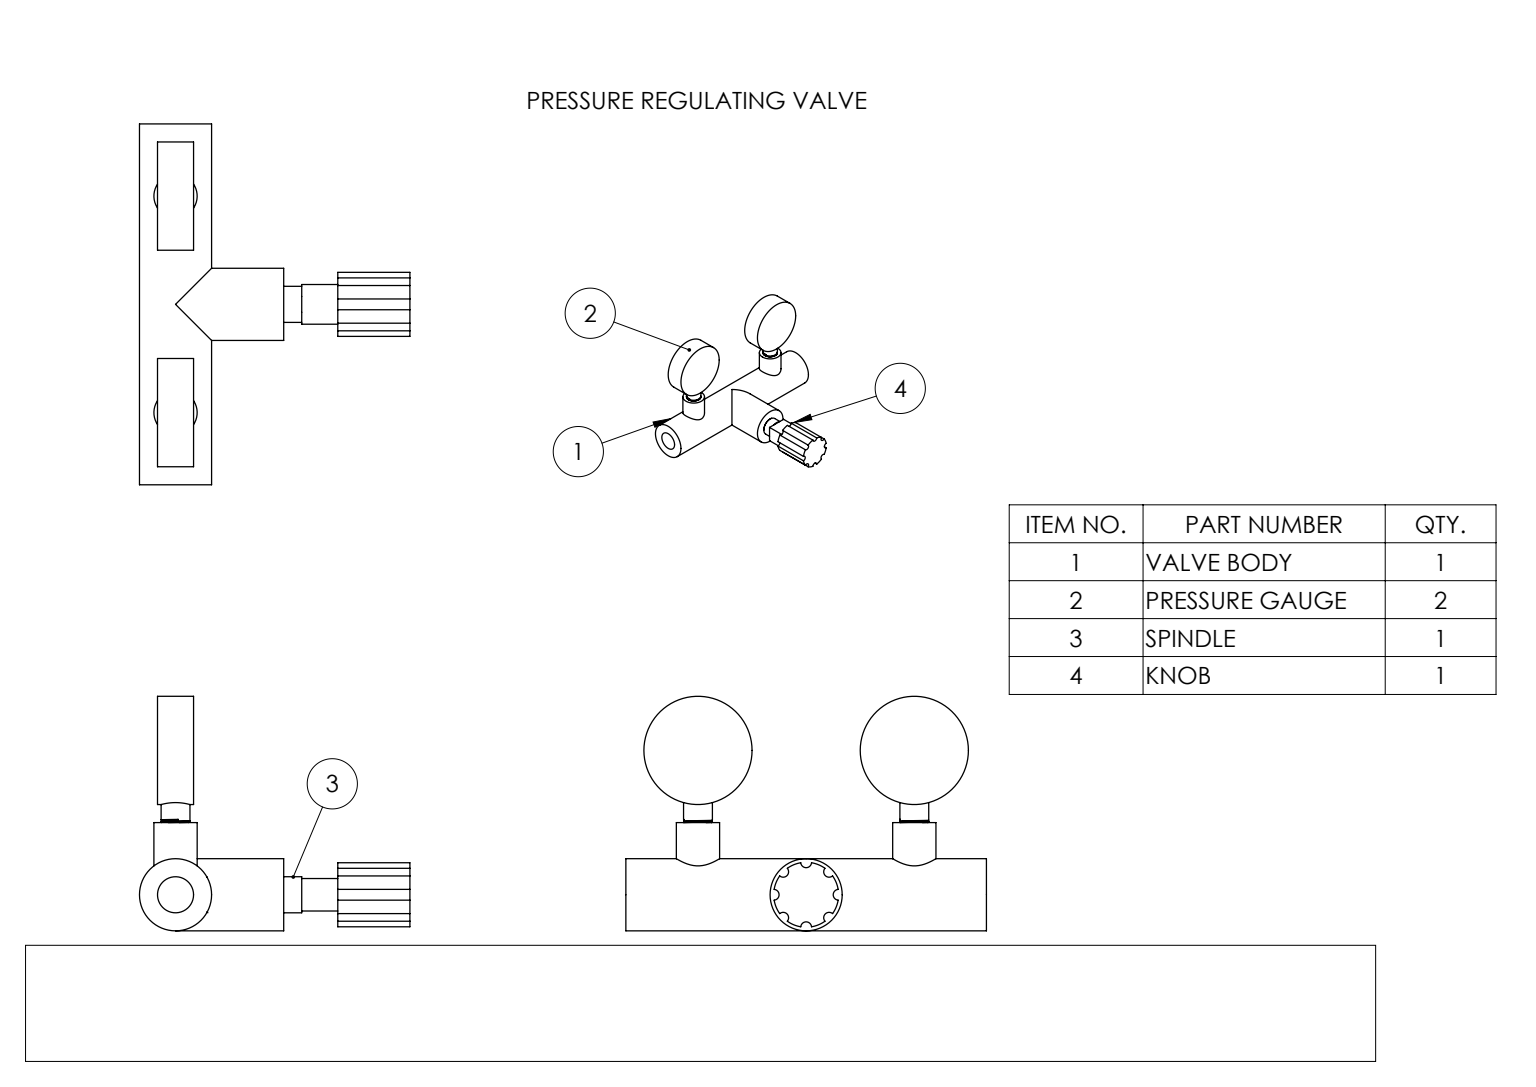
ISO-10303-21;
HEADER;
FILE_DESCRIPTION (('STEP AP214'),
    '1' );
FILE_NAME ('MAS-181',
    '2026-10-26T05:42:23',
    ( '' ),
    ( '' ),
    'SwSTEP 2.0',
    'SolidWorks 2026',
    '' );
FILE_SCHEMA (( 'AUTOMOTIVE_DESIGN' ));
ENDSEC;

DATA;
#1 = CARTESIAN_POINT ( 'NONE',  ( 9.721875000614517148, -6.054752690667223547, -1.112240025338166033E-15 ) ) ;
#2 = CARTESIAN_POINT ( 'NONE',  ( 3.999999999999998668, 14.07500000122903749, -32.30940107675850470 ) ) ;
#3 = CARTESIAN_POINT ( 'NONE',  ( 20.46562500061451928, -6.054752690667223547, -1.112240025338166033E-15 ) ) ;
#4 = CARTESIAN_POINT ( 'NONE',  ( -5.810221930991193690E-16, 14.48749999999999893, 26.00000000000000355 ) ) ;
#5 = CARTESIAN_POINT ( 'NONE',  ( 2.121784821875001281, 17.25312500061459176, 33.67503911421598417 ) ) ;
#6 = CARTESIAN_POINT ( 'NONE',  ( 21.83437500061451786, -4.541064518000419881, 2.621784821874995952 ) ) ;
#7 = CARTESIAN_POINT ( 'NONE',  ( 45.00000000000000000, 0.000000000000000000, 0.000000000000000000 ) ) ;
#8 = CARTESIAN_POINT ( 'NONE',  ( 27.97500000122903074, -5.773502691896255534, -1.060575238724906372E-15 ) ) ;
#9 = CARTESIAN_POINT ( 'NONE',  ( 19.58437500061451786, -2.746126346562642428, -4.756430356249999214 ) ) ;
#10 = CARTESIAN_POINT ( 'NONE',  ( 24.47812500061451502, -4.541064518000419881, 2.621784821874995952 ) ) ;
#11 = CARTESIAN_POINT ( 'NONE',  ( 15.06562500061451537, -6.054752690667223547, -1.112240025338166033E-15 ) ) ;
#12 = CARTESIAN_POINT ( 'NONE',  ( 15.13125000122903252, 4.330127018922191873, 2.499999999999999556 ) ) ;
#13 = CARTESIAN_POINT ( 'NONE',  ( 10.77187500061451786, 3.027376345333613106, -5.243569643749998122 ) ) ;
#14 = CARTESIAN_POINT ( 'NONE',  ( 27.89999999999999858, -4.330127018922190985, -2.500000000000001332 ) ) ;
#15 = CARTESIAN_POINT ( 'NONE',  ( 25.95000000122903216, 5.773502691896255534, 3.535250795749688894E-16 ) ) ;
#16 = CARTESIAN_POINT ( 'NONE',  ( 3.646875000614520079, 6.054752690667223547, 3.707466751127219781E-16 ) ) ;
#17 = CARTESIAN_POINT ( 'NONE',  ( 13.58437500061451786, 4.541064518000418104, 2.621784821874999949 ) ) ;
#18 = CARTESIAN_POINT ( 'NONE',  ( 28.92187500061451644, 3.027376345333611329, 5.243569643749999010 ) ) ;
#19 = CARTESIAN_POINT ( 'NONE',  ( -5.810221930991193690E-16, 12.23750000000000071, -34.00000000000000000 ) ) ;
#20 = ADVANCED_FACE ( 'NONE', ( #69844 ), #24040, .F. ) ;
#21 = CARTESIAN_POINT ( 'NONE',  ( 18.48750000000000071, -2.886751345948126435, -5.000000000000000000 ) ) ;
#22 = CARTESIAN_POINT ( 'NONE',  ( 23.74687500061451573, -3.027376345333610441, -5.243569643749999898 ) ) ;
#23 = CARTESIAN_POINT ( 'NONE',  ( 13.99687500061451928, 6.054752690667223547, 3.707466751127219781E-16 ) ) ;
#24 = CARTESIAN_POINT ( 'NONE',  ( -7.967954043666661671E-16, 16.24062499938548143, 34.33755215474603517 ) ) ;
#25 = CARTESIAN_POINT ( 'NONE',  ( 28.64999999999999858, 0.000000000000000000, 4.999999999999998224 ) ) ;
#26 = CARTESIAN_POINT ( 'NONE',  ( 3.000000001229032875, 5.773502691896255534, 3.535250795749688894E-16 ) ) ;
#27 = CARTESIAN_POINT ( 'NONE',  ( 7.396875000614516082, -4.119189519843965641, -2.378215178125001383 ) ) ;
#28 = CARTESIAN_POINT ( 'NONE',  ( 18.25312500061451715, -4.541064518000417216, -2.621784821875001281 ) ) ;
#29 = CARTESIAN_POINT ( 'NONE',  ( 5.962500000000002132, 2.886751345948129099, -4.999999999999998224 ) ) ;
#30 = CARTESIAN_POINT ( 'NONE',  ( 13.68750000122903288, 6.123233995736764310E-16, -4.999999999999998224 ) ) ;
#31 = CARTESIAN_POINT ( 'NONE',  ( 16.08749999999999503, -2.886751345948129988, 4.999999999999997335 ) ) ;
#32 = CARTESIAN_POINT ( 'NONE',  ( -4.243569643749999898, 13.05312500061451786, 30.00000000000000000 ) ) ;
#33 = CARTESIAN_POINT ( 'NONE',  ( -5.810221930991193690E-16, 11.78749999999999964, 26.00000000000000355 ) ) ;
#34 = CARTESIAN_POINT ( 'NONE',  ( 21.63750000122903572, -4.330127018922194537, 2.499999999999995559 ) ) ;
#35 = FACE_OUTER_BOUND ( 'NONE', #55826, .T. ) ;
#36 = CARTESIAN_POINT ( 'NONE',  ( 26.59687500061451360, 6.054752690667223547, 3.707466751127219781E-16 ) ) ;
#37 = ORIENTED_EDGE ( 'NONE', *, *, #44217, .T. ) ;
#38 = CARTESIAN_POINT ( 'NONE',  ( 14.69062500061451537, -3.027376345333610441, -5.243569643749999898 ) ) ;
#39 = CARTESIAN_POINT ( 'NONE',  ( 22.75312500061451360, -4.541064518000417216, -2.621784821875001281 ) ) ;
#40 = CARTESIAN_POINT ( 'NONE',  ( 22.99687500061451573, 6.054752690667223547, 3.707466751127219781E-16 ) ) ;
#41 = CARTESIAN_POINT ( 'NONE',  ( 6.337499999999998579, -2.886751345948125991, -5.000000000000000000 ) ) ;
#42 = CARTESIAN_POINT ( 'NONE',  ( 8.990625000614516082, 6.054752690667223547, 3.707466751127219781E-16 ) ) ;
#43 = CARTESIAN_POINT ( 'NONE',  ( 24.85312500061451502, 0.000000000000000000, 5.243569643749999010 ) ) ;
#44 = CARTESIAN_POINT ( 'NONE',  ( 14.03437500061451715, 4.541064518000418104, 2.621784821874999949 ) ) ;
#45 = CARTESIAN_POINT ( 'NONE',  ( 18.12187500061451573, 3.027376345333611329, 5.243569643749999010 ) ) ;
#46 = PLANE ( 'NONE',  #66233 ) ;
#47 = CARTESIAN_POINT ( 'NONE',  ( -4.243569643749997233, 17.59062500061451928, 32.45002607614398471 ) ) ;
#48 = CARTESIAN_POINT ( 'NONE',  ( 21.78750000122903074, 6.123233995736764310E-16, -4.999999999999998224 ) ) ;
#49 = CARTESIAN_POINT ( 'NONE',  ( 13.88437500061451679, 5.824947211148865298E-16, -4.756430356249998326 ) ) ;
#50 = CARTESIAN_POINT ( 'NONE',  ( 11.39062500061451644, -3.027376345333614438, 5.243569643749998122 ) ) ;
#51 = CARTESIAN_POINT ( 'NONE',  ( 6.684375000614518392, 6.421520780324663323E-16, -5.243569643749999010 ) ) ;
#52 = CARTESIAN_POINT ( 'NONE',  ( 4.284375000614518925, -4.541064518000419881, 2.621784821874995952 ) ) ;
#53 = ORIENTED_EDGE ( 'NONE', *, *, #36827, .F. ) ;
#54 = CARTESIAN_POINT ( 'NONE',  ( 26.82187500061451857, -6.054752690667223547, -1.112240025338166033E-15 ) ) ;
#55 = CARTESIAN_POINT ( 'NONE',  ( 16.45312500061451289, -4.541064518000417216, -2.621784821875001281 ) ) ;
#56 = CARTESIAN_POINT ( 'NONE',  ( 27.82500000122903572, 2.886751345948126879, 4.999999999999999112 ) ) ;
#57 = CARTESIAN_POINT ( 'NONE',  ( 28.45312500061451289, 0.000000000000000000, 5.243569643749999010 ) ) ;
#58 = CARTESIAN_POINT ( 'NONE',  ( 25.02187500061451431, -6.054752690667223547, -1.112240025338166033E-15 ) ) ;
#59 = CARTESIAN_POINT ( 'NONE',  ( 18.14062500061451644, -3.027376345333614438, 5.243569643749998122 ) ) ;
#60 = CARTESIAN_POINT ( 'NONE',  ( 4.243569643749999010, 19.22187500061452070, 27.54997392385601174 ) ) ;
#61 = CARTESIAN_POINT ( 'NONE',  ( 24.92812500061451431, -4.541064518000419881, 2.621784821874995952 ) ) ;
#62 = CARTESIAN_POINT ( 'NONE',  ( 4.087500001229035007, -4.330127018922194537, 2.499999999999995559 ) ) ;
#63 = ORIENTED_EDGE ( 'NONE', *, *, #30962, .F. ) ;
#64 = CARTESIAN_POINT ( 'NONE',  ( 27.89999999999999858, -4.330127018922190985, -2.500000000000001332 ) ) ;
#65 = CARTESIAN_POINT ( 'NONE',  ( -2.828200636599751609E-16, 15.83750000000000036, -34.61880215351700230 ) ) ;
#66 = CARTESIAN_POINT ( 'NONE',  ( -3.756430356250000102, 17.92812499938548498, 30.00000000000000000 ) ) ;
#67 = CARTESIAN_POINT ( 'NONE',  ( 5.784375000614517148, 6.421520780324663323E-16, -5.243569643749999010 ) ) ;
#68 = CARTESIAN_POINT ( 'NONE',  ( 10.07812500061451644, -4.541064518000419881, 2.621784821874995952 ) ) ;
#69 = CARTESIAN_POINT ( 'NONE',  ( 5.859375000614519102, 4.541064518000418104, -2.621784821874998173 ) ) ;
#70 = CARTESIAN_POINT ( 'NONE',  ( 24.22500000122903430, 2.886751345948126879, 4.999999999999999112 ) ) ;
#71 = CARTESIAN_POINT ( 'NONE',  ( 14.70937500061451786, -4.541064518000417216, -2.621784821875001281 ) ) ;
#72 = CARTESIAN_POINT ( 'NONE',  ( 28.86562500061451786, 3.027376345333611329, 5.243569643749999010 ) ) ;
#73 = CARTESIAN_POINT ( 'NONE',  ( 27.67499999999999716, 4.330127018922191873, 2.499999999999999556 ) ) ;
#74 = EDGE_CURVE ( 'NONE', #45106, #54880, #1431, .T. ) ;
#75 = CARTESIAN_POINT ( 'NONE',  ( 3.065625000614517592, 3.027376345333613106, -5.243569643749998122 ) ) ;
#76 = CARTESIAN_POINT ( 'NONE',  ( 12.92812500061451786, 6.421520780324663323E-16, -5.243569643749999010 ) ) ;
#77 = ORIENTED_EDGE ( 'NONE', *, *, #11122, .T. ) ;
#78 = CARTESIAN_POINT ( 'NONE',  ( 8.953125000614518214, 4.541064518000418104, -2.621784821874998173 ) ) ;
#79 = CARTESIAN_POINT ( 'NONE',  ( 5.203125000614518214, -4.541064518000417216, -2.621784821875001281 ) ) ;
#80 = CARTESIAN_POINT ( 'NONE',  ( 19.88437500061451857, 4.119189519843966529, 2.378215178124999607 ) ) ;
#81 = CARTESIAN_POINT ( 'NONE',  ( 14.10000000122903430, -2.886751345948126435, -5.000000000000000000 ) ) ;
#82 = CARTESIAN_POINT ( 'NONE',  ( 14.66249999999999964, 2.886751345948126879, 4.999999999999999112 ) ) ;
#83 = CARTESIAN_POINT ( 'NONE',  ( 15.90937500061451892, 0.000000000000000000, 5.243569643749999010 ) ) ;
#84 = CARTESIAN_POINT ( 'NONE',  ( 11.36250000122903536, -4.330127018922190985, -2.500000000000001332 ) ) ;
#85 = CARTESIAN_POINT ( 'NONE',  ( 19.46249999999999858, 2.886751345948129099, -4.999999999999998224 ) ) ;
#86 = CARTESIAN_POINT ( 'NONE',  ( 21.72187500061451715, 3.027376345333611329, 5.243569643749999010 ) ) ;
#87 = CARTESIAN_POINT ( 'NONE',  ( -3.000416591977282496E-16, 12.94062500061451537, -34.90005215228797653 ) ) ;
#88 = CARTESIAN_POINT ( 'NONE',  ( -3.999999999999999112, 19.88749999999999929, 27.69059892324149530 ) ) ;
#89 = CARTESIAN_POINT ( 'NONE',  ( 24.45937500061451786, -5.492252693125287522, -1.008910452111647106E-15 ) ) ;
#90 = CARTESIAN_POINT ( 'NONE',  ( 27.62812500061451360, -4.541064518000419881, 2.621784821874995952 ) ) ;
#91 = CARTESIAN_POINT ( 'NONE',  ( 25.05000000000000071, 0.000000000000000000, 4.999999999999998224 ) ) ;
#92 = CARTESIAN_POINT ( 'NONE',  ( 29.82187500061451502, 3.027376345333611329, 5.243569643749999010 ) ) ;
#93 = CARTESIAN_POINT ( 'NONE',  ( 25.38749999999999929, 5.773502691896255534, 3.535250795749688894E-16 ) ) ;
#94 = CARTESIAN_POINT ( 'NONE',  ( 8.465625000614515727, 3.027376345333613106, -5.243569643749998122 ) ) ;
#95 = CARTESIAN_POINT ( 'NONE',  ( 27.64687500061451431, -4.119189519843965641, -2.378215178125001383 ) ) ;
#96 = CARTESIAN_POINT ( 'NONE',  ( 19.09687500061451360, -3.027376345333614438, 5.243569643749998122 ) ) ;
#97 = CARTESIAN_POINT ( 'NONE',  ( 11.07187500061451679, 5.824947211148865298E-16, -4.756430356249998326 ) ) ;
#98 = CARTESIAN_POINT ( 'NONE',  ( 4.603125000614518569, 0.000000000000000000, 5.243569643749999010 ) ) ;
#99 = CARTESIAN_POINT ( 'NONE',  ( 10.69687500061451679, -3.027376345333610441, -5.243569643749999898 ) ) ;
#100 = VERTEX_POINT ( 'NONE', #12957 ) ;
#101 = CARTESIAN_POINT ( 'NONE',  ( 22.28437500061451715, -4.541064518000419881, 2.621784821874995952 ) ) ;
#102 = CARTESIAN_POINT ( 'NONE',  ( -1.071796769724496334, 15.72634618820330310, 26.00000000000000355 ) ) ;
#103 = CARTESIAN_POINT ( 'NONE',  ( 28.42499999999999716, 6.123233995736764310E-16, -4.999999999999998224 ) ) ;
#104 =( BOUNDED_CURVE ( )  B_SPLINE_CURVE ( 2, ( #27084, #21157, #20050, #59212, #14521, #42242, #3825 ),
 .UNSPECIFIED., .F., .F. ) 
 B_SPLINE_CURVE_WITH_KNOTS ( ( 3, 2, 2, 3 ),
 ( 0.5700000000000000622, 0.5733333333333334725, 0.5766666666666667718, 0.5800000000000000711 ),
 .UNSPECIFIED. ) 
 CURVE ( )  GEOMETRIC_REPRESENTATION_ITEM ( )  RATIONAL_B_SPLINE_CURVE ( ( 0.9999999999999955591, 0.8660254037844431485, 1.000000000000000000, 0.8660254037844387076, 1.000000000000000000, 0.8660254037844342667, 1.000000000000004441 ) ) 
 REPRESENTATION_ITEM ( '' )  );
#105 = CARTESIAN_POINT ( 'NONE',  ( 5.887500000000000178, -2.886751345948125991, -5.000000000000000000 ) ) ;
#106 = CARTESIAN_POINT ( 'NONE',  ( 14.36250000122903359, 0.000000000000000000, 4.999999999999998224 ) ) ;
#107 = CARTESIAN_POINT ( 'NONE',  ( 1.999999999999998668, 12.31250000122903465, 26.53589838486224650 ) ) ;
#108 = CARTESIAN_POINT ( 'NONE',  ( 18.67500000000000071, 4.330127018922191873, 2.499999999999999556 ) ) ;
#109 = ORIENTED_EDGE ( 'NONE', *, *, #38380, .F. ) ;
#110 = CARTESIAN_POINT ( 'NONE',  ( 12.15000000000000036, -4.330127018922190985, -2.500000000000001332 ) ) ;
#111 = CARTESIAN_POINT ( 'NONE',  ( 26.84062500061451573, -3.027376345333610441, -5.243569643749999898 ) ) ;
#112 = CARTESIAN_POINT ( 'NONE',  ( 16.19999999999999929, -4.330127018922190985, -2.500000000000001332 ) ) ;
#113 = ADVANCED_FACE ( 'NONE', ( #65026 ), #30323, .F. ) ;
#114 = CARTESIAN_POINT ( 'NONE',  ( 10.20000000122903572, 5.773502691896255534, 3.535250795749688894E-16 ) ) ;
#115 = CARTESIAN_POINT ( 'NONE',  ( 8.128125000614515372, 4.541064518000418104, 2.621784821874999949 ) ) ;
#116 = CARTESIAN_POINT ( 'NONE',  ( 9.225000000000001421, 4.330127018922191873, 2.499999999999999556 ) ) ;
#117 = FACE_OUTER_BOUND ( 'NONE', #13285, .T. ) ;
#118 = CARTESIAN_POINT ( 'NONE',  ( 4.243569643749999010, 15.17187500061451644, -32.45002607614398471 ) ) ;
#119 = CARTESIAN_POINT ( 'NONE',  ( 27.00000000122903288, -2.886751345948129988, 4.999999999999997335 ) ) ;
#120 = CARTESIAN_POINT ( 'NONE',  ( 3.756430356250000546, 13.57812499938548711, 27.83122392262697886 ) ) ;
#121 = CARTESIAN_POINT ( 'NONE',  ( 7.162500000000001421, -5.773502691896255534, -1.060575238724906372E-15 ) ) ;
#122 = DIRECTION ( 'NONE',  ( 0.000000000000000000, 0.000000000000000000, -1.000000000000000000 ) ) ;
#123 = ORIENTED_EDGE ( 'NONE', *, *, #29254, .F. ) ;
#124 = CARTESIAN_POINT ( 'NONE',  ( 25.04062500061451502, -3.027376345333610441, -5.243569643749999898 ) ) ;
#125 = CARTESIAN_POINT ( 'NONE',  ( 14.88750000122903394, -4.330127018922194537, 2.499999999999995559 ) ) ;
#126 = CARTESIAN_POINT ( 'NONE',  ( 29.57812500061451644, 6.421520780324663323E-16, -5.243569643749999010 ) ) ;
#127 = CARTESIAN_POINT ( 'NONE',  ( 28.62187500061451573, -6.054752690667223547, -1.112240025338166033E-15 ) ) ;
#128 = CARTESIAN_POINT ( 'NONE',  ( 18.87187500061451573, 3.027376345333613106, -5.243569643749998122 ) ) ;
#129 = CARTESIAN_POINT ( 'NONE',  ( 16.49062500061451786, -3.027376345333610441, -5.243569643749999898 ) ) ;
#130 = CARTESIAN_POINT ( 'NONE',  ( -4.243569643749998122, 10.39062500061459460, -27.54997392385601174 ) ) ;
#131 = CARTESIAN_POINT ( 'NONE',  ( 5.990625000614517859, -3.027376345333614438, 5.243569643749998122 ) ) ;
#132 = CARTESIAN_POINT ( 'NONE',  ( 29.28750000122903074, -4.330127018922194537, 2.499999999999995559 ) ) ;
#133 = CARTESIAN_POINT ( 'NONE',  ( 22.35937500061451644, -4.119189519843965641, -2.378215178125001383 ) ) ;
#134 = CARTESIAN_POINT ( 'NONE',  ( 19.19062500061452070, -3.027376345333610441, -5.243569643749999898 ) ) ;
#135 = CARTESIAN_POINT ( 'NONE',  ( 1.878215178125000495, 19.01562499938548356, 26.74683588394047007 ) ) ;
#136 = CARTESIAN_POINT ( 'NONE',  ( 13.39687500061451608, -3.027376345333610441, -5.243569643749999898 ) ) ;
#137 = CARTESIAN_POINT ( 'NONE',  ( 11.14687500061451608, -3.027376345333610441, -5.243569643749999898 ) ) ;
#138 = CARTESIAN_POINT ( 'NONE',  ( 23.59687500061451715, -3.027376345333614438, 5.243569643749998122 ) ) ;
#139 = ORIENTED_EDGE ( 'NONE', *, *, #5292, .F. ) ;
#140 = CARTESIAN_POINT ( 'NONE',  ( 3.290625000614516793, -3.027376345333614438, 5.243569643749998122 ) ) ;
#141 = CARTESIAN_POINT ( 'NONE',  ( 27.40312500061451573, 4.541064518000418104, -2.621784821874998173 ) ) ;
#142 =( BOUNDED_CURVE ( )  B_SPLINE_CURVE ( 2, ( #31020, #38022, #48390, #19556, #9951, #32488, #65735 ),
 .UNSPECIFIED., .F., .F. ) 
 B_SPLINE_CURVE_WITH_KNOTS ( ( 3, 2, 2, 3 ),
 ( 0.6416666666666668295, 0.6444444444444445974, 0.6472222222222223653, 0.6500000000000001332 ),
 .UNSPECIFIED. ) 
 CURVE ( )  GEOMETRIC_REPRESENTATION_ITEM ( )  RATIONAL_B_SPLINE_CURVE ( ( 0.9999999999999946709, 0.8660254037844440367, 1.000000000000000000, 0.8660254037844387076, 1.000000000000000000, 0.8660254037844333785, 1.000000000000005329 ) ) 
 REPRESENTATION_ITEM ( '' )  );
#143 = CARTESIAN_POINT ( 'NONE',  ( 27.55312500061451786, 0.000000000000000000, 5.243569643749999010 ) ) ;
#144 = CARTESIAN_POINT ( 'NONE',  ( 4.000000000000000000, 12.08750000000000036, -27.69059892324149885 ) ) ;
#145 = CARTESIAN_POINT ( 'NONE',  ( -2.828200636599751609E-16, 16.73750000000000071, 25.38119784648299770 ) ) ;
#146 = CARTESIAN_POINT ( 'NONE',  ( 4.021875000614516082, 3.027376345333613106, -5.243569643749998122 ) ) ;
#147 = CARTESIAN_POINT ( 'NONE',  ( 11.58750000122903501, 4.330127018922191873, 2.499999999999999556 ) ) ;
#148 = CARTESIAN_POINT ( 'NONE',  ( 7.987500001229032698, 4.330127018922191873, 2.499999999999999556 ) ) ;
#149 = CARTESIAN_POINT ( 'NONE',  ( 28.50000000122903288, -2.886751345948125991, -5.000000000000000000 ) ) ;
#150 = CARTESIAN_POINT ( 'NONE',  ( 2.828200636599751609E-16, 18.40624999877096712, 25.38119784648299415 ) ) ;
#151 = CARTESIAN_POINT ( 'NONE',  ( 17.30625000122903145, 4.330127018922192761, -2.499999999999997780 ) ) ;
#152 = CARTESIAN_POINT ( 'NONE',  ( 11.78437500061451892, 4.541064518000418104, 2.621784821874999949 ) ) ;
#153 = CARTESIAN_POINT ( 'NONE',  ( -3.999999999999999112, 17.58124999877096428, 27.69059892324149530 ) ) ;
#154 = CARTESIAN_POINT ( 'NONE',  ( 20.31562500061451715, 3.027376345333611329, 5.243569643749999010 ) ) ;
#155 = CARTESIAN_POINT ( 'NONE',  ( 13.95937500061451786, 4.541064518000418104, -2.621784821874998173 ) ) ;
#156 = CARTESIAN_POINT ( 'NONE',  ( 3.778125000614519280, -4.541064518000419881, 2.621784821874995952 ) ) ;
#157 = CARTESIAN_POINT ( 'NONE',  ( 23.33437500061451786, 6.421520780324663323E-16, -5.243569643749999010 ) ) ;
#158 = CARTESIAN_POINT ( 'NONE',  ( 8.746875000614515727, -3.027376345333614438, 5.243569643749998122 ) ) ;
#159 = CARTESIAN_POINT ( 'NONE',  ( 4.565625000614516260, 3.027376345333611329, 5.243569643749999010 ) ) ;
#160 = CARTESIAN_POINT ( 'NONE',  ( 5.812500000000001776, -5.773502691896255534, -1.060575238724906372E-15 ) ) ;
#161 = CARTESIAN_POINT ( 'NONE',  ( 5.850000001229035185, -2.886751345948129988, 4.999999999999997335 ) ) ;
#162 = CARTESIAN_POINT ( 'NONE',  ( 19.82812500061451644, 4.541064518000418104, 2.621784821874999949 ) ) ;
#163 = EDGE_CURVE ( 'NONE', #39643, #7983, #64627, .T. ) ;
#164 = CARTESIAN_POINT ( 'NONE',  ( 9.000000001229034652, -2.886751345948129988, 4.999999999999997335 ) ) ;
#165 =( BOUNDED_CURVE ( )  B_SPLINE_CURVE ( 2, ( #55772, #22147, #62756, #34675, #57203, #6619, #72393 ),
 .UNSPECIFIED., .F., .F. ) 
 B_SPLINE_CURVE_WITH_KNOTS ( ( 3, 2, 2, 3 ),
 ( 0.06666666666666665186, 0.06944444444444443365, 0.07222222222222218768, 0.07499999999999996947 ),
 .UNSPECIFIED. ) 
 CURVE ( )  GEOMETRIC_REPRESENTATION_ITEM ( )  RATIONAL_B_SPLINE_CURVE ( ( 1.000000000000000666, 0.8660254037844379305, 1.000000000000000000, 0.8660254037844387076, 1.000000000000000000, 0.8660254037844400399, 0.9999999999999986677 ) ) 
 REPRESENTATION_ITEM ( '' )  );
#166 = CARTESIAN_POINT ( 'NONE',  ( 18.47812500061451857, 4.541064518000418104, 2.621784821874999949 ) ) ;
#167 = CARTESIAN_POINT ( 'NONE',  ( 14.35312500061451679, 4.541064518000418104, -2.621784821874998173 ) ) ;
#168 = CARTESIAN_POINT ( 'NONE',  ( 26.67187500061451644, 2.746126346562643317, 4.756430356249998326 ) ) ;
#169 = CARTESIAN_POINT ( 'NONE',  ( 12.71250000000000036, 2.886751345948129099, -4.999999999999998224 ) ) ;
#170 = CARTESIAN_POINT ( 'NONE',  ( 10.16250000122903252, 4.330127018922192761, -2.499999999999997780 ) ) ;
#171 = CARTESIAN_POINT ( 'NONE',  ( 4.603125000614518569, 0.000000000000000000, 5.243569643749999010 ) ) ;
#172 = CARTESIAN_POINT ( 'NONE',  ( 21.45000000122903216, 5.773502691896255534, 3.535250795749688894E-16 ) ) ;
#173 = CARTESIAN_POINT ( 'NONE',  ( 26.25000000000000000, 4.330127018922192761, -2.499999999999997780 ) ) ;
#174 = CARTESIAN_POINT ( 'NONE',  ( 4.243569643749999898, 11.08437500061451786, -30.00000000000000000 ) ) ;
#175 = CARTESIAN_POINT ( 'NONE',  ( 5.587500001229033231, 6.123233995736764310E-16, -4.999999999999998224 ) ) ;
#176 = CARTESIAN_POINT ( 'NONE',  ( 24.07499999999999929, 4.330127018922191873, 2.499999999999999556 ) ) ;
#177 = CARTESIAN_POINT ( 'NONE',  ( 6.487499999999999822, 5.773502691896255534, 3.535250795749688401E-16 ) ) ;
#178 = CARTESIAN_POINT ( 'NONE',  ( 21.38437500061451502, -4.541064518000419881, 2.621784821874995952 ) ) ;
#179 = CARTESIAN_POINT ( 'NONE',  ( 1.999999999999998668, 18.61250000122903359, 26.53589838486224650 ) ) ;
#180 = CARTESIAN_POINT ( 'NONE',  ( 16.34062500061451573, -3.027376345333614438, 5.243569643749998122 ) ) ;
#181 = CARTESIAN_POINT ( 'NONE',  ( 11.11875000122903323, 2.886751345948126879, 4.999999999999999112 ) ) ;
#182 = CARTESIAN_POINT ( 'NONE',  ( 13.19999999999999929, 4.330127018922192761, -2.499999999999997780 ) ) ;
#183 = CARTESIAN_POINT ( 'NONE',  ( -1.071796769724492115, 14.61740381056766402, 34.00000000000000000 ) ) ;
#184 = CARTESIAN_POINT ( 'NONE',  ( 27.12187500061451573, 3.027376345333611329, 5.243569643749999010 ) ) ;
#185 = CARTESIAN_POINT ( 'NONE',  ( 21.27187500061451431, -4.119189519843968306, 2.378215178124996054 ) ) ;
#186 = CARTESIAN_POINT ( 'NONE',  ( 11.54062500061451857, -3.027376345333610441, -5.243569643749999898 ) ) ;
#187 = CARTESIAN_POINT ( 'NONE',  ( 11.67187500061451821, 3.027376345333613106, -5.243569643749998122 ) ) ;
#188 = ORIENTED_EDGE ( 'NONE', *, *, #4935, .T. ) ;
#189 = CARTESIAN_POINT ( 'NONE',  ( -1.999999999999997113, 14.22500000000000142, -26.53589838486224295 ) ) ;
#190 = CARTESIAN_POINT ( 'NONE',  ( 23.54062500061451146, -3.027376345333614438, 5.243569643749998122 ) ) ;
#191 = CARTESIAN_POINT ( 'NONE',  ( 1.071796769724489895, 13.22990381179669939, -34.00000000000000000 ) ) ;
#192 = CARTESIAN_POINT ( 'NONE',  ( 10.74375000122903323, -2.886751345948130876, 4.999999999999996447 ) ) ;
#193 = CARTESIAN_POINT ( 'NONE',  ( 12.00000000000000000, 0.000000000000000000, 4.999999999999998224 ) ) ;
#194 = CARTESIAN_POINT ( 'NONE',  ( 22.72500000122903430, 2.886751345948129099, -4.999999999999998224 ) ) ;
#195 = CARTESIAN_POINT ( 'NONE',  ( 15.70312500061451644, 4.541064518000418104, -2.621784821874998173 ) ) ;
#196 = CARTESIAN_POINT ( 'NONE',  ( 13.05937500061451573, 2.746126346562643317, 4.756430356249998326 ) ) ;
#197 = ORIENTED_EDGE ( 'NONE', *, *, #67048, .T. ) ;
#198 = CARTESIAN_POINT ( 'NONE',  ( 19.98749999999999716, 5.773502691896255534, 3.535250795749688894E-16 ) ) ;
#199 = CARTESIAN_POINT ( 'NONE',  ( 24.78750000000000497, -2.886751345948125991, -5.000000000000000000 ) ) ;
#200 = CARTESIAN_POINT ( 'NONE',  ( 21.42187500061451644, -6.054752690667223547, -1.112240025338166033E-15 ) ) ;
#201 = CARTESIAN_POINT ( 'NONE',  ( 26.20312500061451644, 0.000000000000000000, 5.243569643749999010 ) ) ;
#202 = ORIENTED_EDGE ( 'NONE', *, *, #63479, .F. ) ;
#203 = LINE ( 'NONE', #67793, #8872 ) ;
#204 = CARTESIAN_POINT ( 'NONE',  ( 8.728125000614518569, -4.541064518000419881, 2.621784821874995952 ) ) ;
#205 = CARTESIAN_POINT ( 'NONE',  ( 17.40000000122903145, 5.773502691896255534, 3.535250795749688401E-16 ) ) ;
#206 = CARTESIAN_POINT ( 'NONE',  ( 14.40000000000000036, -4.330127018922190985, -2.500000000000001332 ) ) ;
#207 = CARTESIAN_POINT ( 'NONE',  ( 2.121784821874999061, 17.85312500061451502, 26.32496088578401583 ) ) ;
#208 = CARTESIAN_POINT ( 'NONE',  ( 4.171875000614517326, 3.027376345333611329, 5.243569643749999010 ) ) ;
#209 = CARTESIAN_POINT ( 'NONE',  ( 27.30937500061451573, -4.541064518000417216, -2.621784821875001281 ) ) ;
#210 = ORIENTED_EDGE ( 'NONE', *, *, #33045, .F. ) ;
#211 = CARTESIAN_POINT ( 'NONE',  ( 24.70312500061451644, 4.541064518000418104, -2.621784821874998173 ) ) ;
#212 = CARTESIAN_POINT ( 'NONE',  ( 25.05937500061451573, -4.541064518000417216, -2.621784821875001281 ) ) ;
#213 = CARTESIAN_POINT ( 'NONE',  ( 4.243569643749999898, 19.57812500061459460, -30.00000000000000000 ) ) ;
#214 = CARTESIAN_POINT ( 'NONE',  ( 10.49999999999999822, 4.330127018922192761, -2.499999999999997780 ) ) ;
#215 = CARTESIAN_POINT ( 'NONE',  ( 9.478125000614515017, 4.541064518000418104, 2.621784821874999949 ) ) ;
#216 = CYLINDRICAL_SURFACE ( 'NONE', #71725, 4.000000000000000000 ) ;
#217 = CARTESIAN_POINT ( 'NONE',  ( 13.57500000000000107, 6.123233995736764310E-16, -4.999999999999998224 ) ) ;
#218 = CARTESIAN_POINT ( 'NONE',  ( 27.44062500061451715, 6.054752690667223547, 3.707466751127219781E-16 ) ) ;
#219 = CARTESIAN_POINT ( 'NONE',  ( 29.29687500061451644, 0.000000000000000000, 4.756430356249998326 ) ) ;
#220 = CARTESIAN_POINT ( 'NONE',  ( 12.38437500061451857, -4.119189519843968306, 2.378215178124996054 ) ) ;
#221 = CARTESIAN_POINT ( 'NONE',  ( 3.665625000614517681, 3.027376345333611329, 5.243569643749999010 ) ) ;
#222 = CARTESIAN_POINT ( 'NONE',  ( 19.39687500061451786, 6.054752690667223547, 3.707466751127219781E-16 ) ) ;
#223 = CARTESIAN_POINT ( 'NONE',  ( 9.001249775931846008E-16, 14.57187500061451679, 34.90005215228797653 ) ) ;
#224 = CARTESIAN_POINT ( 'NONE',  ( 19.65937500061451360, -4.541064518000417216, -2.621784821875001281 ) ) ;
#225 = CARTESIAN_POINT ( 'NONE',  ( 29.55937500061451573, -4.541064518000417216, -2.621784821875001281 ) ) ;
#226 = CARTESIAN_POINT ( 'NONE',  ( -4.243569643749999898, 18.47187500061451715, 27.54997392385601529 ) ) ;
#227 = CARTESIAN_POINT ( 'NONE',  ( 10.19062500061451892, -3.027376345333610441, -5.243569643749999898 ) ) ;
#228 = CARTESIAN_POINT ( 'NONE',  ( 3.112500001229034918, 0.000000000000000000, 4.999999999999998224 ) ) ;
#229 = CARTESIAN_POINT ( 'NONE',  ( 7.846875000614518036, -3.027376345333614438, 5.243569643749998122 ) ) ;
#230 = CARTESIAN_POINT ( 'NONE',  ( 16.16250000122903430, 0.000000000000000000, 4.999999999999998224 ) ) ;
#231 = CARTESIAN_POINT ( 'NONE',  ( 8.165625000614516793, 3.027376345333611329, 5.243569643749999010 ) ) ;
#232 = CARTESIAN_POINT ( 'NONE',  ( 11.22187500061451892, 3.027376345333613106, -5.243569643749998122 ) ) ;
#233 = CARTESIAN_POINT ( 'NONE',  ( 18.90000000122902790, -2.886751345948129988, 4.999999999999997335 ) ) ;
#234 = CARTESIAN_POINT ( 'NONE',  ( 8.446875000614518569, -3.027376345333610441, -5.243569643749999898 ) ) ;
#235 = CARTESIAN_POINT ( 'NONE',  ( 9.815625000614518925, 3.027376345333613106, -5.243569643749998122 ) ) ;
#236 = CARTESIAN_POINT ( 'NONE',  ( 5.803125000614517859, 4.541064518000418104, -2.621784821874998173 ) ) ;
#237 = CARTESIAN_POINT ( 'NONE',  ( 23.26875000122903003, 2.886751345948126879, 4.999999999999999112 ) ) ;
#238 = CARTESIAN_POINT ( 'NONE',  ( 20.25937500061451857, 4.541064518000418104, -2.621784821874998173 ) ) ;
#239 = CARTESIAN_POINT ( 'NONE',  ( -5.810221930991193690E-16, 13.25000000122903465, 26.00000000000000355 ) ) ;
#240 = CARTESIAN_POINT ( 'NONE',  ( 26.39062500061451644, -3.027376345333610441, -5.243569643749999898 ) ) ;
#241 = CARTESIAN_POINT ( 'NONE',  ( 12.02812500061451573, 6.421520780324663323E-16, -5.243569643749999010 ) ) ;
#242 = CARTESIAN_POINT ( 'NONE',  ( 28.99687500061451573, -3.027376345333614438, 5.243569643749998122 ) ) ;
#243 = CARTESIAN_POINT ( 'NONE',  ( 2.121784821874999061, 10.25937500061451857, -33.67503911421598417 ) ) ;
#244 = CARTESIAN_POINT ( 'NONE',  ( 12.78750000122903430, 6.123233995736764310E-16, -4.999999999999998224 ) ) ;
#245 = CARTESIAN_POINT ( 'NONE',  ( 28.19062500061451715, -3.027376345333610441, -5.243569643749999898 ) ) ;
#246 = ADVANCED_FACE ( 'NONE', ( #36587 ), #41411, .F. ) ;
#247 = CARTESIAN_POINT ( 'NONE',  ( -2.121784821874999949, 15.22812500061451679, -33.67503911421598417 ) ) ;
#248 = CARTESIAN_POINT ( 'NONE',  ( 15.22500000122903252, 2.886751345948126879, 4.999999999999999112 ) ) ;
#249 = CARTESIAN_POINT ( 'NONE',  ( 13.68750000000000178, 5.773502691896255534, 3.535250795749688894E-16 ) ) ;
#250 = CARTESIAN_POINT ( 'NONE',  ( 21.62812500061451360, 4.541064518000418104, 2.621784821874999949 ) ) ;
#251 = CARTESIAN_POINT ( 'NONE',  ( 8.184375000614515727, 4.541064518000418104, 2.621784821874999949 ) ) ;
#252 = CARTESIAN_POINT ( 'NONE',  ( 7.912500001229033408, 4.330127018922192761, -2.499999999999997780 ) ) ;
#253 = CARTESIAN_POINT ( 'NONE',  ( 17.25000000122903288, -2.886751345948125991, -5.000000000000000000 ) ) ;
#254 = CARTESIAN_POINT ( 'NONE',  ( 13.04062500061451502, 6.054752690667223547, 3.707466751127219781E-16 ) ) ;
#255 = CARTESIAN_POINT ( 'NONE',  ( 16.04062500061451857, -3.027376345333610441, -5.243569643749999898 ) ) ;
#256 = CARTESIAN_POINT ( 'NONE',  ( 27.56250000122902932, -4.330127018922190985, -2.500000000000001332 ) ) ;
#257 = CARTESIAN_POINT ( 'NONE',  ( 21.93750000000000000, -2.886751345948129988, 4.999999999999997335 ) ) ;
#258 = CARTESIAN_POINT ( 'NONE',  ( 24.15937500061451715, -4.541064518000417216, -2.621784821875001281 ) ) ;
#259 = DIRECTION ( 'NONE',  ( -0.000000000000000000, -1.000000000000000000, -0.000000000000000000 ) ) ;
#260 = CARTESIAN_POINT ( 'NONE',  ( 10.42500000122903536, -5.773502691896255534, -1.060575238724906372E-15 ) ) ;
#261 = CARTESIAN_POINT ( 'NONE',  ( 28.28437500061451715, 6.421520780324663323E-16, -5.243569643749999010 ) ) ;
#262 = CARTESIAN_POINT ( 'NONE',  ( 5.146875000614517859, -3.027376345333614438, 5.243569643749998122 ) ) ;
#263 = CARTESIAN_POINT ( 'NONE',  ( 24.59062500061451573, -3.027376345333610441, -5.243569643749999898 ) ) ;
#264 = CARTESIAN_POINT ( 'NONE',  ( -7.967954043666661671E-16, 14.44062499938548250, 34.33755215474603517 ) ) ;
#265 = CARTESIAN_POINT ( 'NONE',  ( -1.999999999999999112, 13.94374999877096677, 26.53589838486224650 ) ) ;
#266 = CARTESIAN_POINT ( 'NONE',  ( 10.69687500061451679, -3.027376345333610441, -5.243569643749999898 ) ) ;
#267 = CARTESIAN_POINT ( 'NONE',  ( 3.999999999999998668, 12.61250000000000249, 27.69059892324149530 ) ) ;
#268 = CARTESIAN_POINT ( 'NONE',  ( 29.09062500061451573, -3.027376345333610441, -5.243569643749999898 ) ) ;
#269 = CARTESIAN_POINT ( 'NONE',  ( 7.321875000614516793, 3.027376345333611329, 5.243569643749999010 ) ) ;
#270 = CARTESIAN_POINT ( 'NONE',  ( 6.825000000000001066, 6.123233995736764310E-16, -4.999999999999998224 ) ) ;
#271 = CARTESIAN_POINT ( 'NONE',  ( 25.24687500061451573, 6.054752690667223547, 3.707466751127219781E-16 ) ) ;
#272 = CARTESIAN_POINT ( 'NONE',  ( 2.121784821874999061, 10.65312500061459566, 26.32496088578401583 ) ) ;
#273 = CARTESIAN_POINT ( 'NONE',  ( 18.56250000000000000, 2.886751345948129099, -4.999999999999998224 ) ) ;
#274 = EDGE_LOOP ( 'NONE', ( #54307, #37100, #57406 ) ) ;
#275 = CARTESIAN_POINT ( 'NONE',  ( 26.84999999999999787, 0.000000000000000000, 4.999999999999998224 ) ) ;
#276 =( BOUNDED_CURVE ( )  B_SPLINE_CURVE ( 2, ( #33865, #44247, #5440, #72677, #27980, #66778, #16868, #50510, #73036 ),
 .UNSPECIFIED., .F., .F. ) 
 B_SPLINE_CURVE_WITH_KNOTS ( ( 3, 2, 2, 2, 3 ),
 ( 0.2916666666666666852, 0.2962962962962962798, 0.3055555555555555802, 0.3148148148148148251, 0.3194444444444444753 ),
 .UNSPECIFIED. ) 
 CURVE ( )  GEOMETRIC_REPRESENTATION_ITEM ( )  RATIONAL_B_SPLINE_CURVE ( ( 0.9330127018922194093, 0.9330127018922197424, 1.000000000000000000, 0.8660254037844387076, 1.000000000000000000, 0.8660254037844387076, 1.000000000000000000, 0.9330127018922189652, 0.9330127018922194093 ) ) 
 REPRESENTATION_ITEM ( '' )  );
#277 = CARTESIAN_POINT ( 'NONE',  ( 28.99687500061451573, -3.027376345333614438, 5.243569643749998122 ) ) ;
#278 = ADVANCED_FACE ( 'NONE', ( #72396 ), #26980, .F. ) ;
#279 = EDGE_LOOP ( 'NONE', ( #33564, #50876, #16388, #71740 ) ) ;
#280 = CARTESIAN_POINT ( 'NONE',  ( 16.45312500061451289, -4.541064518000417216, -2.621784821875001281 ) ) ;
#281 = CARTESIAN_POINT ( 'NONE',  ( 7.565625000614518036, 3.027376345333613106, -5.243569643749998122 ) ) ;
#282 = CARTESIAN_POINT ( 'NONE',  ( 17.89687500061451431, 4.119189519843966529, -2.378215178124998275 ) ) ;
#283 = CARTESIAN_POINT ( 'NONE',  ( 5.821875000614519458, 3.027376345333613106, -5.243569643749998122 ) ) ;
#284 = CARTESIAN_POINT ( 'NONE',  ( 18.93750000122903288, -4.330127018922194537, 2.499999999999995559 ) ) ;
#285 = CARTESIAN_POINT ( 'NONE',  ( 22.64999999999999858, 4.330127018922192761, -2.499999999999997780 ) ) ;
#286 = CARTESIAN_POINT ( 'NONE',  ( 3.275492200589926739, -3.777717676570560901, -3.275492200590059078 ) ) ;
#287 = CARTESIAN_POINT ( 'NONE',  ( 7.734375000614517326, 4.541064518000418104, 2.621784821874999949 ) ) ;
#288 = CARTESIAN_POINT ( 'NONE',  ( 12.60937500061451821, 4.541064518000418104, -2.621784821874998173 ) ) ;
#289 = CARTESIAN_POINT ( 'NONE',  ( 21.60937500061451644, 4.541064518000418104, -2.621784821874998173 ) ) ;
#290 = CARTESIAN_POINT ( 'NONE',  ( -5.810221930991193690E-16, 14.48749999999999893, -34.00000000000000000 ) ) ;
#291 = ORIENTED_EDGE ( 'NONE', *, *, #26409, .F. ) ;
#292 = CARTESIAN_POINT ( 'NONE',  ( 3.909375000614518481, -4.541064518000417216, -2.621784821875001281 ) ) ;
#293 = CARTESIAN_POINT ( 'NONE',  ( 7.696875000614516793, 6.054752690667223547, 3.707466751127219781E-16 ) ) ;
#294 = CARTESIAN_POINT ( 'NONE',  ( 19.46249999999999858, 2.886751345948129099, -4.999999999999998224 ) ) ;
#295 = CARTESIAN_POINT ( 'NONE',  ( 15.06562500061451537, -6.054752690667223547, -1.112240025338166033E-15 ) ) ;
#296 = CARTESIAN_POINT ( 'NONE',  ( -1.999999999999999112, 17.60000000000000142, 26.53589838486224650 ) ) ;
#297 = CARTESIAN_POINT ( 'NONE',  ( 18.22499999999999787, 4.330127018922191873, 2.499999999999999556 ) ) ;
#298 = CARTESIAN_POINT ( 'NONE',  ( 19.05937500061451928, 0.000000000000000000, 4.756430356249998326 ) ) ;
#299 = CARTESIAN_POINT ( 'NONE',  ( 10.90312500061451928, 0.000000000000000000, 5.243569643749999010 ) ) ;
#300 = CARTESIAN_POINT ( 'NONE',  ( 26.89687500061451431, -3.027376345333610441, -5.243569643749999898 ) ) ;
#301 = CARTESIAN_POINT ( 'NONE',  ( 27.90937500061451715, 4.541064518000418104, -2.621784821874998173 ) ) ;
#302 = CARTESIAN_POINT ( 'NONE',  ( 9.750000000000001776, 0.000000000000000000, 4.999999999999998224 ) ) ;
#303 = CARTESIAN_POINT ( 'NONE',  ( -3.999999999999999112, 16.06250000122903288, 30.00000000000000000 ) ) ;
#304 = CARTESIAN_POINT ( 'NONE',  ( 8.475000001229034297, 2.886751345948126879, 4.999999999999999112 ) ) ;
#305 = CARTESIAN_POINT ( 'NONE',  ( 20.63437500061451857, 6.421520780324663323E-16, -5.243569643749999010 ) ) ;
#306 = CARTESIAN_POINT ( 'NONE',  ( 14.70937500061451786, -4.541064518000417216, -2.621784821875001281 ) ) ;
#307 = CARTESIAN_POINT ( 'NONE',  ( 9.999999999999992895, 5.857864376269048989, 9.999999999999992895 ) ) ;
#308 = EDGE_LOOP ( 'NONE', ( #45837, #56679, #50706, #57678 ) ) ;
#309 = CARTESIAN_POINT ( 'NONE',  ( 13.97812500061451679, 4.541064518000418104, 2.621784821874999949 ) ) ;
#310 = CARTESIAN_POINT ( 'NONE',  ( 27.00000000122903288, -2.886751345948129988, 4.999999999999997335 ) ) ;
#311 = CARTESIAN_POINT ( 'NONE',  ( 15.38437500061451679, 4.541064518000418104, 2.621784821874999949 ) ) ;
#312 = CARTESIAN_POINT ( 'NONE',  ( 3.440625000614518036, -3.027376345333610441, -5.243569643749999898 ) ) ;
#313 = CARTESIAN_POINT ( 'NONE',  ( 17.42812500061451786, 6.421520780324663323E-16, -5.243569643749999010 ) ) ;
#314 = ADVANCED_FACE ( 'NONE', ( #9615 ), #38044, .F. ) ;
#315 = FACE_OUTER_BOUND ( 'NONE', #42185, .T. ) ;
#316 = CARTESIAN_POINT ( 'NONE',  ( 25.92187500061451999, -6.054752690667223547, -1.112240025338166033E-15 ) ) ;
#317 = CARTESIAN_POINT ( 'NONE',  ( 2.121784821874999061, 11.10312500061451679, 26.32496088578401583 ) ) ;
#318 = CARTESIAN_POINT ( 'NONE',  ( 16.28437500061452070, 4.541064518000418104, 2.621784821874999949 ) ) ;
#319 = CARTESIAN_POINT ( 'NONE',  ( 13.01250000122903394, 0.000000000000000000, 4.999999999999998224 ) ) ;
#320 = CARTESIAN_POINT ( 'NONE',  ( 30.00000000000000000, 0.000000000000000000, 0.000000000000000000 ) ) ;
#321 = CARTESIAN_POINT ( 'NONE',  ( -2.121784821874999949, 19.78437500061451715, -33.67503911421598417 ) ) ;
#322 = CARTESIAN_POINT ( 'NONE',  ( 18.87187500061451573, 3.027376345333613106, -5.243569643749998122 ) ) ;
#323 = CARTESIAN_POINT ( 'NONE',  ( 19.87500000122903288, -5.773502691896255534, -1.060575238724906372E-15 ) ) ;
#324 = CARTESIAN_POINT ( 'NONE',  ( 14.89687500061451786, 6.054752690667223547, 3.707466751127219781E-16 ) ) ;
#325 = CARTESIAN_POINT ( 'NONE',  ( -2.121784821874996840, 11.38437500061451679, 33.67503911421598417 ) ) ;
#326 = CARTESIAN_POINT ( 'NONE',  ( 21.26250000122903572, -4.330127018922190985, -2.500000000000001332 ) ) ;
#327 = CARTESIAN_POINT ( 'NONE',  ( 14.65312500061451573, -4.541064518000417216, -2.621784821875001281 ) ) ;
#328 = CYLINDRICAL_SURFACE ( 'NONE', #3060, 3.999999999999996447 ) ;
#329 = VERTEX_POINT ( 'NONE', #38418 ) ;
#330 = ORIENTED_EDGE ( 'NONE', *, *, #52495, .F. ) ;
#331 = CARTESIAN_POINT ( 'NONE',  ( 20.54999999999999716, 0.000000000000000000, 4.999999999999998224 ) ) ;
#332 = CARTESIAN_POINT ( 'NONE',  ( 3.482548389542082568, 3.599757532507414481, 32.03236939885417911 ) ) ;
#333 = CARTESIAN_POINT ( 'NONE',  ( 14.85000000122903252, -2.886751345948129988, 4.999999999999997335 ) ) ;
#334 = CARTESIAN_POINT ( 'NONE',  ( 19.52812500061451573, -4.541064518000419881, 2.621784821874995952 ) ) ;
#335 = CARTESIAN_POINT ( 'NONE',  ( 23.24062500061451786, -3.027376345333610441, -5.243569643749999898 ) ) ;
#336 = EDGE_CURVE ( 'NONE', #58790, #48104, #15871, .T. ) ;
#337 = CARTESIAN_POINT ( 'NONE',  ( 5.128125000614516260, -4.541064518000419881, 2.621784821874995952 ) ) ;
#338 =( BOUNDED_CURVE ( )  B_SPLINE_CURVE ( 2, ( #15519, #49887, #72412, #9995, #32529, #66507, #49526 ),
 .UNSPECIFIED., .F., .F. ) 
 B_SPLINE_CURVE_WITH_KNOTS ( ( 3, 2, 2, 3 ),
 ( 0.5083333333333334147, 0.5111111111111110716, 0.5138888888888888395, 0.5166666666666666075 ),
 .UNSPECIFIED. ) 
 CURVE ( )  GEOMETRIC_REPRESENTATION_ITEM ( )  RATIONAL_B_SPLINE_CURVE ( ( 0.9999999999999946709, 0.8660254037844440367, 1.000000000000000000, 0.8660254037844387076, 1.000000000000000000, 0.8660254037844440367, 0.9999999999999946709 ) ) 
 REPRESENTATION_ITEM ( '' )  );
#339 = AXIS2_PLACEMENT_3D ( 'NONE', #22340, #45247, #39713 ) ;
#340 = CARTESIAN_POINT ( 'NONE',  ( 29.06250000000000000, 2.886751345948126879, 4.999999999999999112 ) ) ;
#341 = CARTESIAN_POINT ( 'NONE',  ( -1.626862140677534273E-15, 15.03124999877096535, 34.00000000000000000 ) ) ;
#342 = CARTESIAN_POINT ( 'NONE',  ( 9.946875000614516793, 5.492252693125287522, 3.363034840372157021E-16 ) ) ;
#343 = CYLINDRICAL_SURFACE ( 'NONE', #34692, 4.000000000000000000 ) ;
#344 = CARTESIAN_POINT ( 'NONE',  ( 4.000000000000000000, 10.85000000122903430, -27.69059892324149530 ) ) ;
#345 = CARTESIAN_POINT ( 'NONE',  ( 4.243569643749999010, 17.87187500061451573, -32.45002607614398471 ) ) ;
#346 = CARTESIAN_POINT ( 'NONE',  ( 6.562500001229032875, 4.330127018922192761, -2.499999999999997780 ) ) ;
#347 = CARTESIAN_POINT ( 'NONE',  ( 8.737500000000002487, 5.773502691896255534, 3.535250795749688894E-16 ) ) ;
#348 = CARTESIAN_POINT ( 'NONE',  ( 3.787500001229033408, 6.123233995736764310E-16, -4.999999999999998224 ) ) ;
#349 = CARTESIAN_POINT ( 'NONE',  ( 11.74687500061451573, 6.054752690667223547, 3.707466751127219781E-16 ) ) ;
#350 = CARTESIAN_POINT ( 'NONE',  ( 4.057522967627288146, -2.921730200955767298, 4.057522967627288146 ) ) ;
#351 = CARTESIAN_POINT ( 'NONE',  ( 4.396875000614516971, -3.027376345333610441, -5.243569643749999898 ) ) ;
#352 = CARTESIAN_POINT ( 'NONE',  ( 12.90000000122903323, 5.773502691896255534, 3.535250795749688401E-16 ) ) ;
#353 = CARTESIAN_POINT ( 'NONE',  ( 4.000000000000000000, 19.40000000122903856, 32.30940107675849760 ) ) ;
#354 = CARTESIAN_POINT ( 'NONE',  ( 10.84687500061451892, 6.054752690667223547, 3.707466751127219781E-16 ) ) ;
#355 = CARTESIAN_POINT ( 'NONE',  ( 14.48437500061451821, 4.541064518000418104, 2.621784821874999949 ) ) ;
#356 = CARTESIAN_POINT ( 'NONE',  ( 3.609349942001692124, -3.970247583483341280, -3.123329466779292130 ) ) ;
#357 = CARTESIAN_POINT ( 'NONE',  ( 2.121784821874999061, 16.50312500061459176, 26.32496088578401583 ) ) ;
#358 = CARTESIAN_POINT ( 'NONE',  ( 21.15937500061451715, 4.541064518000418104, -2.621784821874998173 ) ) ;
#359 = CARTESIAN_POINT ( 'NONE',  ( 26.92500000122903359, 2.886751345948126879, 4.999999999999999112 ) ) ;
#360 = CARTESIAN_POINT ( 'NONE',  ( 18.38437500061451502, 5.492252693125287522, 3.363034840372157021E-16 ) ) ;
#361 = CARTESIAN_POINT ( 'NONE',  ( 22.52812500061451573, 4.541064518000418104, 2.621784821874999949 ) ) ;
#362 = CARTESIAN_POINT ( 'NONE',  ( 15.85312500061451857, 0.000000000000000000, 5.243569643749999010 ) ) ;
#363 = CARTESIAN_POINT ( 'NONE',  ( 26.67187500061451289, -4.119189519843968306, 2.378215178124996054 ) ) ;
#364 = CARTESIAN_POINT ( 'NONE',  ( 11.55937500061451928, -4.541064518000417216, -2.621784821875001281 ) ) ;
#365 = CARTESIAN_POINT ( 'NONE',  ( 29.73750000000000071, -2.886751345948125991, -5.000000000000000000 ) ) ;
#366 = CARTESIAN_POINT ( 'NONE',  ( 24.75000000122902932, -2.886751345948129988, 4.999999999999997335 ) ) ;
#367 = CARTESIAN_POINT ( 'NONE',  ( 4.659375000614518925, 0.000000000000000000, 5.243569643749999010 ) ) ;
#368 = CARTESIAN_POINT ( 'NONE',  ( 14.93437500061451750, 4.541064518000418104, 2.621784821874999949 ) ) ;
#369 = CARTESIAN_POINT ( 'NONE',  ( 29.70937500061451431, 4.541064518000418104, -2.621784821874998173 ) ) ;
#370 = CARTESIAN_POINT ( 'NONE',  ( 3.070561448845197550, -4.159287105319667610, 2.795903410320249360 ) ) ;
#371 = FACE_OUTER_BOUND ( 'NONE', #14066, .T. ) ;
#372 = CARTESIAN_POINT ( 'NONE',  ( 22.84687500061451715, -3.027376345333610441, -5.243569643749999898 ) ) ;
#373 = CARTESIAN_POINT ( 'NONE',  ( 14.82187500061451679, 3.027376345333613106, -5.243569643749998122 ) ) ;
#374 = CARTESIAN_POINT ( 'NONE',  ( -1.878215178125001827, 14.85312499938548214, 33.25316411605952283 ) ) ;
#375 = CARTESIAN_POINT ( 'NONE',  ( 25.76249999999999929, 2.886751345948129099, -4.999999999999998224 ) ) ;
#376 = CARTESIAN_POINT ( 'NONE',  ( 4.350000001229033408, 5.773502691896255534, 3.535250795749688894E-16 ) ) ;
#377 = CARTESIAN_POINT ( 'NONE',  ( 7.696875000614517681, 0.000000000000000000, 4.756430356249998326 ) ) ;
#378 = CARTESIAN_POINT ( 'NONE',  ( 16.26562500061451289, 3.027376345333611329, 5.243569643749999010 ) ) ;
#379 = CARTESIAN_POINT ( 'NONE',  ( 7.687500000000000000, -2.886751345948125991, -5.000000000000000000 ) ) ;
#380 = EDGE_CURVE ( 'NONE', #38892, #55608, #31618, .T. ) ;
#381 = CARTESIAN_POINT ( 'NONE',  ( 13.65000000122903323, -2.886751345948193048, -4.999999999999883649 ) ) ;
#382 = CARTESIAN_POINT ( 'NONE',  ( 16.80000000000000071, 4.330127018922192761, -2.499999999999997780 ) ) ;
#383 = CARTESIAN_POINT ( 'NONE',  ( -4.243569643749999898, 13.95312500061451821, 30.00000000000000000 ) ) ;
#384 = CARTESIAN_POINT ( 'NONE',  ( 24.84375000122903288, -2.886751345948153968, -4.999999999999952038 ) ) ;
#385 = CARTESIAN_POINT ( 'NONE',  ( 20.88750000122903572, 6.123233995736764310E-16, -4.999999999999998224 ) ) ;
#386 = CARTESIAN_POINT ( 'NONE',  ( 11.38125000122903252, 6.123233995736764310E-16, -4.999999999999998224 ) ) ;
#387 = CARTESIAN_POINT ( 'NONE',  ( 26.18437500061451573, 4.541064518000418104, 2.621784821874999949 ) ) ;
#388 = ORIENTED_EDGE ( 'NONE', *, *, #31467, .F. ) ;
#389 = CARTESIAN_POINT ( 'NONE',  ( 21.36562500061451431, -6.054752690667223547, -1.112240025338166033E-15 ) ) ;
#390 = CARTESIAN_POINT ( 'NONE',  ( 21.72187500061451715, 3.027376345333611329, 5.243569643749999010 ) ) ;
#391 = CARTESIAN_POINT ( 'NONE',  ( 6.787500000000001421, -2.886751345948125991, -5.000000000000000000 ) ) ;
#392 = CARTESIAN_POINT ( 'NONE',  ( 8.915625000614515017, 3.027376345333613106, -5.243569643749998122 ) ) ;
#393 = CARTESIAN_POINT ( 'NONE',  ( 23.46562500061451573, 3.027376345333611329, 5.243569643749999010 ) ) ;
#394 = CARTESIAN_POINT ( 'NONE',  ( 12.72187500061451537, 3.027376345333611329, 5.243569643749999010 ) ) ;
#395 = CARTESIAN_POINT ( 'NONE',  ( 16.80937500061451573, 0.000000000000000000, 5.243569643749999010 ) ) ;
#396 = CARTESIAN_POINT ( 'NONE',  ( 19.20000000000000284, 0.000000000000000000, 4.999999999999998224 ) ) ;
#397 = CARTESIAN_POINT ( 'NONE',  ( 4.243569643749999898, 17.74062500061451786, 32.45002607614398471 ) ) ;
#398 = CARTESIAN_POINT ( 'NONE',  ( 21.60000000122903430, -2.886751345948129988, 4.999999999999997335 ) ) ;
#399 = CARTESIAN_POINT ( 'NONE',  ( 15.08437500061451786, -4.119189519843968306, 2.378215178124996054 ) ) ;
#400 = CARTESIAN_POINT ( 'NONE',  ( 11.16562500061451679, 3.027376345333612662, -5.243569643749998122 ) ) ;
#401 = CARTESIAN_POINT ( 'NONE',  ( 4.959375000614516971, 4.541064518000418104, -2.621784821874998173 ) ) ;
#402 = CARTESIAN_POINT ( 'NONE',  ( 4.059375000614519280, 4.541064518000418104, -2.621784821874998173 ) ) ;
#403 = VERTEX_POINT ( 'NONE', #43241 ) ;
#404 = CARTESIAN_POINT ( 'NONE',  ( 24.68437500061451573, 6.421520780324663323E-16, -5.243569643749999010 ) ) ;
#405 = CARTESIAN_POINT ( 'NONE',  ( 16.15312500061451573, 4.541064518000418104, -2.621784821874998173 ) ) ;
#406 = CARTESIAN_POINT ( 'NONE',  ( 27.26250000122903216, 4.330127018922192761, -2.499999999999997780 ) ) ;
#407 = CARTESIAN_POINT ( 'NONE',  ( 28.60312500061451502, -4.541064518000417216, -2.621784821875001281 ) ) ;
#408 = CARTESIAN_POINT ( 'NONE',  ( 21.98437500061451644, 6.421520780324663323E-16, -5.243569643749999010 ) ) ;
#409 = CARTESIAN_POINT ( 'NONE',  ( 16.22812500061451857, 4.541064518000418104, 2.621784821874999949 ) ) ;
#410 = CARTESIAN_POINT ( 'NONE',  ( 4.243569643749999898, 19.63437500061451857, 30.00000000000000000 ) ) ;
#411 = CARTESIAN_POINT ( 'NONE',  ( 22.94062500061451715, 6.054752690667223547, 3.707466751127219781E-16 ) ) ;
#412 = CARTESIAN_POINT ( 'NONE',  ( 3.825000001229032609, 2.886751345948129099, -4.999999999999998224 ) ) ;
#413 = ORIENTED_EDGE ( 'NONE', *, *, #34178, .T. ) ;
#414 = CARTESIAN_POINT ( 'NONE',  ( 28.57499999999999929, 4.330127018922191873, 2.499999999999999556 ) ) ;
#415 = CARTESIAN_POINT ( 'NONE',  ( -2.000000000000000000, 13.17500000000000071, -33.46410161513775705 ) ) ;
#416 = CARTESIAN_POINT ( 'NONE',  ( 2.655984681222220721E-16, 16.46562499938548285, 25.66244784525396483 ) ) ;
#417 = CARTESIAN_POINT ( 'NONE',  ( 29.09062500061451573, -3.027376345333610441, -5.243569643749999898 ) ) ;
#418 = CARTESIAN_POINT ( 'NONE',  ( 9.253125000614517148, -4.541064518000417216, -2.621784821875001281 ) ) ;
#419 = CARTESIAN_POINT ( 'NONE',  ( 21.22500000122903074, -5.773502691896255534, -1.060575238724906372E-15 ) ) ;
#420 = EDGE_CURVE ( 'NONE', #14890, #16300, #13688, .T. ) ;
#421 = CARTESIAN_POINT ( 'NONE',  ( 12.68437500061451573, 4.541064518000418104, 2.621784821874999949 ) ) ;
#422 = CARTESIAN_POINT ( 'NONE',  ( 28.07812500061451289, -4.541064518000419881, 2.621784821874995952 ) ) ;
#423 = CARTESIAN_POINT ( 'NONE',  ( 27.29999999999999716, 0.000000000000000000, 4.999999999999998224 ) ) ;
#424 = CARTESIAN_POINT ( 'NONE',  ( 4.000000000000000000, 17.60000000122903785, -27.69059892324149530 ) ) ;
#425 = CARTESIAN_POINT ( 'NONE',  ( -1.487416814333745711E-14, 15.72500000122903430, -26.00000000000000000 ) ) ;
#426 = CARTESIAN_POINT ( 'NONE',  ( 12.10312500061451857, 4.541064518000418104, -2.621784821874998173 ) ) ;
#427 = VERTEX_POINT ( 'NONE', #4808 ) ;
#428 = CARTESIAN_POINT ( 'NONE',  ( 11.16562500061451679, 3.027376345333613106, -5.243569643749998122 ) ) ;
#429 = CARTESIAN_POINT ( 'NONE',  ( 6.253125000614517148, 4.541064518000418104, -2.621784821874998173 ) ) ;
#430 = CARTESIAN_POINT ( 'NONE',  ( 17.37187500061451573, -5.492252693125287522, -1.008910452111647106E-15 ) ) ;
#431 = EDGE_CURVE ( 'NONE', #55385, #17600, #60203, .T. ) ;
#432 = CARTESIAN_POINT ( 'NONE',  ( 14.53125000122903288, 6.123233995736764310E-16, -4.999999999999998224 ) ) ;
#433 = CARTESIAN_POINT ( 'NONE',  ( 15.90000000000000036, 4.330127018922192761, -2.499999999999997780 ) ) ;
#434 = CARTESIAN_POINT ( 'NONE',  ( 16.54687500061451644, -3.027376345333610441, -5.243569643749999898 ) ) ;
#435 = CARTESIAN_POINT ( 'NONE',  ( 10.98750000122903536, 6.123233995736764310E-16, -4.999999999999998224 ) ) ;
#436 = CARTESIAN_POINT ( 'NONE',  ( 18.79687500061451644, -3.027376345333610441, -5.243569643749999898 ) ) ;
#437 = CARTESIAN_POINT ( 'NONE',  ( 18.67500000000000071, 4.330127018922191873, 2.499999999999999556 ) ) ;
#438 = CARTESIAN_POINT ( 'NONE',  ( 19.73437500061451644, 6.421520780324663323E-16, -5.243569643749999010 ) ) ;
#439 = CARTESIAN_POINT ( 'NONE',  ( -2.121784821874996840, 14.92812500061451608, -26.32496088578401583 ) ) ;
#440 = CARTESIAN_POINT ( 'NONE',  ( 1.071796769724497445, 16.71740381056766367, 26.00000000000000355 ) ) ;
#441 = CARTESIAN_POINT ( 'NONE',  ( 26.14687500061451431, 0.000000000000000000, 4.756430356249998326 ) ) ;
#442 = CARTESIAN_POINT ( 'NONE',  ( 18.39375000122902648, -2.886751345948074920, 5.000000000000092371 ) ) ;
#443 = CARTESIAN_POINT ( 'NONE',  ( 27.66562500061451146, -6.054752690667223547, -1.112240025338166033E-15 ) ) ;
#444 = SURFACE_STYLE_FILL_AREA ( #52132 ) ;
#445 = CARTESIAN_POINT ( 'NONE',  ( 29.14687500061451075, -3.027376345333610441, -5.243569643749999898 ) ) ;
#446 = EDGE_CURVE ( 'NONE', #17600, #24863, #53958, .T. ) ;
#447 = CARTESIAN_POINT ( 'NONE',  ( 25.01249999999999929, 2.886751345948126879, 4.999999999999999112 ) ) ;
#448 = CARTESIAN_POINT ( 'NONE',  ( 9.478125000614515017, 4.541064518000418104, 2.621784821874999949 ) ) ;
#449 = CARTESIAN_POINT ( 'NONE',  ( 25.02187500061451431, 5.824947211148865298E-16, -4.756430356249998326 ) ) ;
#450 = CARTESIAN_POINT ( 'NONE',  ( 19.50937500061451857, 0.000000000000000000, 5.243569643749999010 ) ) ;
#451 = CARTESIAN_POINT ( 'NONE',  ( 11.10937500061451644, 2.746126346562645981, -4.756430356249997438 ) ) ;
#452 = CARTESIAN_POINT ( 'NONE',  ( 6.440625000614517148, -3.027376345333614438, 5.243569643749998122 ) ) ;
#453 = CARTESIAN_POINT ( 'NONE',  ( 11.07187500061451679, -6.054752690667223547, -1.112240025338166033E-15 ) ) ;
#454 = ORIENTED_EDGE ( 'NONE', *, *, #66600, .F. ) ;
#455 = CARTESIAN_POINT ( 'NONE',  ( 22.54687500061451999, 6.054752690667223547, 3.707466751127219781E-16 ) ) ;
#456 = CARTESIAN_POINT ( 'NONE',  ( 45.00000000000000000, 6.123233995736764310E-16, -4.999999999999998224 ) ) ;
#457 = CARTESIAN_POINT ( 'NONE',  ( 17.00625000122903074, 0.000000000000000000, 4.999999999999998224 ) ) ;
#458 = EDGE_CURVE ( 'NONE', #51815, #43576, #43970, .T. ) ;
#459 = CARTESIAN_POINT ( 'NONE',  ( 3.862500000000001155, 2.886751345948126879, 4.999999999999999112 ) ) ;
#460 = CARTESIAN_POINT ( 'NONE',  ( 14.73750000122903359, 4.330127018922191873, 2.499999999999999556 ) ) ;
#461 = CYLINDRICAL_SURFACE ( 'NONE', #51393, 4.999999999999998224 ) ;
#462 = LINE ( 'NONE', #60676, #9126 ) ;
#463 = ORIENTED_EDGE ( 'NONE', *, *, #9642, .F. ) ;
#464 = CARTESIAN_POINT ( 'NONE',  ( 13.23750000000000071, 5.773502691896255534, 3.535250795749688894E-16 ) ) ;
#465 = CARTESIAN_POINT ( 'NONE',  ( 13.69687500061451679, -4.119189519843965641, -2.378215178125001383 ) ) ;
#466 = CARTESIAN_POINT ( 'NONE',  ( 25.15312500061451217, 4.541064518000418104, -2.621784821874998173 ) ) ;
#467 = CARTESIAN_POINT ( 'NONE',  ( 14.62500000000000000, 4.330127018922191873, 2.499999999999999556 ) ) ;
#468 = CARTESIAN_POINT ( 'NONE',  ( 11.25000000122903288, -2.886751345948129988, 4.999999999999997335 ) ) ;
#469 = CARTESIAN_POINT ( 'NONE',  ( 10.00312500061451715, 0.000000000000000000, 5.243569643749999010 ) ) ;
#470 = CARTESIAN_POINT ( 'NONE',  ( 9.825000000000001066, -4.330127018922194537, 2.499999999999995559 ) ) ;
#471 = CARTESIAN_POINT ( 'NONE',  ( 4.898734551532200499, 1.001199177798645534, 4.898734551532191617 ) ) ;
#472 = CARTESIAN_POINT ( 'NONE',  ( 26.81250000122903288, 4.330127018922192761, -2.499999999999997780 ) ) ;
#473 = CARTESIAN_POINT ( 'NONE',  ( 1.878215178125000495, 18.11562499938548498, 26.74683588394047007 ) ) ;
#474 = CARTESIAN_POINT ( 'NONE',  ( 8.362500000000002487, 2.886751345948126879, 4.999999999999999112 ) ) ;
#475 = CARTESIAN_POINT ( 'NONE',  ( 18.86249999999999716, -5.773502691896255534, -1.060575238724906372E-15 ) ) ;
#476 = ORIENTED_EDGE ( 'NONE', *, *, #37237, .F. ) ;
#477 = CARTESIAN_POINT ( 'NONE',  ( 22.90312500061451573, 4.541064518000418104, -2.621784821874998173 ) ) ;
#478 = CARTESIAN_POINT ( 'NONE',  ( 28.37812500061451715, 4.541064518000418104, 2.621784821874999949 ) ) ;
#479 = CARTESIAN_POINT ( 'NONE',  ( 4.898587196589411843E-16, 20.00000000000000000, -26.00000000000000000 ) ) ;
#480 = CARTESIAN_POINT ( 'NONE',  ( 19.05937500061451928, 0.000000000000000000, 5.243569643749999010 ) ) ;
#481 = CARTESIAN_POINT ( 'NONE',  ( 17.65312500061451573, 0.000000000000000000, 5.243569643749999010 ) ) ;
#482 = CARTESIAN_POINT ( 'NONE',  ( 4.243569643749999898, 11.47812500061459318, -30.00000000000000000 ) ) ;
#483 = CARTESIAN_POINT ( 'NONE',  ( 6.328125000614515550, 4.541064518000418104, 2.621784821874999949 ) ) ;
#484 = CARTESIAN_POINT ( 'NONE',  ( 29.21250000122903145, 0.000000000000000000, 4.999999999999998224 ) ) ;
#485 = CARTESIAN_POINT ( 'NONE',  ( 21.53437500061451715, 5.824947211148865298E-16, -4.756430356249998326 ) ) ;
#486 = CARTESIAN_POINT ( 'NONE',  ( 18.17812500061451786, -4.541064518000419881, 2.621784821874995952 ) ) ;
#487 = CARTESIAN_POINT ( 'NONE',  ( 1.999999999999998668, 11.41250000122903430, -33.46410161513775705 ) ) ;
#488 = CARTESIAN_POINT ( 'NONE',  ( 3.375000001229033320, 2.886751345948129099, -4.999999999999998224 ) ) ;
#489 =( BOUNDED_CURVE ( )  B_SPLINE_CURVE ( 2, ( #20921, #14646, #9118, #48647, #21286, #33107, #71172 ),
 .UNSPECIFIED., .F., .F. ) 
 B_SPLINE_CURVE_WITH_KNOTS ( ( 3, 2, 2, 3 ),
 ( 0.3500000000000000888, 0.3533333333333333881, 0.3566666666666667429, 0.3599999999999999867 ),
 .UNSPECIFIED. ) 
 CURVE ( )  GEOMETRIC_REPRESENTATION_ITEM ( )  RATIONAL_B_SPLINE_CURVE ( ( 0.9999999999999955591, 0.8660254037844431485, 1.000000000000000000, 0.8660254037844387076, 1.000000000000000000, 0.8660254037844387076, 1.000000000000000000 ) ) 
 REPRESENTATION_ITEM ( '' )  );
#490 = CARTESIAN_POINT ( 'NONE',  ( 13.13437500061451857, 4.541064518000418104, 2.621784821874999949 ) ) ;
#491 = CARTESIAN_POINT ( 'NONE',  ( 12.68437500061451573, 4.541064518000418104, 2.621784821874999949 ) ) ;
#492 = CARTESIAN_POINT ( 'NONE',  ( 20.67187500061451289, 3.027376345333613106, -5.243569643749998122 ) ) ;
#493 = VERTEX_POINT ( 'NONE', #59846 ) ;
#494 = CARTESIAN_POINT ( 'NONE',  ( -0.8062380997993553455, 9.975217491784283297, 24.04105076033751942 ) ) ;
#495 = CARTESIAN_POINT ( 'NONE',  ( 23.91562500061451502, 3.027376345333611329, 5.243569643749999010 ) ) ;
#496 = CARTESIAN_POINT ( 'NONE',  ( 18.00937500061451502, 4.541064518000418104, -2.621784821874998173 ) ) ;
#497 = CARTESIAN_POINT ( 'NONE',  ( 25.30312500061451431, 0.000000000000000000, 5.243569643749999010 ) ) ;
#498 = CARTESIAN_POINT ( 'NONE',  ( -4.000000000000000000, 17.16874999877096641, 30.00000000000000000 ) ) ;
#499 = CARTESIAN_POINT ( 'NONE',  ( -3.999999999999999112, 15.94999999999999929, 30.00000000000000000 ) ) ;
#500 = CARTESIAN_POINT ( 'NONE',  ( 3.871875000614519280, -6.054752690667223547, -1.112240025338166033E-15 ) ) ;
#501 = ITEM_DEFINED_TRANSFORMATION ( 'NONE', 'NONE', #6134,  #23765 ) ;
#502 = CARTESIAN_POINT ( 'NONE',  ( 10.95000000122903394, -2.886751345948125991, -5.000000000000000000 ) ) ;
#503 = CARTESIAN_POINT ( 'NONE',  ( 7.612500001229035362, 0.000000000000000000, 4.999999999999998224 ) ) ;
#504 = CARTESIAN_POINT ( 'NONE',  ( 10.20000000000000107, 0.000000000000000000, 4.999999999999998224 ) ) ;
#505 = CARTESIAN_POINT ( 'NONE',  ( 27.56250000122902932, -4.330127018922190985, -2.500000000000001332 ) ) ;
#506 = CARTESIAN_POINT ( 'NONE',  ( 4.000000000000000000, 17.88124999877096855, 27.69059892324149530 ) ) ;
#507 = CARTESIAN_POINT ( 'NONE',  ( 16.66875000122903216, -5.773502691896255534, -1.060575238724906372E-15 ) ) ;
#508 = CARTESIAN_POINT ( 'NONE',  ( 9.009375000614518569, 4.541064518000418104, -2.621784821874998173 ) ) ;
#509 = CARTESIAN_POINT ( 'NONE',  ( 29.67656250092177217, 0.000000000000000000, 4.878215178124998275 ) ) ;
#510 = CARTESIAN_POINT ( 'NONE',  ( 16.37812500061451715, -4.541064518000419881, 2.621784821874995952 ) ) ;
#511 = CARTESIAN_POINT ( 'NONE',  ( 12.57187500061451857, 3.027376345333613106, -5.243569643749998122 ) ) ;
#512 = CARTESIAN_POINT ( 'NONE',  ( 5.765625000614519102, 3.027376345333613106, -5.243569643749998122 ) ) ;
#513 = CARTESIAN_POINT ( 'NONE',  ( 20.25937500061451857, 4.541064518000418104, -2.621784821874998173 ) ) ;
#514 = CARTESIAN_POINT ( 'NONE',  ( 10.65937500061451715, -4.541064518000417216, -2.621784821875001281 ) ) ;
#515 = CARTESIAN_POINT ( 'NONE',  ( 2.990625000614519191, -3.027376345333610441, -5.243569643749999898 ) ) ;
#516 = CARTESIAN_POINT ( 'NONE',  ( 7.320879633048903241E-15, 17.63749999999999218, 26.00000000000000355 ) ) ;
#517 = CARTESIAN_POINT ( 'NONE',  ( 6.300000001229033586, -2.886751345948129988, 4.999999999999997335 ) ) ;
#518 = CARTESIAN_POINT ( 'NONE',  ( 21.14062500061451289, 6.054752690667223547, 3.707466751127219781E-16 ) ) ;
#519 = EDGE_LOOP ( 'NONE', ( #17956, #34557, #55612, #8707 ) ) ;
#520 = CARTESIAN_POINT ( 'NONE',  ( 5.475000001229035185, -5.773502691896255534, -1.060575238724906372E-15 ) ) ;
#521 = CARTESIAN_POINT ( 'NONE',  ( 18.32812500061451644, 6.421520780324663323E-16, -5.243569643749999010 ) ) ;
#522 = CARTESIAN_POINT ( 'NONE',  ( 13.64062500061451644, -3.027376345333614438, 5.243569643749998122 ) ) ;
#523 = CARTESIAN_POINT ( 'NONE',  ( 25.32187500061451857, 2.746126346562643317, 4.756430356249998326 ) ) ;
#524 = CARTESIAN_POINT ( 'NONE',  ( 13.01249999999999929, -5.773502691896255534, -1.060575238724906372E-15 ) ) ;
#525 = CARTESIAN_POINT ( 'NONE',  ( 9.750000001229032875, 5.773502691896255534, 3.535250795749688894E-16 ) ) ;
#526 = CARTESIAN_POINT ( 'NONE',  ( 6.478125000614516793, -4.541064518000419881, 2.621784821874995952 ) ) ;
#527 = CARTESIAN_POINT ( 'NONE',  ( 19.61250000122903359, 4.330127018922192761, -2.499999999999997780 ) ) ;
#528 = CARTESIAN_POINT ( 'NONE',  ( 26.17500000000000071, 6.123233995736764310E-16, -4.999999999999998224 ) ) ;
#529 = CARTESIAN_POINT ( 'NONE',  ( -2.121784821874996840, 11.83437500061451786, -26.32496088578401583 ) ) ;
#530 = CARTESIAN_POINT ( 'NONE',  ( 4.955651476953736534, 0.6855146069033769551, 5.046959488524436210 ) ) ;
#531 = EDGE_CURVE ( 'NONE', #11388, #40707, #27615, .T. ) ;
#532 = DIRECTION ( 'NONE',  ( 0.000000000000000000, 0.000000000000000000, 1.000000000000000000 ) ) ;
#533 =( BOUNDED_CURVE ( )  B_SPLINE_CURVE ( 2, ( #30429, #71415, #70675, #37054, #15610, #8992, #71046, #4191, #26346 ),
 .UNSPECIFIED., .F., .F. ) 
 B_SPLINE_CURVE_WITH_KNOTS ( ( 3, 2, 2, 2, 3 ),
 ( 0.1630434782608695676, 0.1666666666666666574, 0.1739130434782608647, 0.1811594202898550721, 0.1847826086956521896 ),
 .UNSPECIFIED. ) 
 CURVE ( )  GEOMETRIC_REPRESENTATION_ITEM ( )  RATIONAL_B_SPLINE_CURVE ( ( 0.9330127018922194093, 0.9330127018922196314, 1.000000000000000000, 0.8660254037844387076, 1.000000000000000000, 0.8660254037844387076, 1.000000000000000000, 0.9330127018922190762, 0.9330127018922194093 ) ) 
 REPRESENTATION_ITEM ( '' )  );
#534 = CARTESIAN_POINT ( 'NONE',  ( 2.000000000000000444, 14.82500000000000107, 26.53589838486224650 ) ) ;
#535 = CARTESIAN_POINT ( 'NONE',  ( 21.19687500061451502, 6.054752690667223547, 3.707466751127219781E-16 ) ) ;
#536 = CARTESIAN_POINT ( 'NONE',  ( -1.487416814333745711E-14, 16.62500000122903288, 34.00000000000000000 ) ) ;
#537 = CARTESIAN_POINT ( 'NONE',  ( 15.70312500061451644, 4.541064518000418104, -2.621784821874998173 ) ) ;
#538 = CARTESIAN_POINT ( 'NONE',  ( 9.431250001229033231, -4.330127018922194537, 2.499999999999995559 ) ) ;
#539 = CARTESIAN_POINT ( 'NONE',  ( 23.02499999999999858, 6.123233995736764310E-16, -4.999999999999998224 ) ) ;
#540 = CARTESIAN_POINT ( 'NONE',  ( 28.50937500061451502, 0.000000000000000000, 5.243569643749999010 ) ) ;
#541 = CARTESIAN_POINT ( 'NONE',  ( 26.59687500061451360, 6.054752690667223547, 3.707466751127219781E-16 ) ) ;
#542 = CARTESIAN_POINT ( 'NONE',  ( 18.87187500061451573, 4.119189519843966529, 2.378215178124999607 ) ) ;
#543 = VECTOR ( 'NONE', #40593, 1000.000000000000000 ) ;
#544 = CARTESIAN_POINT ( 'NONE',  ( 11.50312500061451892, -4.541064518000417216, -2.621784821875001281 ) ) ;
#545 = CARTESIAN_POINT ( 'NONE',  ( 10.95937500061451964, 0.000000000000000000, 5.243569643749999010 ) ) ;
#546 = EDGE_LOOP ( 'NONE', ( #30188, #59828, #46939, #45480 ) ) ;
#547 = CARTESIAN_POINT ( 'NONE',  ( -1.071796769724488563, 14.24240381056766758, -26.00000000000000000 ) ) ;
#548 = CARTESIAN_POINT ( 'NONE',  ( 20.50312500061451715, -4.541064518000417216, -2.621784821875001281 ) ) ;
#549 = DIRECTION ( 'NONE',  ( 0.000000000000000000, 1.000000000000000000, -6.195440985631455317E-17 ) ) ;
#550 = CARTESIAN_POINT ( 'NONE',  ( 20.96250000000000213, 2.886751345948161074, 4.999999999999941380 ) ) ;
#551 = ADVANCED_FACE ( 'NONE', ( #32513 ), #31786, .F. ) ;
#552 = CARTESIAN_POINT ( 'NONE',  ( 9.074999999999999289, 6.123233995736764310E-16, -4.999999999999998224 ) ) ;
#553 = CARTESIAN_POINT ( 'NONE',  ( 22.20000000122903216, -2.886751345948125991, -5.000000000000000000 ) ) ;
#554 = CARTESIAN_POINT ( 'NONE',  ( 16.04062500061451857, -3.027376345333610441, -5.243569643749999898 ) ) ;
#555 = CARTESIAN_POINT ( 'NONE',  ( 13.13437500061451679, -2.746126346562646425, 4.756430356249996549 ) ) ;
#556 = ORIENTED_EDGE ( 'NONE', *, *, #3876, .T. ) ;
#557 = CARTESIAN_POINT ( 'NONE',  ( 19.57500000000000284, 4.330127018922191873, 2.499999999999999556 ) ) ;
#558 = CARTESIAN_POINT ( 'NONE',  ( 22.19999999999999574, 4.330127018922192761, -2.499999999999997780 ) ) ;
#559 = CARTESIAN_POINT ( 'NONE',  ( 21.53437500061451715, 6.421520780324663323E-16, -5.243569643749999010 ) ) ;
#560 = CARTESIAN_POINT ( 'NONE',  ( 26.16562500061451502, 3.027376345333611329, 5.243569643749999010 ) ) ;
#561 = EDGE_CURVE ( 'NONE', #45352, #72689, #39182, .T. ) ;
#562 =( BOUNDED_CURVE ( )  B_SPLINE_CURVE ( 2, ( #23170, #34989, #67892, #57518, #62340, #11736, #40181 ),
 .UNSPECIFIED., .F., .F. ) 
 B_SPLINE_CURVE_WITH_KNOTS ( ( 3, 2, 2, 3 ),
 ( 0.1750000000000000167, 0.1777777777777778123, 0.1805555555555555525, 0.1833333333333333204 ),
 .UNSPECIFIED. ) 
 CURVE ( )  GEOMETRIC_REPRESENTATION_ITEM ( )  RATIONAL_B_SPLINE_CURVE ( ( 0.9999999999999986677, 0.8660254037844400399, 1.000000000000000000, 0.8660254037844387076, 1.000000000000000000, 0.8660254037844387076, 1.000000000000000000 ) ) 
 REPRESENTATION_ITEM ( '' )  );
#564 = ORIENTED_EDGE ( 'NONE', *, *, #40344, .T. ) ;
#563 = VECTOR ( 'NONE', #40809, 1000.000000000000000 ) ;
#565 = CARTESIAN_POINT ( 'NONE',  ( 27.97500000122903074, -5.773502691896255534, -1.060575238724906372E-15 ) ) ;
#566 = CARTESIAN_POINT ( 'NONE',  ( 7.340625000614518392, -3.027376345333614438, 5.243569643749998122 ) ) ;
#567 = CARTESIAN_POINT ( 'NONE',  ( 1.071796769724489895, 12.21740381056766900, 26.00000000000000355 ) ) ;
#568 = CARTESIAN_POINT ( 'NONE',  ( 14.73749999999999893, -2.886751345948129988, 4.999999999999997335 ) ) ;
#569 = CARTESIAN_POINT ( 'NONE',  ( -2.121784821874999949, 18.37812500061451715, 26.32496088578401938 ) ) ;
#570 = CARTESIAN_POINT ( 'NONE',  ( 28.34062500061451928, 6.054752690667223547, 3.707466751127219781E-16 ) ) ;
#571 = VECTOR ( 'NONE', #21775, 1000.000000000000000 ) ;
#572 = CARTESIAN_POINT ( 'NONE',  ( 27.08437500061451786, 4.541064518000418104, 2.621784821874999949 ) ) ;
#573 = EDGE_LOOP ( 'NONE', ( #31473, #72505, #31464, #35325 ) ) ;
#574 = CARTESIAN_POINT ( 'NONE',  ( 24.77812500061451217, 4.541064518000418104, 2.621784821874999949 ) ) ;
#575 = CARTESIAN_POINT ( 'NONE',  ( 25.17187500061451644, 3.027376345333613106, -5.243569643749998122 ) ) ;
#576 = CARTESIAN_POINT ( 'NONE',  ( -4.243569643749999898, 19.31562500061459176, -32.45002607614398471 ) ) ;
#577 = CARTESIAN_POINT ( 'NONE',  ( 11.47499999999999964, 4.330127018922191873, 2.499999999999999556 ) ) ;
#578 = CARTESIAN_POINT ( 'NONE',  ( 9.740625000614516082, -3.027376345333610441, -5.243569643749999898 ) ) ;
#579 = CARTESIAN_POINT ( 'NONE',  ( 28.88437500061451502, 4.119189519843966529, 2.378215178124999607 ) ) ;
#580 = CARTESIAN_POINT ( 'NONE',  ( 29.01562500061451644, -6.054752690667223547, -1.112240025338166033E-15 ) ) ;
#581 = CARTESIAN_POINT ( 'NONE',  ( 26.95312500061451644, 4.541064518000418104, -2.621784821874998173 ) ) ;
#582 = CARTESIAN_POINT ( 'NONE',  ( 7.320879633048903241E-15, 18.08749999999999858, 26.00000000000000355 ) ) ;
#583 = CARTESIAN_POINT ( 'NONE',  ( 11.67187500061451821, 2.746126346562645981, -4.756430356249997438 ) ) ;
#584 = CARTESIAN_POINT ( 'NONE',  ( 18.42187500061451644, 3.027376345333613106, -5.243569643749998122 ) ) ;
#585 = CARTESIAN_POINT ( 'NONE',  ( -4.243569643749999898, 13.52187500061451786, 27.54997392385601529 ) ) ;
#586 = CARTESIAN_POINT ( 'NONE',  ( 20.18437500061451573, 6.421520780324663323E-16, -5.243569643749999010 ) ) ;
#587 = CARTESIAN_POINT ( 'NONE',  ( 27.98437500061451289, 4.541064518000418104, 2.621784821874999949 ) ) ;
#588 = CARTESIAN_POINT ( 'NONE',  ( 2.121784821874999061, 17.00937500061451857, 26.32496088578401583 ) ) ;
#589 = CARTESIAN_POINT ( 'NONE',  ( 10.97812500061451679, -4.541064518000419881, 2.621784821874995952 ) ) ;
#590 = FACE_OUTER_BOUND ( 'NONE', #71381, .T. ) ;
#591 = CARTESIAN_POINT ( 'NONE',  ( 4.096875000614518925, 6.054752690667223547, 3.707466751127219781E-16 ) ) ;
#592 = CARTESIAN_POINT ( 'NONE',  ( -1.999999999999997113, 16.13750000122903216, -26.53589838486224295 ) ) ;
#593 =( BOUNDED_CURVE ( )  B_SPLINE_CURVE ( 2, ( #12661, #29655, #35196, #35914, #62904, #56997, #24104 ),
 .UNSPECIFIED., .F., .F. ) 
 B_SPLINE_CURVE_WITH_KNOTS ( ( 3, 2, 2, 3 ),
 ( 0.8600000000000002087, 0.8633333333333333970, 0.8666666666666668073, 0.8699999999999999956 ),
 .UNSPECIFIED. ) 
 CURVE ( )  GEOMETRIC_REPRESENTATION_ITEM ( )  RATIONAL_B_SPLINE_CURVE ( ( 0.9999999999999911182, 0.8660254037844475894, 1.000000000000000000, 0.8660254037844387076, 1.000000000000000000, 0.8660254037844387076, 1.000000000000000000 ) ) 
 REPRESENTATION_ITEM ( '' )  );
#594 = CARTESIAN_POINT ( 'NONE',  ( 7.828125000614517326, -4.541064518000419881, 2.621784821874995952 ) ) ;
#595 = CARTESIAN_POINT ( 'NONE',  ( 11.67187500061451821, 3.027376345333613106, -5.243569643749998122 ) ) ;
#596 = CARTESIAN_POINT ( 'NONE',  ( 19.35000000122903430, -2.886751345948129988, 4.999999999999997335 ) ) ;
#597 = CARTESIAN_POINT ( 'NONE',  ( 4.809375000614516615, -4.541064518000417216, -2.621784821875001281 ) ) ;
#598 = CARTESIAN_POINT ( 'NONE',  ( 7.903125000614515727, -4.541064518000417216, -2.621784821875001281 ) ) ;
#599 = CARTESIAN_POINT ( 'NONE',  ( 5.765625000614519102, 3.027376345333612662, -5.243569643749998122 ) ) ;
#600 = CARTESIAN_POINT ( 'NONE',  ( 22.36875000122903145, 2.886751345948126879, 4.999999999999999112 ) ) ;
#601 = CARTESIAN_POINT ( 'NONE',  ( 17.93437500061451928, 6.421520780324663323E-16, -5.243569643749999010 ) ) ;
#602 = ORIENTED_EDGE ( 'NONE', *, *, #7167, .F. ) ;
#603 = CARTESIAN_POINT ( 'NONE',  ( 24.36562500061451786, 3.027376345333611329, 5.243569643749999010 ) ) ;
#604 = CARTESIAN_POINT ( 'NONE',  ( 12.92812500061451786, 6.421520780324663323E-16, -5.243569643749999010 ) ) ;
#605 = CARTESIAN_POINT ( 'NONE',  ( 26.84999999999999787, 0.000000000000000000, 4.999999999999998224 ) ) ;
#606 = CARTESIAN_POINT ( 'NONE',  ( 11.76562500061451644, 3.027376345333611329, 5.243569643749999010 ) ) ;
#607 = CARTESIAN_POINT ( 'NONE',  ( 25.55625000122903501, 0.000000000000000000, 4.999999999999998224 ) ) ;
#608 = CARTESIAN_POINT ( 'NONE',  ( 11.73750000122903181, -4.330127018922194537, 2.499999999999995559 ) ) ;
#609 = CARTESIAN_POINT ( 'NONE',  ( 26.80312500061451431, -4.541064518000417216, -2.621784821875001281 ) ) ;
#610 = CARTESIAN_POINT ( 'NONE',  ( -3.000416591977282496E-16, 12.94062500061451537, -34.90005215228797653 ) ) ;
#611 = CARTESIAN_POINT ( 'NONE',  ( 14.88750000122903394, -4.330127018922194537, 2.499999999999995559 ) ) ;
#612 = CARTESIAN_POINT ( 'NONE',  ( 11.47499999999999964, 4.330127018922191873, 2.499999999999999556 ) ) ;
#613 = CARTESIAN_POINT ( 'NONE',  ( 19.56562500061451715, -6.054752690667223547, -1.112240025338166033E-15 ) ) ;
#614 = CARTESIAN_POINT ( 'NONE',  ( 7.921875000614517326, -6.054752690667223547, -1.112240025338166033E-15 ) ) ;
#615 = CARTESIAN_POINT ( 'NONE',  ( 6.900000001229035007, -2.886751345948125991, -5.000000000000000000 ) ) ;
#616 = CARTESIAN_POINT ( 'NONE',  ( 16.01250000122903216, 4.330127018922192761, -2.499999999999997780 ) ) ;
#617 = CIRCLE ( 'NONE', #41869, 14.99999999999999822 ) ;
#618 = CARTESIAN_POINT ( 'NONE',  ( 13.22812500061451502, -4.541064518000419881, 2.621784821874995952 ) ) ;
#619 = CARTESIAN_POINT ( 'NONE',  ( 16.71562500061451573, 3.027376345333611329, 5.243569643749999010 ) ) ;
#620 = AXIS2_PLACEMENT_3D ( 'NONE', #43170, #25435, #32078 ) ;
#621 = CARTESIAN_POINT ( 'NONE',  ( 26.55000000122902648, -2.886751345948129988, 4.999999999999997335 ) ) ;
#622 = CARTESIAN_POINT ( 'NONE',  ( 20.96250000000000213, 2.886751345948126879, 4.999999999999999112 ) ) ;
#623 = AXIS2_PLACEMENT_3D ( 'NONE', #29778, #52314, #7249 ) ;
#624 = CARTESIAN_POINT ( 'NONE',  ( 22.39687500061451075, -3.027376345333610441, -5.243569643749999898 ) ) ;
#625 = CARTESIAN_POINT ( 'NONE',  ( 4.000000000000000000, 13.85000000000000142, 30.00000000000000000 ) ) ;
#626 = CARTESIAN_POINT ( 'NONE',  ( 10.80000000122903536, -2.886751345948129988, 4.999999999999997335 ) ) ;
#627 = CARTESIAN_POINT ( 'NONE',  ( 8.746875000614515727, -3.027376345333614438, 5.243569643749998122 ) ) ;
#628 = CARTESIAN_POINT ( 'NONE',  ( 27.38437500061451857, 6.421520780324663323E-16, -5.243569643749999010 ) ) ;
#629 = CARTESIAN_POINT ( 'NONE',  ( 1.626862140677534470E-15, 13.23124999877096819, 34.00000000000000000 ) ) ;
#630 = CARTESIAN_POINT ( 'NONE',  ( 23.54062500061451146, -3.027376345333614438, 5.243569643749998122 ) ) ;
#631 = CARTESIAN_POINT ( 'NONE',  ( 3.756430356250000546, 15.94062499938548427, 27.83122392262697886 ) ) ;
#632 = CARTESIAN_POINT ( 'NONE',  ( 4.000000000000000000, 19.73749999999999716, -27.69059892324149885 ) ) ;
#633 = CARTESIAN_POINT ( 'NONE',  ( 8.334375000614516082, -4.541064518000419881, 2.621784821874995952 ) ) ;
#634 = CARTESIAN_POINT ( 'NONE',  ( 1.626862140677534273E-15, 12.46250000000000213, 34.00000000000000000 ) ) ;
#635 = CARTESIAN_POINT ( 'NONE',  ( 27.62812500061451360, -4.541064518000419881, 2.621784821874995952 ) ) ;
#636 = CARTESIAN_POINT ( 'NONE',  ( 6.759375000614516793, 4.541064518000418104, -2.621784821874998173 ) ) ;
#637 = CARTESIAN_POINT ( 'NONE',  ( 6.787500000000001421, -2.886751345948126435, -5.000000000000000000 ) ) ;
#638 = CARTESIAN_POINT ( 'NONE',  ( 25.77187500061451075, 3.027376345333611329, 5.243569643749999010 ) ) ;
#639 = CARTESIAN_POINT ( 'NONE',  ( 18.89999999999999858, -4.330127018922190985, -2.500000000000001332 ) ) ;
#640 = EDGE_LOOP ( 'NONE', ( #68001, #59297, #35506, #56728 ) ) ;
#641 = CARTESIAN_POINT ( 'NONE',  ( 27.67499999999999716, 4.330127018922191873, 2.499999999999999556 ) ) ;
#642 = CARTESIAN_POINT ( 'NONE',  ( 28.54687500061451644, -3.027376345333614438, 5.243569643749998122 ) ) ;
#643 = EDGE_CURVE ( 'NONE', #26767, #59300, #38760, .T. ) ;
#644 = ORIENTED_EDGE ( 'NONE', *, *, #29319, .T. ) ;
#645 = CARTESIAN_POINT ( 'NONE',  ( 14.46562500061451750, 3.027376345333611329, 5.243569643749999010 ) ) ;
#646 = CARTESIAN_POINT ( 'NONE',  ( 8.278125000614515727, -4.541064518000419881, 2.621784821874995952 ) ) ;
#647 = CARTESIAN_POINT ( 'NONE',  ( 18.12187500061451928, -4.119189519843968306, 2.378215178124996054 ) ) ;
#648 = CARTESIAN_POINT ( 'NONE',  ( 4.246875000614519280, -3.027376345333614438, 5.243569643749998122 ) ) ;
#649 = CARTESIAN_POINT ( 'NONE',  ( 18.15000000122903501, -2.886751345948125991, -5.000000000000000000 ) ) ;
#650 = CARTESIAN_POINT ( 'NONE',  ( 21.75000000000000000, 4.330127018922192761, -2.499999999999997780 ) ) ;
#651 = CARTESIAN_POINT ( 'NONE',  ( 29.21249999999999858, -5.773502691896255534, -1.060575238724906372E-15 ) ) ;
#652 = CARTESIAN_POINT ( 'NONE',  ( 5.821875000614519458, 3.027376345333613106, -5.243569643749998122 ) ) ;
#653 = CARTESIAN_POINT ( 'NONE',  ( 11.93437500061451573, -4.541064518000419881, 2.621784821874995952 ) ) ;
#654 = CARTESIAN_POINT ( 'NONE',  ( 22.17187500061451644, 3.027376345333611329, 5.243569643749999010 ) ) ;
#655 = CARTESIAN_POINT ( 'NONE',  ( -2.000000000000000000, 17.22500000000000142, -33.46410161513775705 ) ) ;
#656 = ORIENTED_EDGE ( 'NONE', *, *, #40314, .T. ) ;
#657 = CARTESIAN_POINT ( 'NONE',  ( 4.996875000614516615, 6.054752690667223547, 3.707466751127219781E-16 ) ) ;
#658 = CARTESIAN_POINT ( 'NONE',  ( 7.021875000614518747, -6.054752690667223547, -1.112240025338166033E-15 ) ) ;
#659 = CARTESIAN_POINT ( 'NONE',  ( 18.67500000000000071, 4.330127018922191873, 2.499999999999999556 ) ) ;
#660 = CARTESIAN_POINT ( 'NONE',  ( 16.90312500061451573, -4.541064518000417216, -2.621784821875001281 ) ) ;
#661 = CARTESIAN_POINT ( 'NONE',  ( -2.000000000000001776, 19.54999999999999716, 33.46410161513775705 ) ) ;
#662 = CARTESIAN_POINT ( 'NONE',  ( 22.12500000000000000, 6.123233995736764310E-16, -4.999999999999998224 ) ) ;
#663 = CARTESIAN_POINT ( 'NONE',  ( 20.85937500061451644, 0.000000000000000000, 4.756430356249998326 ) ) ;
#664 = CARTESIAN_POINT ( 'NONE',  ( 9.815625000614518925, 3.027376345333613106, -5.243569643749998122 ) ) ;
#665 = CARTESIAN_POINT ( 'NONE',  ( 27.15937500061451360, 0.000000000000000000, 5.243569643749999010 ) ) ;
#666 = CARTESIAN_POINT ( 'NONE',  ( 6.262500001229034829, 0.000000000000000000, 4.999999999999998224 ) ) ;
#667 = CARTESIAN_POINT ( 'NONE',  ( 25.62187500061451573, 3.027376345333613106, -5.243569643749998122 ) ) ;
#668 = CARTESIAN_POINT ( 'NONE',  ( 9.674999999999998934, 4.330127018922191873, 2.499999999999999556 ) ) ;
#669 = CARTESIAN_POINT ( 'NONE',  ( 2.000000000000001332, 13.51250000122903394, 33.46410161513774995 ) ) ;
#670 = CARTESIAN_POINT ( 'NONE',  ( 9.412500001229034297, 0.000000000000000000, 4.999999999999998224 ) ) ;
#671 = AXIS2_PLACEMENT_3D ( 'NONE', #60394, #71870, #49704 ) ;
#672 = CARTESIAN_POINT ( 'NONE',  ( 20.59687500061451360, -3.027376345333610441, -5.243569643749999898 ) ) ;
#673 = CARTESIAN_POINT ( 'NONE',  ( 11.33437500061451608, 4.541064518000418104, 2.621784821874999949 ) ) ;
#674 = CARTESIAN_POINT ( 'NONE',  ( -1.090676731616017747, 4.887066358488519668, -33.85805426562694720 ) ) ;
#675 = VERTEX_POINT ( 'NONE', #2077 ) ;
#676 = CARTESIAN_POINT ( 'NONE',  ( 15.96562500061451573, -6.054752690667223547, -1.112240025338166033E-15 ) ) ;
#677 = AXIS2_PLACEMENT_3D ( 'NONE', #72142, #59579, #42605 ) ;
#678 = CARTESIAN_POINT ( 'NONE',  ( 25.80000000122903714, -2.886751345948125991, -5.000000000000000000 ) ) ;
#679 = CARTESIAN_POINT ( 'NONE',  ( 12.49687500061451573, -3.027376345333610441, -5.243569643749999898 ) ) ;
#680 = CARTESIAN_POINT ( 'NONE',  ( 17.16562500061451502, 3.027376345333611329, 5.243569643749999010 ) ) ;
#681 = CYLINDRICAL_SURFACE ( 'NONE', #16177, 4.999999999999998224 ) ;
#682 = CARTESIAN_POINT ( 'NONE',  ( 27.00937500061451857, 4.541064518000418104, -2.621784821874998173 ) ) ;
#683 = CARTESIAN_POINT ( 'NONE',  ( -2.121784821874996840, 11.32812500061451644, 33.67503911421598417 ) ) ;
#684 = CARTESIAN_POINT ( 'NONE',  ( 12.22500000122903430, -5.773502691896255534, -1.060575238724906372E-15 ) ) ;
#685 = LINE ( 'NONE', #56105, #8000 ) ;
#686 = CARTESIAN_POINT ( 'NONE',  ( -3.000416591977282496E-16, 17.49687500061451573, -34.90005215228797653 ) ) ;
#687 = CARTESIAN_POINT ( 'NONE',  ( 17.33437500061451431, -4.541064518000419881, 2.621784821874995952 ) ) ;
#688 = CARTESIAN_POINT ( 'NONE',  ( 20.88750000122903572, 6.123233995736764310E-16, -4.999999999999998224 ) ) ;
#689 = CARTESIAN_POINT ( 'NONE',  ( 14.59687500061452070, -3.027376345333614438, 5.243569643749998122 ) ) ;
#690 = CARTESIAN_POINT ( 'NONE',  ( -4.243569643749999898, 19.76562500061451644, -32.45002607614398471 ) ) ;
#691 = CARTESIAN_POINT ( 'NONE',  ( 23.55000000122903359, -2.886751345948125991, -5.000000000000000000 ) ) ;
#692 = CARTESIAN_POINT ( 'NONE',  ( 15.02812500061451750, -4.541064518000419881, 2.621784821874995952 ) ) ;
#693 = DIRECTION ( 'NONE',  ( -0.000000000000000000, -1.000000000000000000, -0.000000000000000000 ) ) ;
#694 = ORIENTED_EDGE ( 'NONE', *, *, #60253, .T. ) ;
#695 = ORIENTED_EDGE ( 'NONE', *, *, #13854, .T. ) ;
#696 = CARTESIAN_POINT ( 'NONE',  ( 20.62499999999999645, -4.330127018922194537, 2.499999999999995559 ) ) ;
#697 = CARTESIAN_POINT ( 'NONE',  ( 1.071796769724491227, 18.38615380933863008, 26.00000000000000000 ) ) ;
#698 = CARTESIAN_POINT ( 'NONE',  ( 2.915625000614516793, -6.054752690667223547, -1.112240025338166033E-15 ) ) ;
#699 = CARTESIAN_POINT ( 'NONE',  ( 15.11250000122903359, 4.330127018922192761, -2.499999999999997780 ) ) ;
#700 = CARTESIAN_POINT ( 'NONE',  ( 21.21562500061451573, 3.027376345333611329, 5.243569643749999010 ) ) ;
#701 = CARTESIAN_POINT ( 'NONE',  ( 23.91562500061451502, 3.027376345333611329, 5.243569643749999010 ) ) ;
#702 = CARTESIAN_POINT ( 'NONE',  ( 29.36250000122903003, -4.330127018922190985, -2.500000000000001332 ) ) ;
#703 = EDGE_CURVE ( 'NONE', #27416, #27910, #5889, .T. ) ;
#704 = CARTESIAN_POINT ( 'NONE',  ( 28.80000000000000071, -4.330127018922190985, -2.500000000000001332 ) ) ;
#705 = CARTESIAN_POINT ( 'NONE',  ( 4.621347029917726168, 1.908772861692954237, 4.883837314020292197 ) ) ;
#706 = AXIS2_PLACEMENT_3D ( 'NONE', #6791, #31874, #14139 ) ;
#707 = CARTESIAN_POINT ( 'NONE',  ( 9.834375000614517859, 5.824947211148865298E-16, -4.756430356249998326 ) ) ;
#708 = CARTESIAN_POINT ( 'NONE',  ( 29.59687500061451715, -3.027376345333610441, -5.243569643749999898 ) ) ;
#709 = B_SPLINE_CURVE_WITH_KNOTS ( 'NONE', 3,
 ( #61858, #17153, #39711, #5719, #62940, #22338, #17864, #44890, #62229, #23420 ),
 .UNSPECIFIED., .F., .F.,
 ( 4, 3, 3, 4 ),
 ( 1.810050118334583309E-16, 0.0001572268011904103229, 0.0003144534009725573147, 0.0005711762704777365160 ),
 .UNSPECIFIED. ) ;
#710 = CARTESIAN_POINT ( 'NONE',  ( -1.999999999999997113, 11.18750000122903288, -26.53589838486224295 ) ) ;
#711 = CARTESIAN_POINT ( 'NONE',  ( 2.121784821875001281, 19.55937500061451573, -26.32496088578401938 ) ) ;
#712 = CARTESIAN_POINT ( 'NONE',  ( 5.850000001229035185, -2.886751345948129988, 4.999999999999997335 ) ) ;
#713 = CARTESIAN_POINT ( 'NONE',  ( 7.537500000000002309, -2.886751345948129988, 4.999999999999997335 ) ) ;
#714 =( BOUNDED_CURVE ( )  B_SPLINE_CURVE ( 2, ( #55045, #54322, #32143, #43600, #3352, #48777, #59843, #48414, #25874 ),
 .UNSPECIFIED., .F., .F. ) 
 B_SPLINE_CURVE_WITH_KNOTS ( ( 3, 2, 2, 2, 3 ),
 ( 0.1413043478260869734, 0.1449275362318840632, 0.1521739130434782705, 0.1594202898550724501, 0.1630434782608695676 ),
 .UNSPECIFIED. ) 
 CURVE ( )  GEOMETRIC_REPRESENTATION_ITEM ( )  RATIONAL_B_SPLINE_CURVE ( ( 0.9330127018922194093, 0.9330127018922196314, 1.000000000000000000, 0.8660254037844387076, 1.000000000000000000, 0.8660254037844387076, 1.000000000000000000, 0.9330127018922190762, 0.9330127018922194093 ) ) 
 REPRESENTATION_ITEM ( '' )  );
#715 = CARTESIAN_POINT ( 'NONE',  ( 3.900000001229034563, 5.773502691896255534, 3.535250795749688894E-16 ) ) ;
#716 = CARTESIAN_POINT ( 'NONE',  ( 12.53437500061451537, 6.421520780324663323E-16, -5.243569643749999010 ) ) ;
#717 = CARTESIAN_POINT ( 'NONE',  ( 24.71250000122903145, 0.000000000000000000, 4.999999999999998224 ) ) ;
#718 = CARTESIAN_POINT ( 'NONE',  ( 3.871875000614519280, -6.054752690667223547, -1.112240025338166033E-15 ) ) ;
#719 = DIRECTION ( 'NONE',  ( -0.000000000000000000, -1.000000000000000000, -0.000000000000000000 ) ) ;
#720 = CARTESIAN_POINT ( 'NONE',  ( 29.47500000122903430, 2.886751345948139313, -4.999999999999980460 ) ) ;
#721 = EDGE_CURVE ( 'NONE', #60301, #16877, #21451, .T. ) ;
#722 = CARTESIAN_POINT ( 'NONE',  ( 11.14687500061451608, -3.027376345333610441, -5.243569643749999898 ) ) ;
#723 = CARTESIAN_POINT ( 'NONE',  ( 14.40937500061451715, 4.541064518000418104, -2.621784821874998173 ) ) ;
#724 = CARTESIAN_POINT ( 'NONE',  ( 3.756430356250000102, 12.64062499938548356, 30.00000000000000000 ) ) ;
#725 = CARTESIAN_POINT ( 'NONE',  ( 6.899999999999999467, 4.330127018922192761, -2.499999999999997780 ) ) ;
#726 = CARTESIAN_POINT ( 'NONE',  ( 4.243569643749999898, 17.29062500061459318, 32.45002607614398471 ) ) ;
#727 = CARTESIAN_POINT ( 'NONE',  ( 20.63437500061451857, 6.421520780324663323E-16, -5.243569643749999010 ) ) ;
#728 = CARTESIAN_POINT ( 'NONE',  ( 26.73750000122903003, 6.123233995736764310E-16, -4.999999999999998224 ) ) ;
#729 = CARTESIAN_POINT ( 'NONE',  ( 18.23437500061451644, -2.746126346562642428, -4.756430356249999214 ) ) ;
#730 = CARTESIAN_POINT ( 'NONE',  ( 22.97812500061451857, 4.541064518000418104, 2.621784821874999949 ) ) ;
#731 = CARTESIAN_POINT ( 'NONE',  ( 14.87812500061451537, 4.541064518000418104, 2.621784821874999949 ) ) ;
#732 = CARTESIAN_POINT ( 'NONE',  ( 24.98437500061451289, -2.746126346562642428, -4.756430356249999214 ) ) ;
#733 = CARTESIAN_POINT ( 'NONE',  ( 12.60937500061451821, 4.541064518000418104, -2.621784821874998173 ) ) ;
#734 = CARTESIAN_POINT ( 'NONE',  ( 29.39999999999999858, 4.330127018922192761, -2.499999999999997780 ) ) ;
#735 = CARTESIAN_POINT ( 'NONE',  ( 25.42500000122903359, 2.886751345948129099, -4.999999999999998224 ) ) ;
#736 = CARTESIAN_POINT ( 'NONE',  ( 28.72500000000000142, -4.330127018922194537, 2.499999999999995559 ) ) ;
#737 = CARTESIAN_POINT ( 'NONE',  ( 10.84687500061451892, 6.054752690667223547, 3.707466751127219781E-16 ) ) ;
#738 = CARTESIAN_POINT ( 'NONE',  ( 29.67187500061451644, 3.027376345333613106, -5.243569643749998122 ) ) ;
#739 = CARTESIAN_POINT ( 'NONE',  ( 3.046875000614519990, -3.027376345333610441, -5.243569643749999898 ) ) ;
#740 = DIRECTION ( 'NONE',  ( -1.000000000000000000, -0.000000000000000000, -0.000000000000000000 ) ) ;
#741 = CARTESIAN_POINT ( 'NONE',  ( 21.68437500061451573, 4.541064518000418104, 2.621784821874999949 ) ) ;
#742 = CARTESIAN_POINT ( 'NONE',  ( 15.38437500061451679, 4.541064518000418104, 2.621784821874999949 ) ) ;
#743 = CARTESIAN_POINT ( 'NONE',  ( -7.967954043666661671E-16, 18.49062499938548143, 34.33755215474603517 ) ) ;
#744 = CARTESIAN_POINT ( 'NONE',  ( 25.87500000000000000, 4.330127018922191873, 2.499999999999999556 ) ) ;
#745 = CARTESIAN_POINT ( 'NONE',  ( 4.575000001229033941, -5.773502691896255534, -1.060575238724906372E-15 ) ) ;
#746 = CARTESIAN_POINT ( 'NONE',  ( 26.14687500061451431, 5.492252693125287522, 3.363034840372157021E-16 ) ) ;
#747 = CARTESIAN_POINT ( 'NONE',  ( 17.09062500061451573, 6.054752690667223547, 3.707466751127219781E-16 ) ) ;
#748 = CARTESIAN_POINT ( 'NONE',  ( 5.887500000000000178, -2.886751345948125991, -5.000000000000000000 ) ) ;
#749 = CARTESIAN_POINT ( 'NONE',  ( 1.999999999999998668, 13.66250000122903607, 26.53589838486224650 ) ) ;
#750 = CARTESIAN_POINT ( 'NONE',  ( 16.16250000000000142, -5.773502691896255534, -1.060575238724906372E-15 ) ) ;
#751 = CARTESIAN_POINT ( 'NONE',  ( 2.121784821875001281, 12.30312500061451608, 33.67503911421598417 ) ) ;
#752 = CARTESIAN_POINT ( 'NONE',  ( -2.000000000000001776, 16.40000000000000213, 33.46410161513775705 ) ) ;
#753 = CARTESIAN_POINT ( 'NONE',  ( 26.10937500061451644, 4.541064518000418104, -2.621784821874998173 ) ) ;
#754 = AXIS2_PLACEMENT_3D ( 'NONE', #48020, #47643, #36558 ) ;
#755 = VERTEX_POINT ( 'NONE', #11435 ) ;
#756 = CARTESIAN_POINT ( 'NONE',  ( 23.09062500061451573, -3.027376345333614438, 5.243569643749998122 ) ) ;
#757 = CARTESIAN_POINT ( 'NONE',  ( 21.94687500061451857, -3.027376345333610441, -5.243569643749999898 ) ) ;
#758 = CARTESIAN_POINT ( 'NONE',  ( 3.525000000000000355, -4.330127018922194537, 2.499999999999995559 ) ) ;
#759 = CARTESIAN_POINT ( 'NONE',  ( 6.703125000614516438, 4.541064518000418104, -2.621784821874998173 ) ) ;
#760 = CARTESIAN_POINT ( 'NONE',  ( 24.77812500061451217, 4.541064518000418104, 2.621784821874999949 ) ) ;
#761 = CARTESIAN_POINT ( 'NONE',  ( 13.32187500061451502, -6.054752690667223547, -1.112240025338166033E-15 ) ) ;
#762 = CARTESIAN_POINT ( 'NONE',  ( 16.13437500061451502, 6.421520780324663323E-16, -5.243569643749999010 ) ) ;
#763 = CARTESIAN_POINT ( 'NONE',  ( 2.121784821874999061, 18.75312500061451715, 26.32496088578401583 ) ) ;
#764 = CARTESIAN_POINT ( 'NONE',  ( 18.60000000122903430, -2.886751345948125991, -5.000000000000000000 ) ) ;
#765 = CARTESIAN_POINT ( 'NONE',  ( 15.19687500061451679, -2.746126346562641984, -4.756430356249999214 ) ) ;
#766 = CARTESIAN_POINT ( 'NONE',  ( 9.440625000614517148, 6.054752690667223547, 3.707466751127219781E-16 ) ) ;
#767 = CARTESIAN_POINT ( 'NONE',  ( 6.046875000614519102, -3.027376345333614438, 5.243569643749998122 ) ) ;
#768 = CARTESIAN_POINT ( 'NONE',  ( 5.259375000614518569, -4.541064518000417216, -2.621784821875001281 ) ) ;
#769 = ORIENTED_EDGE ( 'NONE', *, *, #18393, .F. ) ;
#770 = CARTESIAN_POINT ( 'NONE',  ( 24.79687500061451999, 6.054752690667223547, 3.707466751127219781E-16 ) ) ;
#771 = CARTESIAN_POINT ( 'NONE',  ( 15.85312500061451857, 0.000000000000000000, 5.243569643749999010 ) ) ;
#772 = CARTESIAN_POINT ( 'NONE',  ( 26.47500000122903074, 2.886751345948126879, 4.999999999999999112 ) ) ;
#773 =( BOUNDED_CURVE ( )  B_SPLINE_CURVE ( 2, ( #17330, #46145, #39889, #18045, #63124, #12520, #27707 ),
 .UNSPECIFIED., .F., .F. ) 
 B_SPLINE_CURVE_WITH_KNOTS ( ( 3, 2, 2, 3 ),
 ( 0.7500000000000000000, 0.7527777777777777679, 0.7555555555555555358, 0.7583333333333333037 ),
 .UNSPECIFIED. ) 
 CURVE ( )  GEOMETRIC_REPRESENTATION_ITEM ( )  RATIONAL_B_SPLINE_CURVE ( ( 1.000000000000000000, 0.8660254037844387076, 1.000000000000000000, 0.8660254037844387076, 1.000000000000000000, 0.8660254037844387076, 1.000000000000000000 ) ) 
 REPRESENTATION_ITEM ( '' )  );
#774 = CARTESIAN_POINT ( 'NONE',  ( 27.66562500061451146, -6.054752690667223547, -1.112240025338166033E-15 ) ) ;
#775 = CARTESIAN_POINT ( 'NONE',  ( 20.67187500061451289, 3.027376345333613106, -5.243569643749998122 ) ) ;
#776 = CARTESIAN_POINT ( 'NONE',  ( 16.00312500061451715, -4.541064518000417216, -2.621784821875001281 ) ) ;
#777 = CARTESIAN_POINT ( 'NONE',  ( 1.999999999999998668, 10.40000000000000213, 26.53589838486224650 ) ) ;
#778 = CARTESIAN_POINT ( 'NONE',  ( 21.85312500061451502, -4.541064518000417216, -2.621784821875001281 ) ) ;
#779 = CARTESIAN_POINT ( 'NONE',  ( 3.262500001229035718, -4.330127018922190985, -2.500000000000001332 ) ) ;
#780 = ORIENTED_EDGE ( 'NONE', *, *, #27131, .T. ) ;
#781 = CARTESIAN_POINT ( 'NONE',  ( 26.92499999999999716, -4.330127018922194537, 2.499999999999995559 ) ) ;
#782 = CARTESIAN_POINT ( 'NONE',  ( -1.999999999999997113, 12.42500000000000249, -26.53589838486224295 ) ) ;
#783 = CARTESIAN_POINT ( 'NONE',  ( 1.878215178124997609, 18.52812499938548285, 33.25316411605952993 ) ) ;
#784 = CARTESIAN_POINT ( 'NONE',  ( 29.31562500061451715, 3.027376345333611329, 5.243569643749999010 ) ) ;
#785 = CARTESIAN_POINT ( 'NONE',  ( 10.56562500061451715, -6.054752690667223547, -1.112240025338166033E-15 ) ) ;
#786 = CARTESIAN_POINT ( 'NONE',  ( 21.63750000122903572, -4.330127018922194537, 2.499999999999995559 ) ) ;
#787 = CARTESIAN_POINT ( 'NONE',  ( 27.59062500061451573, -3.027376345333614438, 5.243569643749998122 ) ) ;
#788 = CARTESIAN_POINT ( 'NONE',  ( 28.38749999999999929, -2.886751345948125991, -5.000000000000000000 ) ) ;
#789 = CARTESIAN_POINT ( 'NONE',  ( 2.000000000000001332, 18.46250000122903501, -26.53589838486224650 ) ) ;
#790 = CARTESIAN_POINT ( 'NONE',  ( 25.27500000122903145, -5.773502691896255534, -1.060575238724906372E-15 ) ) ;
#791 = CARTESIAN_POINT ( 'NONE',  ( 13.19062500061451537, -3.027376345333614438, 5.243569643749998122 ) ) ;
#792 = ORIENTED_EDGE ( 'NONE', *, *, #47637, .T. ) ;
#793 = EDGE_CURVE ( 'NONE', #12747, #52141, #14130, .T. ) ;
#794 = CARTESIAN_POINT ( 'NONE',  ( 7.115625000614516082, 3.027376345333613106, -5.243569643749998122 ) ) ;
#795 = CARTESIAN_POINT ( 'NONE',  ( 5.090625000614516615, -3.027376345333614438, 5.243569643749998122 ) ) ;
#796 = AXIS2_PLACEMENT_3D ( 'NONE', #15994, #54797, #66618 ) ;
#797 = CARTESIAN_POINT ( 'NONE',  ( 17.29687500061451999, -2.746126346562646425, 4.756430356249996549 ) ) ;
#798 = EDGE_CURVE ( 'NONE', #16648, #45031, #59438, .T. ) ;
#799 = CARTESIAN_POINT ( 'NONE',  ( -4.243569643749999898, 19.85937500061451644, -30.00000000000000000 ) ) ;
#800 = CARTESIAN_POINT ( 'NONE',  ( 15.37500000000000000, 6.123233995736764310E-16, -4.999999999999998224 ) ) ;
#801 = ADVANCED_FACE ( 'NONE', ( #17678 ), #50957, .F. ) ;
#802 = CARTESIAN_POINT ( 'NONE',  ( 16.77187500061451786, 3.027376345333611329, 5.243569643749999010 ) ) ;
#803 = CARTESIAN_POINT ( 'NONE',  ( 11.25000000122903288, -2.886751345948129988, 4.999999999999997335 ) ) ;
#804 = CARTESIAN_POINT ( 'NONE',  ( 19.35937500061451644, 4.541064518000418104, -2.621784821874998173 ) ) ;
#805 = CARTESIAN_POINT ( 'NONE',  ( 16.35000000000000142, 4.330127018922192761, -2.499999999999997780 ) ) ;
#806 = CARTESIAN_POINT ( 'NONE',  ( 21.34687500061451715, -3.027376345333614438, 5.243569643749998122 ) ) ;
#807 = CARTESIAN_POINT ( 'NONE',  ( 2.121784821875001281, 15.00312500061451715, -26.32496088578401938 ) ) ;
#808 = DIRECTION ( 'NONE',  ( 0.000000000000000000, 1.000000000000000000, -8.673617379884036705E-17 ) ) ;
#809 = CARTESIAN_POINT ( 'NONE',  ( 26.52187500061451431, 4.119189519843966529, 2.378215178124999607 ) ) ;
#810 = CARTESIAN_POINT ( 'NONE',  ( 20.73750000000000071, -2.886751345948092684, -5.000000000000057732 ) ) ;
#811 = CARTESIAN_POINT ( 'NONE',  ( 27.36562500061451786, 3.027376345333613106, -5.243569643749998122 ) ) ;
#812 =( NAMED_UNIT ( * ) SI_UNIT ( $, .STERADIAN. ) SOLID_ANGLE_UNIT ( ) );
#813 = CARTESIAN_POINT ( 'NONE',  ( 28.58437500061451786, -4.541064518000419881, 2.621784821874995952 ) ) ;
#814 = CARTESIAN_POINT ( 'NONE',  ( 23.55000000000000071, 4.330127018922192761, -2.499999999999997780 ) ) ;
#815 = CARTESIAN_POINT ( 'NONE',  ( 7.040625000614517681, -3.027376345333610441, -5.243569643749999898 ) ) ;
#816 = CARTESIAN_POINT ( 'NONE',  ( 23.85937500061451644, 2.746126346562643317, 4.756430356249998326 ) ) ;
#817 = CARTESIAN_POINT ( 'NONE',  ( 19.32187500061451857, 3.027376345333613106, -5.243569643749998122 ) ) ;
#818 = CARTESIAN_POINT ( 'NONE',  ( 10.32187500061451679, 4.119189519843966529, 2.378215178124999607 ) ) ;
#819 = CARTESIAN_POINT ( 'NONE',  ( 4.865625000614517859, 3.027376345333613106, -5.243569643749998122 ) ) ;
#820 = CARTESIAN_POINT ( 'NONE',  ( 9.571875000614518569, 3.027376345333611329, 5.243569643749999010 ) ) ;
#821 = ORIENTED_EDGE ( 'NONE', *, *, #39594, .T. ) ;
#822 = CARTESIAN_POINT ( 'NONE',  ( 22.09687500061451715, 6.054752690667223547, 3.707466751127219781E-16 ) ) ;
#823 = CARTESIAN_POINT ( 'NONE',  ( 16.72500000000000142, 6.123233995736764310E-16, -4.999999999999998224 ) ) ;
#824 = CARTESIAN_POINT ( 'NONE',  ( 29.62500000000000000, -4.330127018922194537, 2.499999999999995559 ) ) ;
#826 = EDGE_CURVE ( 'NONE', #30532, #37056, #33986, .T. ) ;
#825 = CARTESIAN_POINT ( 'NONE',  ( 29.10937500061451644, -4.541064518000417216, -2.621784821875001281 ) ) ;
#827 = CARTESIAN_POINT ( 'NONE',  ( 29.55000000000000071, 0.000000000000000000, 4.999999999999998224 ) ) ;
#828 = CARTESIAN_POINT ( 'NONE',  ( 3.319923472288579536, -4.210009680006762345, 3.195188621371491511 ) ) ;
#829 = VERTEX_POINT ( 'NONE', #12152 ) ;
#830 = CARTESIAN_POINT ( 'NONE',  ( 9.299999999999998934, 0.000000000000000000, 4.999999999999998224 ) ) ;
#831 = CARTESIAN_POINT ( 'NONE',  ( 11.82187500061451502, -4.119189519843968306, 2.378215178124996054 ) ) ;
#832 = CARTESIAN_POINT ( 'NONE',  ( 23.95312500061451289, 0.000000000000000000, 5.243569643749999010 ) ) ;
#833 = CARTESIAN_POINT ( 'NONE',  ( 13.98750000000000249, -2.886751345948125991, -5.000000000000000000 ) ) ;
#834 = CARTESIAN_POINT ( 'NONE',  ( 10.83750000122903501, -4.330127018922194537, 2.499999999999995559 ) ) ;
#835 = CARTESIAN_POINT ( 'NONE',  ( 8.090625000614515727, 6.054752690667223547, 3.707466751127219781E-16 ) ) ;
#836 = CARTESIAN_POINT ( 'NONE',  ( 25.19999999999999929, -4.330127018922190985, -2.500000000000001332 ) ) ;
#837 = CARTESIAN_POINT ( 'NONE',  ( 20.84062500061451573, -3.027376345333614438, 5.243569643749998122 ) ) ;
#838 = CARTESIAN_POINT ( 'NONE',  ( 18.71250000122903145, 4.330127018922192761, -2.499999999999997780 ) ) ;
#839 = CARTESIAN_POINT ( 'NONE',  ( 28.83750000122903145, -4.330127018922194537, 2.499999999999995559 ) ) ;
#840 = CARTESIAN_POINT ( 'NONE',  ( -3.756430356250000102, 16.46562499938548285, 30.00000000000000000 ) ) ;
#841 = CARTESIAN_POINT ( 'NONE',  ( 7.124999999999999112, -4.330127018922194537, 2.499999999999995559 ) ) ;
#842 = ORIENTED_EDGE ( 'NONE', *, *, #18114, .T. ) ;
#843 = CARTESIAN_POINT ( 'NONE',  ( 20.99062500061451431, -3.027376345333610441, -5.243569643749999898 ) ) ;
#844 = CARTESIAN_POINT ( 'NONE',  ( 29.46562500061451573, -6.054752690667223547, -1.112240025338166033E-15 ) ) ;
#845 = CARTESIAN_POINT ( 'NONE',  ( 28.43437500061451573, 4.541064518000418104, 2.621784821874999949 ) ) ;
#846 = CARTESIAN_POINT ( 'NONE',  ( 18.30937500061451928, -4.541064518000417216, -2.621784821875001281 ) ) ;
#847 = CARTESIAN_POINT ( 'NONE',  ( 16.04062500061451857, -3.027376345333610441, -5.243569643749999898 ) ) ;
#848 = AXIS2_PLACEMENT_3D ( 'NONE', #69404, #35764, #52400 ) ;
#849 = LINE ( 'NONE', #7827, #71099 ) ;
#850 = CARTESIAN_POINT ( 'NONE',  ( 4.603125000614518569, 0.000000000000000000, 5.243569643749999010 ) ) ;
#851 = VECTOR ( 'NONE', #69149, 1000.000000000000000 ) ;
#852 = CARTESIAN_POINT ( 'NONE',  ( 27.48750000122903359, -4.330127018922194537, 2.499999999999995559 ) ) ;
#853 = CARTESIAN_POINT ( 'NONE',  ( 21.38437500061451502, -4.119189519843968306, 2.378215178124996054 ) ) ;
#854 = CARTESIAN_POINT ( 'NONE',  ( 19.26562500061451644, 3.027376345333612662, -5.243569643749998122 ) ) ;
#855 = CARTESIAN_POINT ( 'NONE',  ( 1.071796769724489895, 11.42990381179669868, -34.00000000000000000 ) ) ;
#856 = CARTESIAN_POINT ( 'NONE',  ( 4.162500001229033408, -4.330127018922190985, -2.500000000000001332 ) ) ;
#857 = CARTESIAN_POINT ( 'NONE',  ( 13.80937500061451750, -4.541064518000417216, -2.621784821875001281 ) ) ;
#858 = CARTESIAN_POINT ( 'NONE',  ( 12.87187500061451750, -6.054752690667223547, -1.112240025338166033E-15 ) ) ;
#859 = CARTESIAN_POINT ( 'NONE',  ( 20.59687500061451360, -3.027376345333610441, -5.243569643749999898 ) ) ;
#860 = VERTEX_POINT ( 'NONE', #61310 ) ;
#861 = CARTESIAN_POINT ( 'NONE',  ( 29.36250000000000071, 2.886751345948160630, -4.999999999999943157 ) ) ;
#862 = CARTESIAN_POINT ( 'NONE',  ( 24.25312500061451715, 4.541064518000418104, -2.621784821874998173 ) ) ;
#863 = CARTESIAN_POINT ( 'NONE',  ( 18.60937500061451644, 0.000000000000000000, 5.243569643749999010 ) ) ;
#864 = CARTESIAN_POINT ( 'NONE',  ( 23.24062500061451786, -3.027376345333610441, -5.243569643749999898 ) ) ;
#865 = CARTESIAN_POINT ( 'NONE',  ( 15.05625000122903323, 4.330127018922192761, -2.499999999999997780 ) ) ;
#866 = CARTESIAN_POINT ( 'NONE',  ( 3.999999999999998668, 15.76249999999999751, 27.69059892324149175 ) ) ;
#867 = CARTESIAN_POINT ( 'NONE',  ( 28.97812500061451502, -4.541064518000419881, 2.621784821874995952 ) ) ;
#868 = CARTESIAN_POINT ( 'NONE',  ( 9.262500001229033941, 4.330127018922192761, -2.499999999999997780 ) ) ;
#869 = CARTESIAN_POINT ( 'NONE',  ( 6.487500001229034474, 6.123233995736764310E-16, -4.999999999999998224 ) ) ;
#870 = CARTESIAN_POINT ( 'NONE',  ( -3.999999999999999556, 19.06249999999999645, -32.30940107675850470 ) ) ;
#871 = CARTESIAN_POINT ( 'NONE',  ( 26.36250000122903003, 4.330127018922192761, -2.499999999999997780 ) ) ;
#872 = CARTESIAN_POINT ( 'NONE',  ( -1.999999999999999112, 19.34374999877096712, 26.53589838486224650 ) ) ;
#873 = CARTESIAN_POINT ( 'NONE',  ( 16.59375000122903288, -2.886751345948129988, 4.999999999999997335 ) ) ;
#874 = CARTESIAN_POINT ( 'NONE',  ( 9.459375000614517859, 4.541064518000418104, -2.621784821874998173 ) ) ;
#875 = CARTESIAN_POINT ( 'NONE',  ( 24.48749999999999716, 5.773502691896255534, 3.535250795749688401E-16 ) ) ;
#876 = CARTESIAN_POINT ( 'NONE',  ( 16.86562500061451786, -6.054752690667223547, -1.112240025338166033E-15 ) ) ;
#877 = CARTESIAN_POINT ( 'NONE',  ( 9.946875000614516793, 6.054752690667223547, 3.707466751127219781E-16 ) ) ;
#878 = CARTESIAN_POINT ( 'NONE',  ( 29.06250000122903288, 4.330127018922192761, -2.499999999999997780 ) ) ;
#879 = CARTESIAN_POINT ( 'NONE',  ( 19.77187500061451786, 3.027376345333612662, -5.243569643749998122 ) ) ;
#880 = CARTESIAN_POINT ( 'NONE',  ( 6.496875000614517504, -3.027376345333614438, 5.243569643749998122 ) ) ;
#881 = CARTESIAN_POINT ( 'NONE',  ( 15.00000000122903465, -2.886751345948126435, -5.000000000000000000 ) ) ;
#882 = CARTESIAN_POINT ( 'NONE',  ( 1.626862140677534273E-15, 17.86250000000000071, 34.00000000000000000 ) ) ;
#883 = CARTESIAN_POINT ( 'NONE',  ( 7.378125000614518036, -4.541064518000419881, 2.621784821874995952 ) ) ;
#884 = CARTESIAN_POINT ( 'NONE',  ( 19.97812500061451502, -4.541064518000419881, 2.621784821874995952 ) ) ;
#885 = VERTEX_POINT ( 'NONE', #33238 ) ;
#886 = CARTESIAN_POINT ( 'NONE',  ( 6.187500001229032875, 4.330127018922191873, 2.499999999999999556 ) ) ;
#887 = CARTESIAN_POINT ( 'NONE',  ( 14.91562500061451679, 3.027376345333611329, 5.243569643749999010 ) ) ;
#888 = CARTESIAN_POINT ( 'NONE',  ( 12.89062500061451821, -3.027376345333610441, -5.243569643749999898 ) ) ;
#889 = CARTESIAN_POINT ( 'NONE',  ( 24.60937500061451644, -4.119189519843965641, -2.378215178125001383 ) ) ;
#890 = CARTESIAN_POINT ( 'NONE',  ( 12.22499999999999964, 6.123233995736764310E-16, -4.999999999999998224 ) ) ;
#891 = CARTESIAN_POINT ( 'NONE',  ( 8.025000001229035007, 2.886751345948126879, 4.999999999999999112 ) ) ;
#892 = CARTESIAN_POINT ( 'NONE',  ( 6.553125000614518747, -4.541064518000417216, -2.621784821875001281 ) ) ;
#893 = EDGE_CURVE ( 'NONE', #53197, #52280, #67237, .T. ) ;
#894 = CARTESIAN_POINT ( 'NONE',  ( 18.18750000122903288, 6.123233995736764310E-16, -4.999999999999998224 ) ) ;
#895 = CARTESIAN_POINT ( 'NONE',  ( 23.96249999999999858, 2.886751345948129099, -4.999999999999998224 ) ) ;
#896 = CARTESIAN_POINT ( 'NONE',  ( 9.001249775931846008E-16, 10.07187500061451857, -25.09994784771203058 ) ) ;
#897 = CARTESIAN_POINT ( 'NONE',  ( 4.898587196589411843E-16, 20.00000000000000000, 33.99999999999999289 ) ) ;
#898 = CARTESIAN_POINT ( 'NONE',  ( 3.000000001229032875, 5.773502691896255534, 3.535250795749688894E-16 ) ) ;
#899 = VECTOR ( 'NONE', #33176, 1000.000000000000000 ) ;
#900 = CARTESIAN_POINT ( 'NONE',  ( 3.037500001229032964, 4.330127018922191873, 2.499999999999999556 ) ) ;
#901 = CARTESIAN_POINT ( 'NONE',  ( 17.97187500061451715, 3.027376345333613106, -5.243569643749998122 ) ) ;
#902 = CARTESIAN_POINT ( 'NONE',  ( 22.96875000122903288, -5.773502691896255534, -1.060575238724906372E-15 ) ) ;
#903 = CARTESIAN_POINT ( 'NONE',  ( 13.07812500061451821, 4.541064518000418104, 2.621784821874999949 ) ) ;
#904 = CARTESIAN_POINT ( 'NONE',  ( 9.993750001229033231, -2.886751345948125991, -5.000000000000000000 ) ) ;
#905 = CARTESIAN_POINT ( 'NONE',  ( 9.037499999999997868, -2.886751345948181946, -4.999999999999904077 ) ) ;
#906 = CARTESIAN_POINT ( 'NONE',  ( 28.95937500061451431, 0.000000000000000000, 5.243569643749999010 ) ) ;
#907 = CARTESIAN_POINT ( 'NONE',  ( 26.74687500061451573, -3.027376345333614438, 5.243569643749998122 ) ) ;
#908 = CARTESIAN_POINT ( 'NONE',  ( 19.39687500061451786, 0.000000000000000000, 4.756430356249998326 ) ) ;
#909 = CARTESIAN_POINT ( 'NONE',  ( 12.89062500061451821, -3.027376345333610441, -5.243569643749999898 ) ) ;
#910 = CARTESIAN_POINT ( 'NONE',  ( 10.28437500061451715, 6.421520780324663323E-16, -5.243569643749999010 ) ) ;
#911 = ORIENTED_EDGE ( 'NONE', *, *, #71191, .F. ) ;
#912 = CARTESIAN_POINT ( 'NONE',  ( 27.52500000000000213, 6.123233995736764310E-16, -4.999999999999998224 ) ) ;
#913 = CARTESIAN_POINT ( 'NONE',  ( 20.39062500061451644, -3.027376345333614438, 5.243569643749998122 ) ) ;
#914 = CARTESIAN_POINT ( 'NONE',  ( 3.138870840040013821, 3.891985242736291539, -3.513904600516652099 ) ) ;
#915 = LINE ( 'NONE', #46332, #51391 ) ;
#916 = CARTESIAN_POINT ( 'NONE',  ( 10.38750000000000107, -2.886751345948125991, -5.000000000000000000 ) ) ;
#917 = CARTESIAN_POINT ( 'NONE',  ( 20.66250000122903074, 0.000000000000000000, 4.999999999999998224 ) ) ;
#918 = CARTESIAN_POINT ( 'NONE',  ( 15.10312500061451502, -4.541064518000417216, -2.621784821875001281 ) ) ;
#919 = CARTESIAN_POINT ( 'NONE',  ( 10.20937500061451608, 2.746126346562645981, -4.756430356249997438 ) ) ;
#920 = ORIENTED_EDGE ( 'NONE', *, *, #27236, .F. ) ;
#921 = CARTESIAN_POINT ( 'NONE',  ( 17.96250000000000213, -5.773502691896255534, -1.060575238724906372E-15 ) ) ;
#922 =( BOUNDED_CURVE ( )  B_SPLINE_CURVE ( 2, ( #607, #7219, #22752, #18276, #6498, #23113, #45303 ),
 .UNSPECIFIED., .F., .F. ) 
 B_SPLINE_CURVE_WITH_KNOTS ( ( 3, 2, 2, 3 ),
 ( 0.1799999999999999378, 0.1833333333333333204, 0.1866666666666667029, 0.1900000000000000855 ),
 .UNSPECIFIED. ) 
 CURVE ( )  GEOMETRIC_REPRESENTATION_ITEM ( )  RATIONAL_B_SPLINE_CURVE ( ( 1.000000000000002220, 0.8660254037844364872, 1.000000000000000000, 0.8660254037844387076, 1.000000000000000000, 0.8660254037844353769, 1.000000000000003331 ) ) 
 REPRESENTATION_ITEM ( '' )  );
#923 = CARTESIAN_POINT ( 'NONE',  ( 22.08749999999999858, -2.886751345948125991, -5.000000000000000000 ) ) ;
#924 = CARTESIAN_POINT ( 'NONE',  ( 20.22187500061451715, 3.027376345333613106, -5.243569643749998122 ) ) ;
#925 = CARTESIAN_POINT ( 'NONE',  ( 25.11562500061451431, 3.027376345333613106, -5.243569643749998122 ) ) ;
#926 = ORIENTED_EDGE ( 'NONE', *, *, #17867, .T. ) ;
#927 = CARTESIAN_POINT ( 'NONE',  ( -1.071796769724485010, 17.05490381179669868, 34.00000000000000000 ) ) ;
#928 = CARTESIAN_POINT ( 'NONE',  ( 7.153125000614518392, 4.541064518000418104, -2.621784821874998173 ) ) ;
#929 = CARTESIAN_POINT ( 'NONE',  ( -2.498395430326213790E-14, 18.85624999877096641, 26.00000000000000000 ) ) ;
#930 = CARTESIAN_POINT ( 'NONE',  ( 13.50000000000000178, -4.330127018922190985, -2.500000000000001332 ) ) ;
#931 = CARTESIAN_POINT ( 'NONE',  ( 4.243569643749999010, 16.46562500061451573, 27.54997392385601174 ) ) ;
#932 = CARTESIAN_POINT ( 'NONE',  ( 28.00312500061451715, 0.000000000000000000, 5.243569643749999010 ) ) ;
#933 = CARTESIAN_POINT ( 'NONE',  ( -3.756430356250001434, 14.25312499938548250, 32.16877607737301048 ) ) ;
#934 = CARTESIAN_POINT ( 'NONE',  ( 26.14687500061451431, 6.054752690667223547, 3.707466751127219781E-16 ) ) ;
#935 = ORIENTED_EDGE ( 'NONE', *, *, #68490, .F. ) ;
#936 = CARTESIAN_POINT ( 'NONE',  ( 23.87812500061451715, 4.541064518000418104, 2.621784821874999949 ) ) ;
#937 = CARTESIAN_POINT ( 'NONE',  ( 24.79687500061451999, 6.054752690667223547, 3.707466751127219781E-16 ) ) ;
#938 = ADVANCED_FACE ( 'NONE', ( #56138 ), #34679, .T. ) ;
#939 = CARTESIAN_POINT ( 'NONE',  ( 9.001249775931846008E-16, 17.66562500061459318, -25.09994784771203058 ) ) ;
#940 = CARTESIAN_POINT ( 'NONE',  ( 12.00000000000000000, 0.000000000000000000, 4.999999999999998224 ) ) ;
#941 = CARTESIAN_POINT ( 'NONE',  ( 8.840625000614515727, -3.027376345333610441, -5.243569643749999898 ) ) ;
#942 = CARTESIAN_POINT ( 'NONE',  ( 28.54687500061451644, -2.746126346562646425, 4.756430356249996549 ) ) ;
#943 = CARTESIAN_POINT ( 'NONE',  ( 1.626862140677534273E-15, 11.11250000000000071, 34.00000000000000000 ) ) ;
#944 = CARTESIAN_POINT ( 'NONE',  ( 26.54062500061451146, 6.054752690667223547, 3.707466751127219781E-16 ) ) ;
#945 = CARTESIAN_POINT ( 'NONE',  ( 27.64687500061451431, -4.119189519843965641, -2.378215178125001383 ) ) ;
#946 = CARTESIAN_POINT ( 'NONE',  ( 12.45937500061451786, -4.119189519843965641, -2.378215178125001383 ) ) ;
#947 = CARTESIAN_POINT ( 'NONE',  ( 20.52187500061451786, -6.054752690667223547, -1.112240025338166033E-15 ) ) ;
#948 = CARTESIAN_POINT ( 'NONE',  ( -4.243569643749999898, 13.07187500061452035, 27.54997392385601529 ) ) ;
#949 = CARTESIAN_POINT ( 'NONE',  ( 18.60937500061451644, 0.000000000000000000, 5.243569643749999010 ) ) ;
#950 = CARTESIAN_POINT ( 'NONE',  ( 26.82187500061451857, -6.054752690667223547, -1.112240025338166033E-15 ) ) ;
#951 = CARTESIAN_POINT ( 'NONE',  ( -4.243569643749999898, 17.60937500061451999, 30.00000000000000000 ) ) ;
#952 = CARTESIAN_POINT ( 'NONE',  ( 8.503125000614515372, 4.541064518000418104, -2.621784821874998173 ) ) ;
#953 = CARTESIAN_POINT ( 'NONE',  ( 3.999999999999999112, 16.17500000000000071, 30.00000000000000000 ) ) ;
#954 = CARTESIAN_POINT ( 'NONE',  ( 3.646875000614520079, 6.054752690667223547, 3.707466751127219781E-16 ) ) ;
#955 = CARTESIAN_POINT ( 'NONE',  ( 30.00000000000000000, 0.000000000000000000, 4.999999999999998224 ) ) ;
#956 = CARTESIAN_POINT ( 'NONE',  ( 6.215625000614517504, 3.027376345333613106, -5.243569643749998122 ) ) ;
#957 = CARTESIAN_POINT ( 'NONE',  ( 10.32187500061451679, 3.027376345333613106, -5.243569643749998122 ) ) ;
#958 = CARTESIAN_POINT ( 'NONE',  ( 20.25000000122903288, -2.886751345948129988, 4.999999999999997335 ) ) ;
#959 = CARTESIAN_POINT ( 'NONE',  ( 6.571875000614517681, -6.054752690667223547, -1.112240025338166033E-15 ) ) ;
#960 = CARTESIAN_POINT ( 'NONE',  ( 6.853125000614516793, 0.000000000000000000, 5.243569643749999010 ) ) ;
#961 = CARTESIAN_POINT ( 'NONE',  ( 22.51875000122903003, -5.773502691896255534, -1.060575238724906372E-15 ) ) ;
#962 = CARTESIAN_POINT ( 'NONE',  ( 17.89687500061451431, -3.027376345333610441, -5.243569643749999898 ) ) ;
#963 = CARTESIAN_POINT ( 'NONE',  ( 4.457256472106807976, 2.265816029382255792, 4.511484450116618916 ) ) ;
#964 = VERTEX_POINT ( 'NONE', #62041 ) ;
#965 = CARTESIAN_POINT ( 'NONE',  ( 24.81562500061451715, 3.027376345333611329, 5.243569643749999010 ) ) ;
#966 = CARTESIAN_POINT ( 'NONE',  ( 9.253125000614517148, -4.541064518000417216, -2.621784821875001281 ) ) ;
#967 = CARTESIAN_POINT ( 'NONE',  ( 27.04687500061450933, 6.054752690667223547, 3.707466751127219781E-16 ) ) ;
#968 = CARTESIAN_POINT ( 'NONE',  ( 10.75312500061451715, 4.541064518000418104, -2.621784821874998173 ) ) ;
#969 = CARTESIAN_POINT ( 'NONE',  ( 4.425757632551291287, -2.326665885598202088, -4.651935364053993993 ) ) ;
#970 = CARTESIAN_POINT ( 'NONE',  ( 13.35000000122903430, 5.773502691896255534, 3.535250795749688894E-16 ) ) ;
#971 = CARTESIAN_POINT ( 'NONE',  ( 26.87812500061451360, 6.421520780324663323E-16, -5.243569643749999010 ) ) ;
#972 = CARTESIAN_POINT ( 'NONE',  ( 4.243569643749999010, 11.96562500061451750, -32.45002607614398471 ) ) ;
#973 = CARTESIAN_POINT ( 'NONE',  ( 13.50000000122903288, -2.886751345948129988, 4.999999999999997335 ) ) ;
#974 = CARTESIAN_POINT ( 'NONE',  ( 10.68750000000000000, -2.886751345948129988, 4.999999999999997335 ) ) ;
#975 = CARTESIAN_POINT ( 'NONE',  ( 19.37812500061451715, 4.541064518000418104, 2.621784821874999949 ) ) ;
#976 = CARTESIAN_POINT ( 'NONE',  ( 6.346875000614517148, 6.054752690667223547, 3.707466751127219781E-16 ) ) ;
#977 = CARTESIAN_POINT ( 'NONE',  ( 21.67500000000000071, 6.123233995736764310E-16, -4.999999999999998224 ) ) ;
#978 = CARTESIAN_POINT ( 'NONE',  ( 7.800000001229035362, -2.886751345948125991, -5.000000000000000000 ) ) ;
#979 = CARTESIAN_POINT ( 'NONE',  ( 17.06250000122903288, 0.000000000000000000, 4.999999999999998224 ) ) ;
#980 =( BOUNDED_CURVE ( )  B_SPLINE_CURVE ( 2, ( #56330, #547, #189, #6078, #16423, #33787, #16787, #50430, #67779 ),
 .UNSPECIFIED., .F., .F. ) 
 B_SPLINE_CURVE_WITH_KNOTS ( ( 3, 2, 2, 2, 3 ),
 ( 0.5543478260869565410, 0.5579710144927536586, 0.5652173913043477826, 0.5724637681159420177, 0.5760869565217391353 ),
 .UNSPECIFIED. ) 
 CURVE ( )  GEOMETRIC_REPRESENTATION_ITEM ( )  RATIONAL_B_SPLINE_CURVE ( ( 0.9330127018922194093, 0.9330127018922194093, 1.000000000000000000, 0.8660254037844387076, 1.000000000000000000, 0.8660254037844387076, 1.000000000000000000, 0.9330127018922194093, 0.9330127018922194093 ) ) 
 REPRESENTATION_ITEM ( '' )  );
#981 = CARTESIAN_POINT ( 'NONE',  ( 12.32812500061451821, -4.541064518000419881, 2.621784821874995952 ) ) ;
#982 = CARTESIAN_POINT ( 'NONE',  ( 16.19062500061451715, 6.054752690667223547, 3.707466751127219781E-16 ) ) ;
#983 = ADVANCED_FACE ( 'NONE', ( #48596 ), #31602, .F. ) ;
#984 = CARTESIAN_POINT ( 'NONE',  ( 25.01250000122903216, 4.330127018922192761, -2.499999999999997780 ) ) ;
#985 = CARTESIAN_POINT ( 'NONE',  ( 19.61249999999999716, 2.886751345948126879, 4.999999999999999112 ) ) ;
#986 = CARTESIAN_POINT ( 'NONE',  ( 23.85937500061451644, 4.541064518000418104, -2.621784821874998173 ) ) ;
#987 = FACE_OUTER_BOUND ( 'NONE', #13837, .T. ) ;
#988 = CARTESIAN_POINT ( 'NONE',  ( 9.787500001229036073, 4.330127018922191873, 2.499999999999999556 ) ) ;
#989 = CARTESIAN_POINT ( 'NONE',  ( 8.446875000614518569, -3.027376345333610441, -5.243569643749999898 ) ) ;
#990 = CARTESIAN_POINT ( 'NONE',  ( 25.24687500061451573, 6.054752690667223547, 3.707466751127219781E-16 ) ) ;
#991 =( BOUNDED_CURVE ( )  B_SPLINE_CURVE ( 2, ( #28868, #810, #72857, #67327, #50687, #16687, #39243 ),
 .UNSPECIFIED., .F., .F. ) 
 B_SPLINE_CURVE_WITH_KNOTS ( ( 3, 2, 2, 3 ),
 ( 0.3416666666666666186, 0.3444444444444444420, 0.3472222222222222099, 0.3500000000000000333 ),
 .UNSPECIFIED. ) 
 CURVE ( )  GEOMETRIC_REPRESENTATION_ITEM ( )  RATIONAL_B_SPLINE_CURVE ( ( 1.000000000000002665, 0.8660254037844360431, 1.000000000000000000, 0.8660254037844387076, 1.000000000000000000, 0.8660254037844360431, 1.000000000000002665 ) ) 
 REPRESENTATION_ITEM ( '' )  );
#992 = CARTESIAN_POINT ( 'NONE',  ( 2.971875000614517592, -6.054752690667223547, -1.112240025338166033E-15 ) ) ;
#993 = CARTESIAN_POINT ( 'NONE',  ( 24.66562500061451502, 3.027376345333613106, -5.243569643749998122 ) ) ;
#994 = CARTESIAN_POINT ( 'NONE',  ( 26.48437500061451644, 6.421520780324663323E-16, -5.243569643749999010 ) ) ;
#995 = CARTESIAN_POINT ( 'NONE',  ( 3.756430356250000102, 16.80312499938548498, 30.00000000000000000 ) ) ;
#996 = CARTESIAN_POINT ( 'NONE',  ( 19.14375000122903003, 5.773502691896255534, 3.535250795749688401E-16 ) ) ;
#997 = CARTESIAN_POINT ( 'NONE',  ( 7.246875000614518392, 6.054752690667223547, 3.707466751127219781E-16 ) ) ;
#998 = CARTESIAN_POINT ( 'NONE',  ( 1.071796769724491893, 12.48259618943233384, 33.99999999999999289 ) ) ;
#999 = CARTESIAN_POINT ( 'NONE',  ( 28.37812500061451715, 4.541064518000418104, 2.621784821874999949 ) ) ;
#1000 = CARTESIAN_POINT ( 'NONE',  ( 6.834375000614518747, 4.541064518000418104, 2.621784821874999949 ) ) ;
#1001 = CARTESIAN_POINT ( 'NONE',  ( 25.76249999999999929, 2.886751345948095793, -5.000000000000055067 ) ) ;
#1002 = CARTESIAN_POINT ( 'NONE',  ( -1.473776270879187500, 9.816672227264625405, 25.95083297442941017 ) ) ;
#1003 = CARTESIAN_POINT ( 'NONE',  ( 16.31250000000000000, 2.886751345948129099, -4.999999999999998224 ) ) ;
#1004 = ORIENTED_EDGE ( 'NONE', *, *, #41944, .T. ) ;
#1005 = CARTESIAN_POINT ( 'NONE',  ( 27.97500000000000142, 6.123233995736764310E-16, -4.999999999999998224 ) ) ;
#1006 = CARTESIAN_POINT ( 'NONE',  ( 29.44687500061451857, -3.027376345333614438, 5.243569643749998122 ) ) ;
#1007 = ORIENTED_EDGE ( 'NONE', *, *, #23321, .F. ) ;
#1008 = CARTESIAN_POINT ( 'NONE',  ( 15.10312500061451502, -4.541064518000417216, -2.621784821875001281 ) ) ;
#1009 = CARTESIAN_POINT ( 'NONE',  ( 5.615625000614517859, -6.054752690667223547, -1.112240025338166033E-15 ) ) ;
#1010 = CARTESIAN_POINT ( 'NONE',  ( 19.80937500061451217, 2.746126346562643317, 4.756430356249998326 ) ) ;
#1011 = CARTESIAN_POINT ( 'NONE',  ( 4.809375000614516615, -4.541064518000417216, -2.621784821875001281 ) ) ;
#1012 =( BOUNDED_CURVE ( )  B_SPLINE_CURVE ( 2, ( #8240, #47399, #2701, #60291, #65115, #64749, #48503 ),
 .UNSPECIFIED., .F., .F. ) 
 B_SPLINE_CURVE_WITH_KNOTS ( ( 3, 2, 2, 3 ),
 ( 0.4799999999999999267, 0.4833333333333333370, 0.4866666666666667473, 0.4900000000000001021 ),
 .UNSPECIFIED. ) 
 CURVE ( )  GEOMETRIC_REPRESENTATION_ITEM ( )  RATIONAL_B_SPLINE_CURVE ( ( 1.000000000000002220, 0.8660254037844364872, 1.000000000000000000, 0.8660254037844387076, 1.000000000000000000, 0.8660254037844342667, 1.000000000000004441 ) ) 
 REPRESENTATION_ITEM ( '' )  );
#1013 = CARTESIAN_POINT ( 'NONE',  ( 16.31250000122903288, -4.330127018922190985, -2.500000000000001332 ) ) ;
#1014 = CARTESIAN_POINT ( 'NONE',  ( 21.82499999999999574, 4.330127018922191873, 2.499999999999999556 ) ) ;
#1015 = CARTESIAN_POINT ( 'NONE',  ( 28.76249999999999929, -5.773502691896255534, -1.060575238724906372E-15 ) ) ;
#1016 = CARTESIAN_POINT ( 'NONE',  ( 5.034375000614519813, 4.541064518000418104, 2.621784821874999949 ) ) ;
#1017 = CARTESIAN_POINT ( 'NONE',  ( 8.221875000614518925, 3.027376345333611329, 5.243569643749999010 ) ) ;
#1018 = CARTESIAN_POINT ( 'NONE',  ( 20.97187500061451715, -6.054752690667223547, -1.112240025338166033E-15 ) ) ;
#1019 = DIRECTION ( 'NONE',  ( 0.000000000000000000, 0.000000000000000000, -1.000000000000000000 ) ) ;
#1020 = ORIENTED_EDGE ( 'NONE', *, *, #66019, .T. ) ;
#1021 = CARTESIAN_POINT ( 'NONE',  ( 3.009375000614516793, -4.541064518000417216, -2.621784821875001281 ) ) ;
#1022 = CARTESIAN_POINT ( 'NONE',  ( 6.750000000000002665, -4.330127018922190985, -2.500000000000001332 ) ) ;
#1023 = CARTESIAN_POINT ( 'NONE',  ( 6.946875000614517681, -3.027376345333614438, 5.243569643749998122 ) ) ;
#1024 = CARTESIAN_POINT ( 'NONE',  ( 18.97499999999999787, 6.123233995736764310E-16, -4.999999999999998224 ) ) ;
#1025 = CARTESIAN_POINT ( 'NONE',  ( 15.81562500061451537, 3.027376345333611329, 5.243569643749999010 ) ) ;
#1026 = CARTESIAN_POINT ( 'NONE',  ( 4.000000000000000000, 20.15000000000000213, 30.00000000000000000 ) ) ;
#1027 = CARTESIAN_POINT ( 'NONE',  ( 22.19999999999999574, 4.330127018922192761, -2.499999999999997780 ) ) ;
#1028 = CARTESIAN_POINT ( 'NONE',  ( 20.40937500061451715, 0.000000000000000000, 4.756430356249998326 ) ) ;
#1029 = CARTESIAN_POINT ( 'NONE',  ( 11.20312500061451644, 4.541064518000418104, -2.621784821874998173 ) ) ;
#1030 = CARTESIAN_POINT ( 'NONE',  ( 27.75937500061451502, -4.541064518000417216, -2.621784821875001281 ) ) ;
#1031 = CARTESIAN_POINT ( 'NONE',  ( -2.121784821874996840, 19.03437500061451715, 33.67503911421598417 ) ) ;
#1032 = CARTESIAN_POINT ( 'NONE',  ( 27.23437500061451644, -4.541064518000419881, 2.621784821874995952 ) ) ;
#1033 = CARTESIAN_POINT ( 'NONE',  ( 8.062500000000000000, -5.773502691896255534, -1.060575238724906372E-15 ) ) ;
#1034 = CARTESIAN_POINT ( 'NONE',  ( -3.999999999999997335, 13.40000000122903323, 32.30940107675850470 ) ) ;
#1035 = CARTESIAN_POINT ( 'NONE',  ( 6.750000001229033764, -2.886751345948129988, 4.999999999999997335 ) ) ;
#1036 = CARTESIAN_POINT ( 'NONE',  ( 18.53437500061451715, 4.541064518000418104, 2.621784821874999949 ) ) ;
#1037 = CARTESIAN_POINT ( 'NONE',  ( 12.30937500061451573, 0.000000000000000000, 5.243569643749999010 ) ) ;
#1038 = CARTESIAN_POINT ( 'NONE',  ( -0.1398361002794802910, 5.000000000000000000, -33.99999999999998579 ) ) ;
#1039 = ORIENTED_EDGE ( 'NONE', *, *, #67203, .F. ) ;
#1040 = CARTESIAN_POINT ( 'NONE',  ( 14.20312500061451644, -4.541064518000417216, -2.621784821875001281 ) ) ;
#1041 = CARTESIAN_POINT ( 'NONE',  ( 26.06250000122903288, 0.000000000000000000, 4.999999999999998224 ) ) ;
#1042 = CARTESIAN_POINT ( 'NONE',  ( 12.42187500061451821, -6.054752690667223547, -1.112240025338166033E-15 ) ) ;
#1043 = CARTESIAN_POINT ( 'NONE',  ( -1.626862140677534273E-15, 20.43124999877096570, 34.00000000000000000 ) ) ;
#1044 = CARTESIAN_POINT ( 'NONE',  ( 13.56562500061451892, 3.027376345333611329, 5.243569643749999010 ) ) ;
#1045 = CARTESIAN_POINT ( 'NONE',  ( 29.60625000122903216, 0.000000000000000000, 4.999999999999998224 ) ) ;
#1046 = CARTESIAN_POINT ( 'NONE',  ( 23.67187500061451999, -6.054752690667223547, -1.112240025338166033E-15 ) ) ;
#1047 = CARTESIAN_POINT ( 'NONE',  ( 2.874095310376903356, -4.091409605186981047, 3.279548391533174012 ) ) ;
#1048 = CARTESIAN_POINT ( 'NONE',  ( 11.88750000122903216, 6.123233995736764310E-16, -4.999999999999998224 ) ) ;
#1049 = CARTESIAN_POINT ( 'NONE',  ( 8.521875000614517859, 2.746126346562645981, -4.756430356249997438 ) ) ;
#1050 = CARTESIAN_POINT ( 'NONE',  ( 65.00000000000000000, 9.000000000000000000, 0.000000000000000000 ) ) ;
#1051 = CARTESIAN_POINT ( 'NONE',  ( -3.000416591977282496E-16, 16.14687500061451786, -34.90005215228797653 ) ) ;
#1052 = CARTESIAN_POINT ( 'NONE',  ( 17.52187500061451431, 3.027376345333613106, -5.243569643749998122 ) ) ;
#1053 = CARTESIAN_POINT ( 'NONE',  ( 19.16250000122903430, 4.330127018922192761, -2.499999999999997780 ) ) ;
#1054 = CARTESIAN_POINT ( 'NONE',  ( 14.97187500061451892, 3.027376345333611329, 5.243569643749999010 ) ) ;
#1055 = EDGE_CURVE ( 'NONE', #42390, #54979, #24487, .T. ) ;
#1056 = CARTESIAN_POINT ( 'NONE',  ( -2.121784821874999949, 10.33437500061451786, 26.32496088578401938 ) ) ;
#1057 = CARTESIAN_POINT ( 'NONE',  ( 19.27500000122903145, 2.886751345948126879, 4.999999999999999112 ) ) ;
#1058 = CARTESIAN_POINT ( 'NONE',  ( 15.51562500061451644, -6.054752690667223547, -1.112240025338166033E-15 ) ) ;
#1059 = CARTESIAN_POINT ( 'NONE',  ( 25.46249999999999503, 2.886751345948143754, 4.999999999999969802 ) ) ;
#1060 = ORIENTED_EDGE ( 'NONE', *, *, #43888, .F. ) ;
#1061 = ORIENTED_EDGE ( 'NONE', *, *, #53191, .F. ) ;
#1062 = CARTESIAN_POINT ( 'NONE',  ( 19.12500000000000000, 4.330127018922191873, 2.499999999999999556 ) ) ;
#1063 = CARTESIAN_POINT ( 'NONE',  ( 10.00000000000000000, 1.224646799147353256E-15, -10.00000000000000888 ) ) ;
#1064 = CARTESIAN_POINT ( 'NONE',  ( 3.815625000614518036, -6.054752690667223547, -1.112240025338166033E-15 ) ) ;
#1065 = CARTESIAN_POINT ( 'NONE',  ( 15.67500000122903181, 2.886751345948126879, 4.999999999999999112 ) ) ;
#1066 = CARTESIAN_POINT ( 'NONE',  ( 27.00937500061451857, 4.541064518000418104, -2.621784821874998173 ) ) ;
#1067 = EDGE_CURVE ( 'NONE', #56470, #45665, #34410, .T. ) ;
#1068 = CARTESIAN_POINT ( 'NONE',  ( 21.17812500061451431, 4.541064518000418104, 2.621784821874999949 ) ) ;
#1069 = CARTESIAN_POINT ( 'NONE',  ( 22.26562500061451644, -6.054752690667223547, -1.112240025338166033E-15 ) ) ;
#1070 = CARTESIAN_POINT ( 'NONE',  ( 3.703125000614516882, 0.000000000000000000, 5.243569643749999010 ) ) ;
#1071 = EDGE_CURVE ( 'NONE', #53683, #17652, #44373, .T. ) ;
#1072 = CARTESIAN_POINT ( 'NONE',  ( 26.92499999999999716, -4.330127018922194537, 2.499999999999995559 ) ) ;
#1073 = CARTESIAN_POINT ( 'NONE',  ( 4.596237264682155654, 1.968401129533140059, 4.860084320473172070 ) ) ;
#1074 = CARTESIAN_POINT ( 'NONE',  ( 8.709375000614517859, 0.000000000000000000, 4.756430356249998326 ) ) ;
#1075 = DIRECTION ( 'NONE',  ( 0.000000000000000000, 0.000000000000000000, 1.000000000000000000 ) ) ;
#1076 = CARTESIAN_POINT ( 'NONE',  ( -3.999999999999999556, 11.52500000122903501, -32.30940107675850470 ) ) ;
#1077 = CARTESIAN_POINT ( 'NONE',  ( -4.243569643749999898, 14.90937500061451715, -30.00000000000000000 ) ) ;
#1078 = CARTESIAN_POINT ( 'NONE',  ( 5.325000001229033941, 2.886751345948126879, 4.999999999999999112 ) ) ;
#1079 = CARTESIAN_POINT ( 'NONE',  ( 5.475000000000000533, 6.123233995736764310E-16, -4.999999999999998224 ) ) ;
#1080 = ADVANCED_FACE ( 'NONE', ( #48229 ), #31963, .F. ) ;
#1081 = CARTESIAN_POINT ( 'NONE',  ( 3.975000001229033852, 2.886751345948126879, 4.999999999999999112 ) ) ;
#1082 = CARTESIAN_POINT ( 'NONE',  ( 10.13437500061451679, -4.541064518000419881, 2.621784821874995952 ) ) ;
#1083 = CARTESIAN_POINT ( 'NONE',  ( 23.98125000122903216, 6.123233995736764310E-16, -4.999999999999998224 ) ) ;
#1084 = CARTESIAN_POINT ( 'NONE',  ( 4.898587196589411843E-16, 20.00000000000000000, -26.00000000000000000 ) ) ;
#1085 = CARTESIAN_POINT ( 'NONE',  ( -4.872631645816652757, 8.733424155075976358, -33.50632029722230953 ) ) ;
#1086 = CARTESIAN_POINT ( 'NONE',  ( 16.95000000122903572, 5.773502691896255534, 3.535250795749688401E-16 ) ) ;
#1087 = CARTESIAN_POINT ( 'NONE',  ( 7.621875000614519280, 3.027376345333613106, -5.243569643749998122 ) ) ;
#1088 = CARTESIAN_POINT ( 'NONE',  ( 12.49687500061451573, -3.027376345333610441, -5.243569643749999898 ) ) ;
#1089 = CARTESIAN_POINT ( 'NONE',  ( 5.700000000000000178, 0.000000000000000000, 4.999999999999998224 ) ) ;
#1090 = CARTESIAN_POINT ( 'NONE',  ( -2.121784821874999949, 16.12812500061459176, 26.32496088578401938 ) ) ;
#1091 = CARTESIAN_POINT ( 'NONE',  ( 21.72187500061451715, 3.027376345333611329, 5.243569643749999010 ) ) ;
#1092 = DIRECTION ( 'NONE',  ( -0.000000000000000000, -1.000000000000000000, -0.000000000000000000 ) ) ;
#1093 = CARTESIAN_POINT ( 'NONE',  ( 25.76250000122903216, -4.330127018922190985, -2.500000000000001332 ) ) ;
#1094 = CARTESIAN_POINT ( 'NONE',  ( 16.77187500061451431, -4.119189519843968306, 2.378215178124996054 ) ) ;
#1095 = CARTESIAN_POINT ( 'NONE',  ( 23.12812500061451360, -4.541064518000419881, 2.621784821874995952 ) ) ;
#1096 = CARTESIAN_POINT ( 'NONE',  ( 13.45312500061451466, 4.541064518000418104, -2.621784821874998173 ) ) ;
#1097 = CARTESIAN_POINT ( 'NONE',  ( 27.27187500061451786, 5.824947211148865298E-16, -4.756430356249998326 ) ) ;
#1098 = CARTESIAN_POINT ( 'NONE',  ( 11.78437500061451892, 4.541064518000418104, 2.621784821874999949 ) ) ;
#1099 = CARTESIAN_POINT ( 'NONE',  ( 27.93750000000000000, -2.886751345948125991, -5.000000000000000000 ) ) ;
#1100 = CARTESIAN_POINT ( 'NONE',  ( 21.60000000122903430, -2.886751345948129988, 4.999999999999997335 ) ) ;
#1101 = DIRECTION ( 'NONE',  ( -1.000000000000000000, -0.000000000000000000, -0.000000000000000000 ) ) ;
#1102 = CARTESIAN_POINT ( 'NONE',  ( 12.72187500061451537, 3.027376345333611329, 5.243569643749999010 ) ) ;
#1103 = CARTESIAN_POINT ( 'NONE',  ( 27.87187500061451573, 3.027376345333613106, -5.243569643749998122 ) ) ;
#1104 = CARTESIAN_POINT ( 'NONE',  ( 28.25625000122903074, 0.000000000000000000, 4.999999999999998224 ) ) ;
#1105 = CARTESIAN_POINT ( 'NONE',  ( 45.00000000000000000, 0.000000000000000000, 0.000000000000000000 ) ) ;
#1106 = CARTESIAN_POINT ( 'NONE',  ( 21.72187500061451715, 3.027376345333611329, 5.243569643749999010 ) ) ;
#1107 = CARTESIAN_POINT ( 'NONE',  ( 15.15937500061451715, -4.541064518000417216, -2.621784821875001281 ) ) ;
#1108 = CARTESIAN_POINT ( 'NONE',  ( -3.756430356250001434, 18.41562499938548214, 32.16877607737301048 ) ) ;
#1109 = CARTESIAN_POINT ( 'NONE',  ( 26.43750000000000000, -2.886751345948129988, 4.999999999999997335 ) ) ;
#1110 = CARTESIAN_POINT ( 'NONE',  ( 4.000000000000000000, 13.43750000000000000, 27.69059892324149530 ) ) ;
#1111 = CARTESIAN_POINT ( 'NONE',  ( 27.60937500061451644, 0.000000000000000000, 4.756430356249998326 ) ) ;
#1112 = CARTESIAN_POINT ( 'NONE',  ( 17.35312500061451502, -4.541064518000417216, -2.621784821875001281 ) ) ;
#1113 = CARTESIAN_POINT ( 'NONE',  ( 7.162500000000001421, -5.773502691896255534, -1.060575238724906372E-15 ) ) ;
#1114 = CARTESIAN_POINT ( 'NONE',  ( 1.071796769724489895, 13.67990381179670045, 26.00000000000000355 ) ) ;
#1115 = CARTESIAN_POINT ( 'NONE',  ( 15.75000000000000000, -4.330127018922190985, -2.500000000000001332 ) ) ;
#1116 = CARTESIAN_POINT ( 'NONE',  ( 2.121784821875001281, 10.50312500061451715, 33.67503911421598417 ) ) ;
#1117 = CARTESIAN_POINT ( 'NONE',  ( 26.03437500061451715, 6.421520780324663323E-16, -5.243569643749999010 ) ) ;
#1118 = ORIENTED_EDGE ( 'NONE', *, *, #30725, .F. ) ;
#1119 = CARTESIAN_POINT ( 'NONE',  ( 21.74062500061451431, -3.027376345333614438, 5.243569643749998122 ) ) ;
#1120 = CARTESIAN_POINT ( 'NONE',  ( 19.69687500061451857, -3.027376345333610441, -5.243569643749999898 ) ) ;
#1121 = CARTESIAN_POINT ( 'NONE',  ( 5.287500000000000533, -2.886751345948129988, 4.999999999999997335 ) ) ;
#1122 = CARTESIAN_POINT ( 'NONE',  ( 6.215625000614517504, 3.027376345333613106, -5.243569643749998122 ) ) ;
#1123 = CARTESIAN_POINT ( 'NONE',  ( 21.17812500061451431, 4.541064518000418104, 2.621784821874999949 ) ) ;
#1124 = CARTESIAN_POINT ( 'NONE',  ( 12.53437500061451537, 6.421520780324663323E-16, -5.243569643749999010 ) ) ;
#1125 = CARTESIAN_POINT ( 'NONE',  ( 16.47187500061452070, -6.054752690667223547, -1.112240025338166033E-15 ) ) ;
#1126 = CARTESIAN_POINT ( 'NONE',  ( 9.001249775931846008E-16, 16.76562500061451999, 34.90005215228797653 ) ) ;
#1127 = CARTESIAN_POINT ( 'NONE',  ( 19.50000000122903288, -2.886751345948125991, -5.000000000000000000 ) ) ;
#1128 = CARTESIAN_POINT ( 'NONE',  ( 15.42187500061451821, 2.746126346562643317, 4.756430356249998326 ) ) ;
#1129 = CARTESIAN_POINT ( 'NONE',  ( 8.803125000614517859, -4.541064518000417216, -2.621784821875001281 ) ) ;
#1130 = CARTESIAN_POINT ( 'NONE',  ( 4.696875000614518569, -3.027376345333614438, 5.243569643749998122 ) ) ;
#1131 = CARTESIAN_POINT ( 'NONE',  ( 5.971875000614516260, 3.027376345333611329, 5.243569643749999010 ) ) ;
#1132 = CARTESIAN_POINT ( 'NONE',  ( 26.25937500061451857, 0.000000000000000000, 5.243569643749999010 ) ) ;
#1133 = CARTESIAN_POINT ( 'NONE',  ( 15.77812500061451573, 4.541064518000418104, 2.621784821874999949 ) ) ;
#1134 = CARTESIAN_POINT ( 'NONE',  ( 26.28750000122903430, 6.123233995736764310E-16, -4.999999999999998224 ) ) ;
#1135 = CARTESIAN_POINT ( 'NONE',  ( 25.75312500061451715, 0.000000000000000000, 5.243569643749999010 ) ) ;
#1136 = CARTESIAN_POINT ( 'NONE',  ( 21.83437500061451786, -4.541064518000419881, 2.621784821874995952 ) ) ;
#1137 = CARTESIAN_POINT ( 'NONE',  ( 18.06562500061451715, 3.027376345333611329, 5.243569643749999010 ) ) ;
#1138 = CARTESIAN_POINT ( 'NONE',  ( -4.243569643749997233, 16.29687500061451644, 32.45002607614398471 ) ) ;
#1139 = CARTESIAN_POINT ( 'NONE',  ( 21.62812500061451360, 4.541064518000418104, 2.621784821874999949 ) ) ;
#1140 = CARTESIAN_POINT ( 'NONE',  ( 3.112500001229034918, 0.000000000000000000, 4.999999999999998224 ) ) ;
#1141 = ORIENTED_EDGE ( 'NONE', *, *, #28856, .F. ) ;
#1142 = CARTESIAN_POINT ( 'NONE',  ( 25.57499999999999929, -4.330127018922194537, 2.499999999999995559 ) ) ;
#1143 = CARTESIAN_POINT ( 'NONE',  ( 3.999999999999998668, 13.06250000000000355, -32.30940107675850470 ) ) ;
#1144 = CARTESIAN_POINT ( 'NONE',  ( 1.999999999999998668, 18.16250000122903074, 26.53589838486224650 ) ) ;
#1145 = EDGE_CURVE ( 'NONE', #65176, #58120, #30504, .T. ) ;
#1146 = EDGE_CURVE ( 'NONE', #35743, #36091, #69393, .T. ) ;
#1147 = CARTESIAN_POINT ( 'NONE',  ( 2.971875000614517592, -6.054752690667223547, -1.112240025338166033E-15 ) ) ;
#1148 = CARTESIAN_POINT ( 'NONE',  ( 9.028125000614517504, 4.541064518000418104, 2.621784821874999949 ) ) ;
#1149 = CARTESIAN_POINT ( 'NONE',  ( 23.40000000122903145, -2.886751345948129988, 4.999999999999997335 ) ) ;
#1150 = CARTESIAN_POINT ( 'NONE',  ( 28.11562500061451431, -6.054752690667223547, -1.112240025338166033E-15 ) ) ;
#1151 = CARTESIAN_POINT ( 'NONE',  ( 27.78749999999999787, -2.886751345948129988, 4.999999999999997335 ) ) ;
#1152 = CARTESIAN_POINT ( 'NONE',  ( -3.999999999999999556, 16.02500000122903501, -32.30940107675850470 ) ) ;
#1153 = CARTESIAN_POINT ( 'NONE',  ( 29.76562500061451644, 3.027376345333611329, 5.243569643749999010 ) ) ;
#1154 = CARTESIAN_POINT ( 'NONE',  ( 10.30312500061451431, 4.541064518000418104, -2.621784821874998173 ) ) ;
#1155 = EDGE_LOOP ( 'NONE', ( #2010, #4569, #25849, #38019 ) ) ;
#1156 = CARTESIAN_POINT ( 'NONE',  ( 25.90312500061451573, -4.541064518000417216, -2.621784821875001281 ) ) ;
#1157 = CARTESIAN_POINT ( 'NONE',  ( 8.090625000614515727, 6.054752690667223547, 3.707466751127219781E-16 ) ) ;
#1158 = CARTESIAN_POINT ( 'NONE',  ( 5.390625000614518214, 6.054752690667223547, 3.707466751127219781E-16 ) ) ;
#1159 = CARTESIAN_POINT ( 'NONE',  ( 17.48437500061451999, 5.824947211148865298E-16, -4.756430356249998326 ) ) ;
#1160 = DIRECTION ( 'NONE',  ( 0.000000000000000000, 0.000000000000000000, 1.000000000000000000 ) ) ;
#1161 = CARTESIAN_POINT ( 'NONE',  ( 16.68750000000000000, -2.886751345948125991, -5.000000000000000000 ) ) ;
#1162 = CARTESIAN_POINT ( 'NONE',  ( 15.12187500061451750, -6.054752690667223547, -1.112240025338166033E-15 ) ) ;
#1163 = CARTESIAN_POINT ( 'NONE',  ( 11.06250000122903288, 4.330127018922192761, -2.499999999999997780 ) ) ;
#1164 = CARTESIAN_POINT ( 'NONE',  ( 16.09687500061452070, -3.027376345333610441, -5.243569643749999898 ) ) ;
#1165 = CARTESIAN_POINT ( 'NONE',  ( 17.02499999999999858, -4.330127018922194537, 2.499999999999995559 ) ) ;
#1166 = CARTESIAN_POINT ( 'NONE',  ( 20.70937500061451786, 4.541064518000418104, -2.621784821874998173 ) ) ;
#1167 = CARTESIAN_POINT ( 'NONE',  ( 2.121784821875001281, 14.55312500061451786, -26.32496088578401938 ) ) ;
#1168 = DIRECTION ( 'NONE',  ( -1.000000000000000000, -0.000000000000000000, -0.000000000000000000 ) ) ;
#1169 = CARTESIAN_POINT ( 'NONE',  ( 24.08437500061451786, -2.746126346562641984, -4.756430356249999214 ) ) ;
#1170 = CARTESIAN_POINT ( 'NONE',  ( 4.121605622237005662, 2.830625451251030711, 4.413915781326256393 ) ) ;
#1171 = CARTESIAN_POINT ( 'NONE',  ( 24.96562500061451573, -6.054752690667223547, -1.112240025338166033E-15 ) ) ;
#1172 = DIRECTION ( 'NONE',  ( 0.000000000000000000, -0.000000000000000000, -1.000000000000000000 ) ) ;
#1173 = CARTESIAN_POINT ( 'NONE',  ( 28.09687500061451360, -3.027376345333614438, 5.243569643749998122 ) ) ;
#1174 = CARTESIAN_POINT ( 'NONE',  ( 24.82499999999999929, 6.123233995736764310E-16, -4.999999999999998224 ) ) ;
#1175 = CARTESIAN_POINT ( 'NONE',  ( 5.878125000614517148, 4.541064518000418104, 2.621784821874999949 ) ) ;
#1176 = CARTESIAN_POINT ( 'NONE',  ( 25.77187500061451431, -4.119189519843968306, 2.378215178124996054 ) ) ;
#1177 = CARTESIAN_POINT ( 'NONE',  ( 18.94687500061451502, 6.054752690667223547, 3.707466751127219781E-16 ) ) ;
#1178 = CARTESIAN_POINT ( 'NONE',  ( 11.40937500061451537, -5.492252693125287522, -1.008910452111647106E-15 ) ) ;
#1179 = CARTESIAN_POINT ( 'NONE',  ( 5.728125000614515905, 6.421520780324663323E-16, -5.243569643749999010 ) ) ;
#1180 = CARTESIAN_POINT ( 'NONE',  ( 8.296875000614516438, -3.027376345333614438, 5.243569643749998122 ) ) ;
#1181 = ORIENTED_EDGE ( 'NONE', *, *, #52747, .F. ) ;
#1182 = CARTESIAN_POINT ( 'NONE',  ( 19.39687500061451786, 6.054752690667223547, 3.707466751127219781E-16 ) ) ;
#1183 = CARTESIAN_POINT ( 'NONE',  ( -4.000000000000000888, 15.85624999877096641, 32.30940107675850470 ) ) ;
#1184 = CARTESIAN_POINT ( 'NONE',  ( 27.22499999999999787, 4.330127018922191873, 2.499999999999999556 ) ) ;
#1185 = CARTESIAN_POINT ( 'NONE',  ( 29.74687500061451217, 6.054752690667223547, 3.707466751127219781E-16 ) ) ;
#1186 = CARTESIAN_POINT ( 'NONE',  ( 19.31250000000000000, -5.773502691896255534, -1.060575238724906372E-15 ) ) ;
#1187 = FACE_OUTER_BOUND ( 'NONE', #70804, .T. ) ;
#1188 = ORIENTED_EDGE ( 'NONE', *, *, #50906, .T. ) ;
#1189 = CARTESIAN_POINT ( 'NONE',  ( 10.68750000000000000, -2.886751345948129988, 4.999999999999997335 ) ) ;
#1190 = CARTESIAN_POINT ( 'NONE',  ( 10.88437500061451679, -2.746126346562646425, 4.756430356249996549 ) ) ;
#1191 = CARTESIAN_POINT ( 'NONE',  ( 24.85312500061451502, 0.000000000000000000, 5.243569643749999010 ) ) ;
#1192 = CARTESIAN_POINT ( 'NONE',  ( 13.38750000000000107, -2.886751345948129988, 4.999999999999997335 ) ) ;
#1193 = CARTESIAN_POINT ( 'NONE',  ( 9.937500001229032875, -4.330127018922194537, 2.499999999999995559 ) ) ;
#1194 = CARTESIAN_POINT ( 'NONE',  ( 8.615625000614517859, 3.027376345333611329, 5.243569643749999010 ) ) ;
#1195 =( BOUNDED_CURVE ( )  B_SPLINE_CURVE ( 2, ( #11522, #40690, #45148, #17414, #39971, #63208, #11162 ),
 .UNSPECIFIED., .F., .F. ) 
 B_SPLINE_CURVE_WITH_KNOTS ( ( 3, 2, 2, 3 ),
 ( 0.4583333333333332593, 0.4611111111111111382, 0.4638888888888889062, 0.4666666666666667296 ),
 .UNSPECIFIED. ) 
 CURVE ( )  GEOMETRIC_REPRESENTATION_ITEM ( )  RATIONAL_B_SPLINE_CURVE ( ( 1.000000000000002665, 0.8660254037844360431, 1.000000000000000000, 0.8660254037844387076, 1.000000000000000000, 0.8660254037844360431, 1.000000000000002665 ) ) 
 REPRESENTATION_ITEM ( '' )  );
#1196 = CARTESIAN_POINT ( 'NONE',  ( 22.53750000000000142, -2.886751345948125991, -5.000000000000000000 ) ) ;
#1197 = EDGE_CURVE ( 'NONE', #48448, #47360, #14965, .T. ) ;
#1198 = CARTESIAN_POINT ( 'NONE',  ( 21.77812500061451928, -4.541064518000419881, 2.621784821874995952 ) ) ;
#1199 = DIRECTION ( 'NONE',  ( 0.000000000000000000, 0.000000000000000000, 1.000000000000000000 ) ) ;
#1200 = CARTESIAN_POINT ( 'NONE',  ( 26.43750000122903288, 4.330127018922191873, 2.499999999999999556 ) ) ;
#1201 = CARTESIAN_POINT ( 'NONE',  ( -3.756430356250000102, 17.36562499938548498, 30.00000000000000000 ) ) ;
#1202 = CARTESIAN_POINT ( 'NONE',  ( 8.474999999999999645, -4.330127018922194537, 2.499999999999995559 ) ) ;
#1203 = ORIENTED_EDGE ( 'NONE', *, *, #11547, .T. ) ;
#1204 = CARTESIAN_POINT ( 'NONE',  ( 22.52812500061451573, 4.541064518000418104, 2.621784821874999949 ) ) ;
#1205 = DIRECTION ( 'NONE',  ( 0.000000000000000000, 0.000000000000000000, 1.000000000000000000 ) ) ;
#1206 = CARTESIAN_POINT ( 'NONE',  ( 26.48437500061451644, 6.421520780324663323E-16, -5.243569643749999010 ) ) ;
#1207 = CARTESIAN_POINT ( 'NONE',  ( 18.04687500061451999, 6.054752690667223547, 3.707466751127219781E-16 ) ) ;
#1208 = CARTESIAN_POINT ( 'NONE',  ( 13.90312500061451750, 4.541064518000418104, -2.621784821874998173 ) ) ;
#1209 = CARTESIAN_POINT ( 'NONE',  ( 9.001249775931846008E-16, 10.01562500061459282, -25.09994784771203058 ) ) ;
#1210 = CARTESIAN_POINT ( 'NONE',  ( 25.68750000122903288, -4.330127018922194537, 2.499999999999995559 ) ) ;
#1211 = CARTESIAN_POINT ( 'NONE',  ( 22.62187500061451573, 2.746126346562643317, 4.756430356249998326 ) ) ;
#1212 = CARTESIAN_POINT ( 'NONE',  ( 15.74062500061451608, 6.054752690667223547, 3.707466751127219781E-16 ) ) ;
#1213 = FACE_OUTER_BOUND ( 'NONE', #2994, .T. ) ;
#1214 = CARTESIAN_POINT ( 'NONE',  ( 3.975000001229033852, 2.886751345948126879, 4.999999999999999112 ) ) ;
#1215 = CARTESIAN_POINT ( 'NONE',  ( 11.78437500061451892, 4.541064518000418104, 2.621784821874999949 ) ) ;
#1216 = CARTESIAN_POINT ( 'NONE',  ( 11.85937500061451644, 0.000000000000000000, 5.243569643749999010 ) ) ;
#1217 = CARTESIAN_POINT ( 'NONE',  ( 19.02187500061451786, 3.027376345333611329, 5.243569643749999010 ) ) ;
#1218 = ORIENTED_EDGE ( 'NONE', *, *, #63369, .F. ) ;
#1219 = CARTESIAN_POINT ( 'NONE',  ( 29.32499999999999929, 6.123233995736764310E-16, -4.999999999999998224 ) ) ;
#1220 = CARTESIAN_POINT ( 'NONE',  ( 23.65312500061451573, -4.541064518000417216, -2.621784821875001281 ) ) ;
#1221 = CARTESIAN_POINT ( 'NONE',  ( 20.10937500061451289, -4.541064518000417216, -2.621784821875001281 ) ) ;
#1222 = CARTESIAN_POINT ( 'NONE',  ( 25.52812500061451573, 6.421520780324663323E-16, -5.243569643749999010 ) ) ;
#1223 = CARTESIAN_POINT ( 'NONE',  ( -3.999999999999999112, 17.13124999877096499, 27.69059892324149530 ) ) ;
#1224 = CARTESIAN_POINT ( 'NONE',  ( 4.000000000000000000, 13.88750000000000107, 32.30940107675849049 ) ) ;
#1225 = CARTESIAN_POINT ( 'NONE',  ( 29.05312500061451431, -4.541064518000417216, -2.621784821875001281 ) ) ;
#1226 = CARTESIAN_POINT ( 'NONE',  ( 9.712500001229033231, 4.330127018922192761, -2.499999999999997780 ) ) ;
#1227 = CARTESIAN_POINT ( 'NONE',  ( 8.062500001229034652, 0.000000000000000000, 4.999999999999998224 ) ) ;
#1228 = CARTESIAN_POINT ( 'NONE',  ( 28.61250000000000071, 2.886751345948148195, 4.999999999999962697 ) ) ;
#1229 = CARTESIAN_POINT ( 'NONE',  ( 26.51250000122903216, 0.000000000000000000, 4.999999999999998224 ) ) ;
#1230 = CARTESIAN_POINT ( 'NONE',  ( 2.655984681222220721E-16, 12.86562499938548321, 25.66244784525396483 ) ) ;
#1231 = CARTESIAN_POINT ( 'NONE',  ( 17.41875000122903216, 2.886751345948126879, 4.999999999999999112 ) ) ;
#1232 = EDGE_CURVE ( 'NONE', #6226, #3193, #4249, .T. ) ;
#1233 = CARTESIAN_POINT ( 'NONE',  ( 8.484375000614518214, 6.421520780324663323E-16, -5.243569643749999010 ) ) ;
#1234 = CARTESIAN_POINT ( 'NONE',  ( 2.000000000000001332, 9.912500001229034297, 33.46410161513774995 ) ) ;
#1235 = CARTESIAN_POINT ( 'NONE',  ( 18.14062500061451644, -3.027376345333614438, 5.243569643749998122 ) ) ;
#1236 = CARTESIAN_POINT ( 'NONE',  ( 10.28437500061451715, 6.421520780324663323E-16, -5.243569643749999010 ) ) ;
#1237 = CARTESIAN_POINT ( 'NONE',  ( 28.31250000122903288, 0.000000000000000000, 4.999999999999998224 ) ) ;
#1238 = CARTESIAN_POINT ( 'NONE',  ( 19.95937500061451786, 0.000000000000000000, 5.243569643749999010 ) ) ;
#1239 = CARTESIAN_POINT ( 'NONE',  ( 8.221875000614518925, 3.027376345333611329, 5.243569643749999010 ) ) ;
#1240 = CARTESIAN_POINT ( 'NONE',  ( 3.103125000614517237, 4.541064518000418104, -2.621784821874998173 ) ) ;
#1241 = CARTESIAN_POINT ( 'NONE',  ( -1.243387493232115393E-14, 16.21250000000000213, 26.00000000000000000 ) ) ;
#1242 = CARTESIAN_POINT ( 'NONE',  ( 7.040625000614517681, -3.027376345333610441, -5.243569643749999898 ) ) ;
#1243 = CARTESIAN_POINT ( 'NONE',  ( 18.66562500061451146, -6.054752690667223547, -1.112240025338166033E-15 ) ) ;
#1244 = ORIENTED_EDGE ( 'NONE', *, *, #41134, .F. ) ;
#1245 = CARTESIAN_POINT ( 'NONE',  ( 5.212500001229032343, 4.330127018922192761, -2.499999999999997780 ) ) ;
#1246 = CARTESIAN_POINT ( 'NONE',  ( 14.09062500061451750, -3.027376345333614438, 5.243569643749998122 ) ) ;
#1247 = CARTESIAN_POINT ( 'NONE',  ( 13.90312500061451750, 4.541064518000418104, -2.621784821874998173 ) ) ;
#1248 = CARTESIAN_POINT ( 'NONE',  ( 23.48437500061451644, 4.119189519843966529, 2.378215178124999607 ) ) ;
#1249 = CARTESIAN_POINT ( 'NONE',  ( 12.44999999999999929, 0.000000000000000000, 4.999999999999998224 ) ) ;
#1250 = CARTESIAN_POINT ( 'NONE',  ( 10.05000000122903181, -2.886751345948125991, -5.000000000000000000 ) ) ;
#1251 = EDGE_CURVE ( 'NONE', #65794, #57266, #26423, .T. ) ;
#1252 = CARTESIAN_POINT ( 'NONE',  ( 6.103125000614515905, -4.541064518000417216, -2.621784821875001281 ) ) ;
#1253 = CARTESIAN_POINT ( 'NONE',  ( 19.38750000122903216, -4.330127018922194537, 2.499999999999995559 ) ) ;
#1254 = CARTESIAN_POINT ( 'NONE',  ( 25.08749999999999858, -2.886751345948129988, 4.999999999999997335 ) ) ;
#1255 = CARTESIAN_POINT ( 'NONE',  ( 4.243569643749999010, 11.12187500061451928, -32.45002607614398471 ) ) ;
#1256 = CARTESIAN_POINT ( 'NONE',  ( 4.087500001229035007, -4.330127018922194537, 2.499999999999995559 ) ) ;
#1257 = CARTESIAN_POINT ( 'NONE',  ( 28.35000000122903430, -2.886751345948114000, 5.000000000000024869 ) ) ;
#1258 = CARTESIAN_POINT ( 'NONE',  ( 24.41250000000000142, 2.886751345948142866, -4.999999999999973355 ) ) ;
#1259 = CARTESIAN_POINT ( 'NONE',  ( 18.30937500061451928, -4.541064518000417216, -2.621784821875001281 ) ) ;
#1260 = CARTESIAN_POINT ( 'NONE',  ( -5.000000000000000000, 39.99999999999999289, 45.00000000000000000 ) ) ;
#1261 = CARTESIAN_POINT ( 'NONE',  ( 14.57812500061451644, -4.541064518000419881, 2.621784821874995952 ) ) ;
#1262 = CARTESIAN_POINT ( 'NONE',  ( 8.493750001229033231, -2.886751345948129988, 4.999999999999997335 ) ) ;
#1263 = CARTESIAN_POINT ( 'NONE',  ( 4.898587196589411843E-16, 20.00000000000000000, -26.00000000000000000 ) ) ;
#1264 = CARTESIAN_POINT ( 'NONE',  ( 26.25937500061451857, 0.000000000000000000, 5.243569643749999010 ) ) ;
#1265 = CARTESIAN_POINT ( 'NONE',  ( 17.74687500061451928, -4.119189519843965641, -2.378215178125001383 ) ) ;
#1266 = CARTESIAN_POINT ( 'NONE',  ( 11.99062500061451608, -3.027376345333610441, -5.243569643749999898 ) ) ;
#1267 = CARTESIAN_POINT ( 'NONE',  ( 16.47187500061452070, -6.054752690667223547, -1.112240025338166033E-15 ) ) ;
#1268 = ORIENTED_EDGE ( 'NONE', *, *, #50356, .T. ) ;
#1269 = CARTESIAN_POINT ( 'NONE',  ( 27.92812500061451431, 4.541064518000418104, 2.621784821874999949 ) ) ;
#1270 = CARTESIAN_POINT ( 'NONE',  ( 19.82812500061451644, 4.541064518000418104, 2.621784821874999949 ) ) ;
#1271 = CARTESIAN_POINT ( 'NONE',  ( 3.144856541311010556, 3.887142566792906706, -3.519253510942787599 ) ) ;
#1272 = CARTESIAN_POINT ( 'NONE',  ( 9.600000000000001421, 4.330127018922192761, -2.499999999999997780 ) ) ;
#1273 = CARTESIAN_POINT ( 'NONE',  ( 18.37500000122903288, 2.886751345948126879, 4.999999999999999112 ) ) ;
#1274 = CARTESIAN_POINT ( 'NONE',  ( 16.55625000122903145, 0.000000000000000000, 4.999999999999998224 ) ) ;
#1275 = CARTESIAN_POINT ( 'NONE',  ( 11.03437500061451360, -2.746126346562642428, -4.756430356249999214 ) ) ;
#1276 = ORIENTED_EDGE ( 'NONE', *, *, #52094, .T. ) ;
#1277 = CARTESIAN_POINT ( 'NONE',  ( 17.88749999999999929, -2.886751345948129988, 4.999999999999997335 ) ) ;
#1278 = CARTESIAN_POINT ( 'NONE',  ( 20.32499999999999929, 6.123233995736764310E-16, -4.999999999999998224 ) ) ;
#1279 = CARTESIAN_POINT ( 'NONE',  ( 20.07187500061451857, -6.054752690667223547, -1.112240025338166033E-15 ) ) ;
#1280 = CARTESIAN_POINT ( 'NONE',  ( 24.70312500061451644, 4.541064518000418104, -2.621784821874998173 ) ) ;
#1281 = ORIENTED_EDGE ( 'NONE', *, *, #64328, .F. ) ;
#1282 = CARTESIAN_POINT ( 'NONE',  ( 5.810221930991193690E-16, 19.36250000000000071, 26.00000000000000000 ) ) ;
#1283 = CARTESIAN_POINT ( 'NONE',  ( 9.103125000614515017, 0.000000000000000000, 5.243569643749999010 ) ) ;
#1284 = CARTESIAN_POINT ( 'NONE',  ( 0.000000000000000000, 20.00000000000000000, 26.00000000000000000 ) ) ;
#1285 = CARTESIAN_POINT ( 'NONE',  ( 15.71250000000000213, -5.773502691896255534, -1.060575238724906372E-15 ) ) ;
#1286 = CARTESIAN_POINT ( 'NONE',  ( -4.243569643749997233, 16.69062500061451360, 32.45002607614398471 ) ) ;
#1287 = CARTESIAN_POINT ( 'NONE',  ( 29.72812500061451502, 4.541064518000418104, 2.621784821874999949 ) ) ;
#1288 = CARTESIAN_POINT ( 'NONE',  ( 9.637499999999999289, 5.773502691896255534, 3.535250795749688894E-16 ) ) ;
#1289 = CARTESIAN_POINT ( 'NONE',  ( 3.756430356249998770, 16.20312499938548356, 32.16877607737302469 ) ) ;
#1290 = CARTESIAN_POINT ( 'NONE',  ( 26.07187500061451857, 3.027376345333613106, -5.243569643749998122 ) ) ;
#1291 = ORIENTED_EDGE ( 'NONE', *, *, #3876, .F. ) ;
#1292 = CARTESIAN_POINT ( 'NONE',  ( 22.34062500061451573, -3.027376345333610441, -5.243569643749999898 ) ) ;
#1293 = CARTESIAN_POINT ( 'NONE',  ( 23.14687500061451786, -3.027376345333614438, 5.243569643749998122 ) ) ;
#1294 = CARTESIAN_POINT ( 'NONE',  ( 4.243569643749999898, 16.87812500061459176, -30.00000000000000000 ) ) ;
#1295 = CARTESIAN_POINT ( 'NONE',  ( 10.42500000000000071, 6.123233995736764310E-16, -4.999999999999998224 ) ) ;
#1296 = CARTESIAN_POINT ( 'NONE',  ( 5.915625000614515905, 3.027376345333611329, 5.243569643749999010 ) ) ;
#1297 = CARTESIAN_POINT ( 'NONE',  ( 29.55937500061451573, -4.119189519843965641, -2.378215178125001383 ) ) ;
#1298 = CARTESIAN_POINT ( 'NONE',  ( 23.16562500061451502, -6.054752690667223547, -1.112240025338166033E-15 ) ) ;
#1299 = CARTESIAN_POINT ( 'NONE',  ( 28.65937500061451715, 2.746126346562645981, -4.756430356249997438 ) ) ;
#1300 = CARTESIAN_POINT ( 'NONE',  ( 13.69687500061451679, -2.746126346562646425, 4.756430356249996549 ) ) ;
#1301 = CARTESIAN_POINT ( 'NONE',  ( 16.65937500061452070, 4.541064518000418104, -2.621784821874998173 ) ) ;
#1302 = CARTESIAN_POINT ( 'NONE',  ( 2.121784821874999061, 12.50937500061451857, 26.32496088578401583 ) ) ;
#1303 = ADVANCED_FACE ( 'NONE', ( #64107 ), #16504, .T. ) ;
#1304 = CARTESIAN_POINT ( 'NONE',  ( 20.14687500061451786, -3.027376345333610441, -5.243569643749999898 ) ) ;
#1305 = CARTESIAN_POINT ( 'NONE',  ( 26.44687500061451502, -3.027376345333610441, -5.243569643749999898 ) ) ;
#1306 = CARTESIAN_POINT ( 'NONE',  ( 2.121784821875001281, 15.95937500061451608, 33.67503911421598417 ) ) ;
#1307 = CARTESIAN_POINT ( 'NONE',  ( 7.078125000614516438, 6.421520780324663323E-16, -5.243569643749999010 ) ) ;
#1308 = DIRECTION ( 'NONE',  ( -1.000000000000000000, -0.000000000000000000, -0.000000000000000000 ) ) ;
#1309 = CARTESIAN_POINT ( 'NONE',  ( 4.959375000614516971, 4.541064518000418104, -2.621784821874998173 ) ) ;
#1310 = CARTESIAN_POINT ( 'NONE',  ( 25.95000000122903216, 5.773502691896255534, 3.535250795749688401E-16 ) ) ;
#1311 = CARTESIAN_POINT ( 'NONE',  ( 6.140625000614516438, -3.027376345333610441, -5.243569643749999898 ) ) ;
#1312 = CARTESIAN_POINT ( 'NONE',  ( 9.684375000614517504, -4.541064518000419881, 2.621784821874995952 ) ) ;
#1313 = CARTESIAN_POINT ( 'NONE',  ( 15.56250000122903465, 4.330127018922192761, -2.499999999999997780 ) ) ;
#1314 = CARTESIAN_POINT ( 'NONE',  ( 5.784375000614517148, 6.421520780324663323E-16, -5.243569643749999010 ) ) ;
#1315 = CARTESIAN_POINT ( 'NONE',  ( 7.978125000614517681, 6.421520780324663323E-16, -5.243569643749999010 ) ) ;
#1316 = CARTESIAN_POINT ( 'NONE',  ( -1.243387493232115393E-14, 15.70624999877096784, 26.00000000000000000 ) ) ;
#1317 = CARTESIAN_POINT ( 'NONE',  ( 22.93125000122903145, -4.330127018922194537, 2.499999999999995559 ) ) ;
#1318 = CARTESIAN_POINT ( 'NONE',  ( 17.25937500061451502, 0.000000000000000000, 5.243569643749999010 ) ) ;
#1319 = CARTESIAN_POINT ( 'NONE',  ( -1.071796769724488563, 10.64240381056766616, 34.00000000000000000 ) ) ;
#1320 = ORIENTED_EDGE ( 'NONE', *, *, #58649, .T. ) ;
#1321 = CARTESIAN_POINT ( 'NONE',  ( 25.11562500061451431, 3.027376345333613106, -5.243569643749998122 ) ) ;
#1322 = CARTESIAN_POINT ( 'NONE',  ( 9.628125000614517148, -4.541064518000419881, 2.621784821874995952 ) ) ;
#1323 = CARTESIAN_POINT ( 'NONE',  ( 26.74687500061451573, -3.027376345333614438, 5.243569643749998122 ) ) ;
#1324 = CARTESIAN_POINT ( 'NONE',  ( 10.22812500061451679, 6.421520780324663323E-16, -5.243569643749999010 ) ) ;
#1325 = CARTESIAN_POINT ( 'NONE',  ( -4.243569643749998122, 10.44687500061451679, -27.54997392385601174 ) ) ;
#1326 = CARTESIAN_POINT ( 'NONE',  ( 11.25000000122903288, -2.886751345948129988, 4.999999999999997335 ) ) ;
#1327 = CARTESIAN_POINT ( 'NONE',  ( 23.72812500061451502, 6.421520780324663323E-16, -5.243569643749999010 ) ) ;
#1328 = CARTESIAN_POINT ( 'NONE',  ( 4.243569643749999898, 14.14062500061451644, -27.54997392385601529 ) ) ;
#1329 = CARTESIAN_POINT ( 'NONE',  ( 13.65000000122903323, -2.886751345948125991, -5.000000000000000000 ) ) ;
#1330 = CARTESIAN_POINT ( 'NONE',  ( 21.06562500061451715, 3.027376345333613106, -5.243569643749998122 ) ) ;
#1331 = CARTESIAN_POINT ( 'NONE',  ( 12.03749999999999964, -2.886751345948129988, 4.999999999999997335 ) ) ;
#1332 = CARTESIAN_POINT ( 'NONE',  ( 19.79062500061451502, 6.054752690667223547, 3.707466751127219781E-16 ) ) ;
#1333 = CARTESIAN_POINT ( 'NONE',  ( 6.271875000614518747, 3.027376345333612662, -5.243569643749998122 ) ) ;
#1334 = CARTESIAN_POINT ( 'NONE',  ( 20.02500000000000213, 4.330127018922191873, 2.499999999999999556 ) ) ;
#1335 = CARTESIAN_POINT ( 'NONE',  ( 6.787500001229032520, -4.330127018922194537, 2.499999999999995559 ) ) ;
#1336 = CARTESIAN_POINT ( 'NONE',  ( 16.83750000122903145, 6.123233995736764310E-16, -4.999999999999998224 ) ) ;
#1337 = CARTESIAN_POINT ( 'NONE',  ( 13.34062500061451750, -3.027376345333610441, -5.243569643749999898 ) ) ;
#1338 = CARTESIAN_POINT ( 'NONE',  ( 15.55312500061451608, -4.541064518000417216, -2.621784821875001281 ) ) ;
#1339 = CARTESIAN_POINT ( 'NONE',  ( 26.40000000122902790, 5.773502691896255534, 3.535250795749688894E-16 ) ) ;
#1340 = CARTESIAN_POINT ( 'NONE',  ( 20.43749999999999645, 5.773502691896255534, 3.535250795749688894E-16 ) ) ;
#1341 = CARTESIAN_POINT ( 'NONE',  ( 23.25937500061451857, -4.541064518000417216, -2.621784821875001281 ) ) ;
#1342 = DIRECTION ( 'NONE',  ( 0.000000000000000000, 0.000000000000000000, -1.000000000000000000 ) ) ;
#1343 = ADVANCED_FACE ( 'NONE', ( #50096 ), #44567, .T. ) ;
#1344 = CARTESIAN_POINT ( 'NONE',  ( 8.962500001229033231, 0.000000000000000000, 4.999999999999998224 ) ) ;
#1345 = ADVANCED_FACE ( 'NONE', ( #26702 ), #38510, .T. ) ;
#1346 = CARTESIAN_POINT ( 'NONE',  ( 9.759375000614516793, -4.541064518000417216, -2.621784821875001281 ) ) ;
#1347 = CARTESIAN_POINT ( 'NONE',  ( 25.54687500061451644, -3.027376345333610441, -5.243569643749999898 ) ) ;
#1348 =( BOUNDED_CURVE ( )  B_SPLINE_CURVE ( 2, ( #882, #12668, #61829, #45938, #68115, #28582, #1600, #35205, #516 ),
 .UNSPECIFIED., .F., .F. ) 
 B_SPLINE_CURVE_WITH_KNOTS ( ( 3, 2, 2, 2, 3 ),
 ( 0.2065217391304347838, 0.2101449275362318736, 0.2173913043478260809, 0.2246376811594202882, 0.2282608695652174058 ),
 .UNSPECIFIED. ) 
 CURVE ( )  GEOMETRIC_REPRESENTATION_ITEM ( )  RATIONAL_B_SPLINE_CURVE ( ( 0.9330127018922194093, 0.9330127018922194093, 1.000000000000000000, 0.8660254037844387076, 1.000000000000000000, 0.8660254037844387076, 1.000000000000000000, 0.9330127018922190762, 0.9330127018922194093 ) ) 
 REPRESENTATION_ITEM ( '' )  );
#1349 = DIRECTION ( 'NONE',  ( -1.000000000000000000, -0.000000000000000000, -0.000000000000000000 ) ) ;
#1350 = CARTESIAN_POINT ( 'NONE',  ( 21.81562500061451004, -6.054752690667223547, -1.112240025338166033E-15 ) ) ;
#1351 = CARTESIAN_POINT ( 'NONE',  ( 25.99687500061451928, -3.027376345333610441, -5.243569643749999898 ) ) ;
#1352 = CARTESIAN_POINT ( 'NONE',  ( 1.878215178125000495, 18.22812499938548214, 26.74683588394047007 ) ) ;
#1353 = CARTESIAN_POINT ( 'NONE',  ( 19.10625000122903216, 4.330127018922192761, -2.499999999999997780 ) ) ;
#1354 = CARTESIAN_POINT ( 'NONE',  ( 7.509375000614517681, -4.541064518000417216, -2.621784821875001281 ) ) ;
#1355 = CARTESIAN_POINT ( 'NONE',  ( 20.35312500061451502, 0.000000000000000000, 5.243569643749999010 ) ) ;
#1356 = ORIENTED_EDGE ( 'NONE', *, *, #14935, .T. ) ;
#1357 = LINE ( 'NONE', #23866, #61936 ) ;
#1358 = CARTESIAN_POINT ( 'NONE',  ( 27.29062500061451502, -3.027376345333610441, -5.243569643749999898 ) ) ;
#1359 = CARTESIAN_POINT ( 'NONE',  ( 3.909375000614518481, -4.541064518000417216, -2.621784821875001281 ) ) ;
#1360 = CARTESIAN_POINT ( 'NONE',  ( 30.00000000000000000, 6.123233995736764310E-16, -4.999999999999998224 ) ) ;
#1361 = CARTESIAN_POINT ( 'NONE',  ( 11.10000000000000142, 0.000000000000000000, 4.999999999999998224 ) ) ;
#1362 = CARTESIAN_POINT ( 'NONE',  ( 16.50000000000000000, 0.000000000000000000, 4.999999999999998224 ) ) ;
#1363 = CARTESIAN_POINT ( 'NONE',  ( 21.66562500061451502, 3.027376345333611329, 5.243569643749999010 ) ) ;
#1364 = ORIENTED_EDGE ( 'NONE', *, *, #69679, .T. ) ;
#1365 = CARTESIAN_POINT ( 'NONE',  ( 23.96249999999999858, 2.886751345948129099, -4.999999999999998224 ) ) ;
#1366 = CARTESIAN_POINT ( 'NONE',  ( 26.22187500061451715, 3.027376345333611329, 5.243569643749999010 ) ) ;
#1367 = ORIENTED_EDGE ( 'NONE', *, *, #63007, .F. ) ;
#1368 = CARTESIAN_POINT ( 'NONE',  ( 16.26562500061451289, 3.027376345333611329, 5.243569643749999010 ) ) ;
#1369 = CARTESIAN_POINT ( 'NONE',  ( 5.578125000614518214, -4.541064518000419881, 2.621784821874995952 ) ) ;
#1370 = CARTESIAN_POINT ( 'NONE',  ( 18.27187500061451431, 5.824947211148865298E-16, -4.756430356249998326 ) ) ;
#1371 = CARTESIAN_POINT ( 'NONE',  ( 28.49062500061451431, -3.027376345333614438, 5.243569643749998122 ) ) ;
#1372 = CARTESIAN_POINT ( 'NONE',  ( 15.78750000122903430, -4.330127018922194537, 2.499999999999995559 ) ) ;
#1373 = CARTESIAN_POINT ( 'NONE',  ( 22.19999999999999574, 4.330127018922192761, -2.499999999999997780 ) ) ;
#1374 = CARTESIAN_POINT ( 'NONE',  ( 29.81250000000000000, 2.886751345948129099, -4.999999999999998224 ) ) ;
#1375 = CARTESIAN_POINT ( 'NONE',  ( 4.996875000614516615, 6.054752690667223547, 3.707466751127219781E-16 ) ) ;
#1376 = CARTESIAN_POINT ( 'NONE',  ( 9.834375000614517859, 6.421520780324663323E-16, -5.243569643749999010 ) ) ;
#1377 = CARTESIAN_POINT ( 'NONE',  ( 19.32187500061451857, 3.027376345333613106, -5.243569643749998122 ) ) ;
#1378 = CARTESIAN_POINT ( 'NONE',  ( -3.999999999999999112, 19.66250000122903430, -30.00000000000000000 ) ) ;
#1379 = ORIENTED_EDGE ( 'NONE', *, *, #49066, .T. ) ;
#1380 = CARTESIAN_POINT ( 'NONE',  ( 5.259375000614518569, -4.541064518000417216, -2.621784821875001281 ) ) ;
#1381 = CARTESIAN_POINT ( 'NONE',  ( 3.374999999999999556, 4.330127018922191873, 2.499999999999999556 ) ) ;
#1382 = CARTESIAN_POINT ( 'NONE',  ( 4.209375000614516971, 0.000000000000000000, 5.243569643749999010 ) ) ;
#1383 = CARTESIAN_POINT ( 'NONE',  ( 19.08750000000000213, 5.773502691896255534, 3.535250795749688894E-16 ) ) ;
#1384 = CARTESIAN_POINT ( 'NONE',  ( 16.11562500061451786, 3.027376345333613106, -5.243569643749998122 ) ) ;
#1385 = CARTESIAN_POINT ( 'NONE',  ( -4.000000000000000888, 19.96250000000000213, 32.30940107675850470 ) ) ;
#1387 = CARTESIAN_POINT ( 'NONE',  ( 22.31250000000000000, 2.886751345948154857, 4.999999999999951150 ) ) ;
#1386 =( GEOMETRIC_REPRESENTATION_CONTEXT ( 3 ) GLOBAL_UNCERTAINTY_ASSIGNED_CONTEXT ( ( #63913 ) ) GLOBAL_UNIT_ASSIGNED_CONTEXT ( ( #46737, #57797, #30097 ) ) REPRESENTATION_CONTEXT ( 'NONE', 'WORKASPACE' ) );
#1388 = CARTESIAN_POINT ( 'NONE',  ( 20.67187500061451289, 2.746126346562645981, -4.756430356249997438 ) ) ;
#1389 = CARTESIAN_POINT ( 'NONE',  ( 9.778125000614517504, 6.421520780324663323E-16, -5.243569643749999010 ) ) ;
#1390 = CARTESIAN_POINT ( 'NONE',  ( 26.48437500061451644, 6.421520780324663323E-16, -5.243569643749999010 ) ) ;
#1391 = CARTESIAN_POINT ( 'NONE',  ( 9.001249775931846008E-16, 18.62187500061451928, 34.90005215228797653 ) ) ;
#1392 = CARTESIAN_POINT ( 'NONE',  ( 26.78437500061451360, -4.541064518000419881, 2.621784821874995952 ) ) ;
#1393 = CARTESIAN_POINT ( 'NONE',  ( 7.650000000000000355, -4.330127018922190985, -2.500000000000001332 ) ) ;
#1394 = CARTESIAN_POINT ( 'NONE',  ( -3.999999999999997335, 12.05000000122903536, 32.30940107675850470 ) ) ;
#1395 = CARTESIAN_POINT ( 'NONE',  ( 14.91562500061451679, 3.027376345333611329, 5.243569643749999010 ) ) ;
#1396 = CARTESIAN_POINT ( 'NONE',  ( 6.225000001229036073, 2.886751345948126879, 4.999999999999999112 ) ) ;
#1397 = CARTESIAN_POINT ( 'NONE',  ( 17.03437500061451715, 6.421520780324663323E-16, -5.243569643749999010 ) ) ;
#1398 = CARTESIAN_POINT ( 'NONE',  ( 11.52187500061451608, -6.054752690667223547, -1.112240025338166033E-15 ) ) ;
#1399 = CARTESIAN_POINT ( 'NONE',  ( -3.581514519956695342, 3.492045901024759758, -31.79929272433821552 ) ) ;
#1400 = VERTEX_POINT ( 'NONE', #32601 ) ;
#1401 = CARTESIAN_POINT ( 'NONE',  ( 13.49062500061451608, 6.054752690667223547, 3.707466751127219781E-16 ) ) ;
#1402 = CARTESIAN_POINT ( 'NONE',  ( 23.85000000122903430, -2.886751345948129988, 4.999999999999997335 ) ) ;
#1403 = CARTESIAN_POINT ( 'NONE',  ( 12.04687500061451821, -3.027376345333610441, -5.243569643749999898 ) ) ;
#1404 = DIRECTION ( 'NONE',  ( 1.000000000000000000, 0.000000000000000000, 0.000000000000000000 ) ) ;
#1405 = CARTESIAN_POINT ( 'NONE',  ( 15.70312500061451644, 4.541064518000418104, -2.621784821874998173 ) ) ;
#1406 = CARTESIAN_POINT ( 'NONE',  ( 1.071796769724491893, 16.53259618943233278, -26.00000000000000355 ) ) ;
#1407 = CARTESIAN_POINT ( 'NONE',  ( 23.52187500061451786, 3.027376345333611329, 5.243569643749999010 ) ) ;
#1408 = DIRECTION ( 'NONE',  ( -0.000000000000000000, -1.000000000000000000, -0.000000000000000000 ) ) ;
#1409 =( BOUNDED_CURVE ( )  B_SPLINE_CURVE ( 2, ( #21607, #14970, #26429, #37508, #37872, #60028, #60391 ),
 .UNSPECIFIED., .F., .F. ) 
 B_SPLINE_CURVE_WITH_KNOTS ( ( 3, 2, 2, 3 ),
 ( 0.7666666666666668295, 0.7694444444444445974, 0.7722222222222223653, 0.7750000000000001332 ),
 .UNSPECIFIED. ) 
 CURVE ( )  GEOMETRIC_REPRESENTATION_ITEM ( )  RATIONAL_B_SPLINE_CURVE ( ( 0.9999999999999946709, 0.8660254037844440367, 1.000000000000000000, 0.8660254037844387076, 1.000000000000000000, 0.8660254037844333785, 1.000000000000005329 ) ) 
 REPRESENTATION_ITEM ( '' )  );
#1410 = CARTESIAN_POINT ( 'NONE',  ( 11.40000000122903501, -2.886751345948125991, -5.000000000000000000 ) ) ;
#1411 = DIRECTION ( 'NONE',  ( -1.000000000000000000, -0.000000000000000000, -0.000000000000000000 ) ) ;
#1412 = CARTESIAN_POINT ( 'NONE',  ( -1.626862140677534273E-15, 14.63749999999999929, 34.00000000000000000 ) ) ;
#1413 = CARTESIAN_POINT ( 'NONE',  ( -4.243569643749999898, 16.70937500061451786, -30.00000000000000000 ) ) ;
#1414 = CARTESIAN_POINT ( 'NONE',  ( 17.29687500061451999, -3.027376345333614438, 5.243569643749998122 ) ) ;
#1415 = CARTESIAN_POINT ( 'NONE',  ( 18.26250000122903216, 4.330127018922192761, -2.499999999999997780 ) ) ;
#1416 =( BOUNDED_CURVE ( )  B_SPLINE_CURVE ( 2, ( #44094, #66621, #3841, #10826, #38546, #14904, #37445 ),
 .UNSPECIFIED., .F., .F. ) 
 B_SPLINE_CURVE_WITH_KNOTS ( ( 3, 2, 2, 3 ),
 ( 0.008333333333333315870, 0.01111111111111108898, 0.01388888888888885863, 0.01666666666666663174 ),
 .UNSPECIFIED. ) 
 CURVE ( )  GEOMETRIC_REPRESENTATION_ITEM ( )  RATIONAL_B_SPLINE_CURVE ( ( 1.000000000000000888, 0.8660254037844378194, 1.000000000000000000, 0.8660254037844387076, 1.000000000000000000, 0.8660254037844403729, 0.9999999999999983347 ) ) 
 REPRESENTATION_ITEM ( '' )  );
#1417 = CARTESIAN_POINT ( 'NONE',  ( 15.23437500061451644, 6.421520780324663323E-16, -5.243569643749999010 ) ) ;
#1418 = CARTESIAN_POINT ( 'NONE',  ( -4.243569643749997233, 9.996875000614517504, 32.45002607614398471 ) ) ;
#1419 = CARTESIAN_POINT ( 'NONE',  ( 20.88750000122903572, 6.123233995736764310E-16, -4.999999999999998224 ) ) ;
#1420 = CARTESIAN_POINT ( 'NONE',  ( 14.20312500061451644, -4.541064518000417216, -2.621784821875001281 ) ) ;
#1421 = ORIENTED_EDGE ( 'NONE', *, *, #69860, .F. ) ;
#1422 = ORIENTED_EDGE ( 'NONE', *, *, #54762, .F. ) ;
#1423 = CARTESIAN_POINT ( 'NONE',  ( 19.34999999999999787, -4.330127018922190985, -2.500000000000001332 ) ) ;
#1424 = CARTESIAN_POINT ( 'NONE',  ( 4.000000000000000000, 14.33750000000000213, 27.69059892324149885 ) ) ;
#1425 = CARTESIAN_POINT ( 'NONE',  ( 3.328125000614516438, -4.541064518000419881, 2.621784821874995952 ) ) ;
#1426 = CARTESIAN_POINT ( 'NONE',  ( 14.25000000122903465, 5.773502691896255534, 3.535250795749688894E-16 ) ) ;
#1427 = CARTESIAN_POINT ( 'NONE',  ( 26.07187500061451857, 3.027376345333613106, -5.243569643749998122 ) ) ;
#1428 = CARTESIAN_POINT ( 'NONE',  ( 19.97812500061451502, -4.541064518000419881, 2.621784821874995952 ) ) ;
#1429 = CARTESIAN_POINT ( 'NONE',  ( 24.02812500061451573, -4.541064518000419881, 2.621784821874995952 ) ) ;
#1430 = CARTESIAN_POINT ( 'NONE',  ( 3.065625000614517592, 3.027376345333613106, -5.243569643749998122 ) ) ;
#1431 =( BOUNDED_CURVE ( )  B_SPLINE_CURVE ( 2, ( #52853, #2977, #53211, #8514, #2607, #25129, #47670 ),
 .UNSPECIFIED., .F., .T. ) 
 B_SPLINE_CURVE_WITH_KNOTS ( ( 3, 2, 2, 3 ),
 ( 0.6300000000000001155, 0.6333333333333334147, 0.6366666666666668251, 0.6400000000000001243 ),
 .UNSPECIFIED. ) 
 CURVE ( )  GEOMETRIC_REPRESENTATION_ITEM ( )  RATIONAL_B_SPLINE_CURVE ( ( 0.9999999999999955591, 0.8660254037844431485, 1.000000000000000000, 0.8660254037844387076, 1.000000000000000000, 0.8660254037844342667, 1.000000000000004441 ) ) 
 REPRESENTATION_ITEM ( '' )  );
#1432 = CARTESIAN_POINT ( 'NONE',  ( 27.56250000000000000, 2.886751345948129099, -4.999999999999998224 ) ) ;
#1433 = CARTESIAN_POINT ( 'NONE',  ( -5.810221930991193690E-16, 10.10000000122903430, -34.00000000000000000 ) ) ;
#1434 = CARTESIAN_POINT ( 'NONE',  ( 8.934375000614517504, 5.824947211148865298E-16, -4.756430356249998326 ) ) ;
#1435 = CARTESIAN_POINT ( 'NONE',  ( 3.999999999999998668, 17.86250000000000071, 32.30940107675850470 ) ) ;
#1436 = CARTESIAN_POINT ( 'NONE',  ( 8.484601909799253346E-16, 9.875000001229032875, -25.38119784648299770 ) ) ;
#1437 = CARTESIAN_POINT ( 'NONE',  ( -4.243569643749999898, 15.77187500061451608, -32.45002607614398471 ) ) ;
#1438 = CARTESIAN_POINT ( 'NONE',  ( 7.275000001229035007, -5.773502691896255534, -1.060575238724906372E-15 ) ) ;
#1439 = CARTESIAN_POINT ( 'NONE',  ( 6.975000000000002309, 4.330127018922191873, 2.499999999999999556 ) ) ;
#1440 = EDGE_CURVE ( 'NONE', #59687, #30573, #41969, .T. ) ;
#1441 = CARTESIAN_POINT ( 'NONE',  ( 2.925000001229034918, 2.886751345948129099, -4.999999999999998224 ) ) ;
#1442 = CARTESIAN_POINT ( 'NONE',  ( 9.834375000614517859, 6.421520780324663323E-16, -5.243569643749999010 ) ) ;
#1443 = AXIS2_PLACEMENT_3D ( 'NONE', #5329, #54476, #14940 ) ;
#1444 = CARTESIAN_POINT ( 'NONE',  ( 29.31562500061451715, 3.027376345333611329, 5.243569643749999010 ) ) ;
#1445 = DIRECTION ( 'NONE',  ( 1.000000000000000000, 0.000000000000000000, 0.000000000000000000 ) ) ;
#1446 = CARTESIAN_POINT ( 'NONE',  ( 5.437500001229035540, -4.330127018922194537, 2.499999999999995559 ) ) ;
#1447 = CARTESIAN_POINT ( 'NONE',  ( 8.634375000614518569, 4.541064518000418104, 2.621784821874999949 ) ) ;
#1448 = CARTESIAN_POINT ( 'NONE',  ( 11.55937500061451928, -4.541064518000417216, -2.621784821875001281 ) ) ;
#1449 = CARTESIAN_POINT ( 'NONE',  ( 5.775000000000002132, -4.330127018922194537, 2.499999999999995559 ) ) ;
#1450 = CARTESIAN_POINT ( 'NONE',  ( -4.243569643749998122, 14.44062500061459531, 32.45002607614398471 ) ) ;
#1451 = CARTESIAN_POINT ( 'NONE',  ( 20.85937500061451644, 0.000000000000000000, 5.243569643749999010 ) ) ;
#1452 = CARTESIAN_POINT ( 'NONE',  ( 2.009231068734822045, 25.40577629059018605, 33.46852441891628871 ) ) ;
#1453 = CARTESIAN_POINT ( 'NONE',  ( 6.600000000000001421, 0.000000000000000000, 4.999999999999998224 ) ) ;
#1454 = CARTESIAN_POINT ( 'NONE',  ( 25.61250000122903359, 0.000000000000000000, 4.999999999999998224 ) ) ;
#1455 = CARTESIAN_POINT ( 'NONE',  ( 17.85937500061451644, 2.746126346562645981, -4.756430356249997438 ) ) ;
#1456 = CARTESIAN_POINT ( 'NONE',  ( 21.55312500061451431, 4.541064518000418104, -2.621784821874998173 ) ) ;
#1457 = CARTESIAN_POINT ( 'NONE',  ( 14.24062500061451608, -3.027376345333610441, -5.243569643749999898 ) ) ;
#1458 = CARTESIAN_POINT ( 'NONE',  ( 26.29687500061451644, -4.119189519843965641, -2.378215178125001383 ) ) ;
#1459 = CARTESIAN_POINT ( 'NONE',  ( 10.65937500061451715, -4.541064518000417216, -2.621784821875001281 ) ) ;
#1460 = CARTESIAN_POINT ( 'NONE',  ( 28.64999999999999858, 0.000000000000000000, 4.999999999999998224 ) ) ;
#1461 = CARTESIAN_POINT ( 'NONE',  ( 21.97500000122903074, 2.886751345948126879, 4.999999999999999112 ) ) ;
#1462 = CARTESIAN_POINT ( 'NONE',  ( -3.999999999999999112, 18.31250000122903288, -30.00000000000000000 ) ) ;
#1463 = CARTESIAN_POINT ( 'NONE',  ( 12.00937500061451857, -4.541064518000417216, -2.621784821875001281 ) ) ;
#1464 = CARTESIAN_POINT ( 'NONE',  ( 28.54687500061451644, -3.027376345333614438, 5.243569643749998122 ) ) ;
#1465 = CARTESIAN_POINT ( 'NONE',  ( 4.171875000614517326, 3.027376345333611329, 5.243569643749999010 ) ) ;
#1466 = DIRECTION ( 'NONE',  ( -1.000000000000000000, -0.000000000000000000, -0.000000000000000000 ) ) ;
#1467 = CARTESIAN_POINT ( 'NONE',  ( 21.27187500061451786, 3.027376345333611329, 5.243569643749999010 ) ) ;
#1468 = CARTESIAN_POINT ( 'NONE',  ( 14.33437500061451786, 6.421520780324663323E-16, -5.243569643749999010 ) ) ;
#1469 = CARTESIAN_POINT ( 'NONE',  ( -7.967954043666661671E-16, 18.94062499938548783, 34.33755215474603517 ) ) ;
#1470 = CARTESIAN_POINT ( 'NONE',  ( 26.84999999999999787, 0.000000000000000000, 4.999999999999998224 ) ) ;
#1471 = CARTESIAN_POINT ( 'NONE',  ( 4.000000000000000000, 12.53749999999999964, 27.69059892324149530 ) ) ;
#1472 = CARTESIAN_POINT ( 'NONE',  ( -3.000416591977282496E-16, 14.79687500061451821, -34.90005215228797653 ) ) ;
#1473 = CARTESIAN_POINT ( 'NONE',  ( 27.83437500061451786, 5.824947211148865298E-16, -4.756430356249998326 ) ) ;
#1474 = CARTESIAN_POINT ( 'NONE',  ( 17.99062500061451786, 6.054752690667223547, 3.707466751127219781E-16 ) ) ;
#1475 = CARTESIAN_POINT ( 'NONE',  ( 7.950000000000001954, 0.000000000000000000, 4.999999999999998224 ) ) ;
#1476 = CARTESIAN_POINT ( 'NONE',  ( 12.22500000122903430, -5.773502691896255534, -1.060575238724906372E-15 ) ) ;
#1477 = CARTESIAN_POINT ( 'NONE',  ( 14.58750000000000036, 5.773502691896255534, 3.535250795749688894E-16 ) ) ;
#1478 = ADVANCED_FACE ( 'NONE', ( #27429 ), #9339, .F. ) ;
#1479 = CARTESIAN_POINT ( 'NONE',  ( -1.473773219643375931, 9.816672173337614993, 25.95083121279759197 ) ) ;
#1480 = CARTESIAN_POINT ( 'NONE',  ( 14.51250000122903394, -4.330127018922190985, -2.500000000000001332 ) ) ;
#1481 = CARTESIAN_POINT ( 'NONE',  ( 25.88437500061451502, -4.541064518000419881, 2.621784821874995952 ) ) ;
#1482 = VERTEX_POINT ( 'NONE', #21504 ) ;
#1483 = CARTESIAN_POINT ( 'NONE',  ( 20.05312500061451431, -4.541064518000417216, -2.621784821875001281 ) ) ;
#1484 = CARTESIAN_POINT ( 'NONE',  ( 20.63437500061451857, 6.421520780324663323E-16, -5.243569643749999010 ) ) ;
#1485 = CARTESIAN_POINT ( 'NONE',  ( 3.075000000000001510, -4.330127018922194537, 2.499999999999995559 ) ) ;
#1486 = CARTESIAN_POINT ( 'NONE',  ( 6.740625000614516082, 6.054752690667223547, 3.707466751127219781E-16 ) ) ;
#1487 = CARTESIAN_POINT ( 'NONE',  ( 22.94062500061451715, 6.054752690667223547, 3.707466751127219781E-16 ) ) ;
#1488 = CARTESIAN_POINT ( 'NONE',  ( 12.23437500061451821, 4.541064518000418104, 2.621784821874999949 ) ) ;
#1489 = CARTESIAN_POINT ( 'NONE',  ( 16.24687500061451573, 6.054752690667223547, 3.707466751127219781E-16 ) ) ;
#1490 = CARTESIAN_POINT ( 'NONE',  ( -4.243569643749997233, 15.34062500061451750, 32.45002607614398471 ) ) ;
#1491 = CARTESIAN_POINT ( 'NONE',  ( 18.18750000122903288, 6.123233995736764310E-16, -4.999999999999998224 ) ) ;
#1492 = CARTESIAN_POINT ( 'NONE',  ( 14.59687500061452070, -2.746126346562646425, 4.756430356249996549 ) ) ;
#1493 = CARTESIAN_POINT ( 'NONE',  ( 9.853125000614516793, 4.541064518000418104, -2.621784821874998173 ) ) ;
#1494 = CARTESIAN_POINT ( 'NONE',  ( 3.309375000614518836, 0.000000000000000000, 5.243569643749999010 ) ) ;
#1495 = CARTESIAN_POINT ( 'NONE',  ( 29.39062500061451289, -3.027376345333614438, 5.243569643749998122 ) ) ;
#1496 = CARTESIAN_POINT ( 'NONE',  ( 25.17187500061451644, 3.027376345333613106, -5.243569643749998122 ) ) ;
#1497 = CARTESIAN_POINT ( 'NONE',  ( 17.09062500061451573, 6.054752690667223547, 3.707466751127219781E-16 ) ) ;
#1498 = CARTESIAN_POINT ( 'NONE',  ( 26.96250000122903145, 0.000000000000000000, 4.999999999999998224 ) ) ;
#1499 = CARTESIAN_POINT ( 'NONE',  ( 25.67812500061451431, 4.541064518000418104, 2.621784821874999949 ) ) ;
#1500 = AXIS2_PLACEMENT_3D ( 'NONE', #34507, #21976, #21609 ) ;
#1501 = CARTESIAN_POINT ( 'NONE',  ( 21.08437500061451786, 6.421520780324663323E-16, -5.243569643749999010 ) ) ;
#1502 = CARTESIAN_POINT ( 'NONE',  ( 17.16562500061451502, 3.027376345333611329, 5.243569643749999010 ) ) ;
#1503 = CARTESIAN_POINT ( 'NONE',  ( 2.121784821875001281, 16.40937500061452070, 33.67503911421598417 ) ) ;
#1504 = CARTESIAN_POINT ( 'NONE',  ( 22.75312500061451360, -4.541064518000417216, -2.621784821875001281 ) ) ;
#1505 = DIRECTION ( 'NONE',  ( -1.000000000000000000, -0.000000000000000000, -0.000000000000000000 ) ) ;
#1506 = ORIENTED_EDGE ( 'NONE', *, *, #71856, .F. ) ;
#1507 = CARTESIAN_POINT ( 'NONE',  ( 25.12499999999999645, -4.330127018922194537, 2.499999999999995559 ) ) ;
#1508 = CARTESIAN_POINT ( 'NONE',  ( -2.828200636599751609E-16, 13.13750000000000107, -34.61880215351700230 ) ) ;
#1509 = CARTESIAN_POINT ( 'NONE',  ( -1.878215178125001827, 19.80312499938548143, 33.25316411605952283 ) ) ;
#1510 = CARTESIAN_POINT ( 'NONE',  ( 29.42812500061451431, -4.541064518000419881, 2.621784821874995952 ) ) ;
#1511 = CARTESIAN_POINT ( 'NONE',  ( 9.365625000614519635, 3.027376345333613106, -5.243569643749998122 ) ) ;
#1512 = CARTESIAN_POINT ( 'NONE',  ( 22.98750000122903003, -4.330127018922194537, 2.499999999999995559 ) ) ;
#1513 = CARTESIAN_POINT ( 'NONE',  ( 28.19062500061451715, -3.027376345333610441, -5.243569643749999898 ) ) ;
#1514 = CARTESIAN_POINT ( 'NONE',  ( 26.17500000000000071, 6.123233995736764310E-16, -4.999999999999998224 ) ) ;
#1515 = CARTESIAN_POINT ( 'NONE',  ( 3.999999999999998668, 15.87500000122903465, -32.30940107675850470 ) ) ;
#1516 = CARTESIAN_POINT ( 'NONE',  ( -5.810221930991193690E-16, 11.45000000122903216, -34.00000000000000000 ) ) ;
#1517 = CARTESIAN_POINT ( 'NONE',  ( 9.478125000614515017, 4.541064518000418104, 2.621784821874999949 ) ) ;
#1518 = VERTEX_POINT ( 'NONE', #4538 ) ;
#1519 = CARTESIAN_POINT ( 'NONE',  ( 25.52812500061451573, 6.421520780324663323E-16, -5.243569643749999010 ) ) ;
#1520 = CARTESIAN_POINT ( 'NONE',  ( 8.315625000614515372, -6.054752690667223547, -1.112240025338166033E-15 ) ) ;
#1521 = CARTESIAN_POINT ( 'NONE',  ( 5.015625000614518214, 3.027376345333611329, 5.243569643749999010 ) ) ;
#1522 = CARTESIAN_POINT ( 'NONE',  ( 15.64687500061451608, -2.746126346562642428, -4.756430356249999214 ) ) ;
#1523 = DIRECTION ( 'NONE',  ( 0.000000000000000000, 0.000000000000000000, 1.000000000000000000 ) ) ;
#1524 = CARTESIAN_POINT ( 'NONE',  ( 14.28750000000000142, -2.886751345948129988, 4.999999999999997335 ) ) ;
#1525 = CARTESIAN_POINT ( 'NONE',  ( 13.50937500061451679, 4.541064518000418104, -2.621784821874998173 ) ) ;
#1526 = CARTESIAN_POINT ( 'NONE',  ( 12.18750000122903465, -4.330127018922194537, 2.499999999999995559 ) ) ;
#1527 = CARTESIAN_POINT ( 'NONE',  ( 16.92187500061451999, -6.054752690667223547, -1.112240025338166033E-15 ) ) ;
#1528 = CARTESIAN_POINT ( 'NONE',  ( 18.26249999999999929, 2.886751345948126879, 4.999999999999999112 ) ) ;
#1529 = CARTESIAN_POINT ( 'NONE',  ( 8.034375000614518925, 6.421520780324663323E-16, -5.243569643749999010 ) ) ;
#1530 = CARTESIAN_POINT ( 'NONE',  ( 2.121784821874999061, 11.10312500061451679, -33.67503911421598417 ) ) ;
#1531 = CARTESIAN_POINT ( 'NONE',  ( 45.00000000000000000, 6.123233995736764310E-16, -4.999999999999998224 ) ) ;
#1532 = CARTESIAN_POINT ( 'NONE',  ( 24.38437500061451502, -2.746126346562646425, 4.756430356249996549 ) ) ;
#1533 = CARTESIAN_POINT ( 'NONE',  ( 30.00000000000000000, 0.000000000000000000, 0.000000000000000000 ) ) ;
#1534 = CARTESIAN_POINT ( 'NONE',  ( 25.30312500061451431, 0.000000000000000000, 5.243569643749999010 ) ) ;
#1535 = CARTESIAN_POINT ( 'NONE',  ( 45.00000000000000000, 0.000000000000000000, 4.999999999999998224 ) ) ;
#1536 = CARTESIAN_POINT ( 'NONE',  ( 28.54687500061451644, -3.027376345333614438, 5.243569643749998122 ) ) ;
#1537 = CARTESIAN_POINT ( 'NONE',  ( 24.18750000000000355, -2.886751345948129988, 4.999999999999997335 ) ) ;
#1538 = CARTESIAN_POINT ( 'NONE',  ( 6.290625000614517681, 6.054752690667223547, 3.707466751127219781E-16 ) ) ;
#1539 = CARTESIAN_POINT ( 'NONE',  ( 25.47187500061451360, 5.824947211148865298E-16, -4.756430356249998326 ) ) ;
#1540 = CARTESIAN_POINT ( 'NONE',  ( 20.14687500061451786, -3.027376345333610441, -5.243569643749999898 ) ) ;
#1541 = CARTESIAN_POINT ( 'NONE',  ( 10.50937500061451502, -5.492252693125287522, -1.008910452111647106E-15 ) ) ;
#1542 = CARTESIAN_POINT ( 'NONE',  ( 3.665625000614517681, 3.027376345333611329, 5.243569643749999010 ) ) ;
#1543 = CARTESIAN_POINT ( 'NONE',  ( 7.696875000614516793, 6.054752690667223547, 3.707466751127219781E-16 ) ) ;
#1544 = ORIENTED_EDGE ( 'NONE', *, *, #61840, .F. ) ;
#1545 = CARTESIAN_POINT ( 'NONE',  ( 19.73437500061451644, 6.421520780324663323E-16, -5.243569643749999010 ) ) ;
#1546 = DIRECTION ( 'NONE',  ( 0.000000000000000000, 0.000000000000000000, 1.000000000000000000 ) ) ;
#1547 = CARTESIAN_POINT ( 'NONE',  ( 27.48749999999999716, -2.886751345948125991, -5.000000000000000000 ) ) ;
#1548 = CARTESIAN_POINT ( 'NONE',  ( 28.69687500061451502, -3.027376345333610441, -5.243569643749999898 ) ) ;
#1549 = DIRECTION ( 'NONE',  ( 0.000000000000000000, 0.000000000000000000, -1.000000000000000000 ) ) ;
#1550 = CARTESIAN_POINT ( 'NONE',  ( 12.28125000122903110, 6.123233995736764310E-16, -4.999999999999998224 ) ) ;
#1551 = ORIENTED_EDGE ( 'NONE', *, *, #27962, .F. ) ;
#1552 = CARTESIAN_POINT ( 'NONE',  ( 9.225000000000001421, 4.330127018922191873, 2.499999999999999556 ) ) ;
#1553 = CARTESIAN_POINT ( 'NONE',  ( 12.19687500061451502, 0.000000000000000000, 4.756430356249998326 ) ) ;
#1554 = CARTESIAN_POINT ( 'NONE',  ( 24.21562500061451573, 3.027376345333613106, -5.243569643749998122 ) ) ;
#1555 = CARTESIAN_POINT ( 'NONE',  ( 13.27500000000000213, 4.330127018922191873, 2.499999999999999556 ) ) ;
#1556 = CARTESIAN_POINT ( 'NONE',  ( 7.837500001229035007, 6.123233995736764310E-16, -4.999999999999998224 ) ) ;
#1557 = CARTESIAN_POINT ( 'NONE',  ( 6.740625000614516082, 6.054752690667223547, 3.707466751127219781E-16 ) ) ;
#1558 = CARTESIAN_POINT ( 'NONE',  ( 21.41250000000000497, 2.886751345948126879, 4.999999999999999112 ) ) ;
#1559 = EDGE_CURVE ( 'NONE', #329, #59300, #16943, .T. ) ;
#1560 = CARTESIAN_POINT ( 'NONE',  ( 21.62812500061451360, 4.541064518000418104, 2.621784821874999949 ) ) ;
#1561 = FACE_OUTER_BOUND ( 'NONE', #67156, .T. ) ;
#1562 = CARTESIAN_POINT ( 'NONE',  ( 25.46250000122903501, 4.330127018922192761, -2.499999999999997780 ) ) ;
#1563 = CARTESIAN_POINT ( 'NONE',  ( -3.756430356250000990, 17.85312499938548214, 32.16877607737301048 ) ) ;
#1564 = CARTESIAN_POINT ( 'NONE',  ( 5.700000000000000178, 0.000000000000000000, 4.999999999999998224 ) ) ;
#1565 = VERTEX_POINT ( 'NONE', #65849 ) ;
#1566 = CARTESIAN_POINT ( 'NONE',  ( 22.94062500061451715, 6.054752690667223547, 3.707466751127219781E-16 ) ) ;
#1567 = CARTESIAN_POINT ( 'NONE',  ( 28.90312500061451217, 0.000000000000000000, 5.243569643749999010 ) ) ;
#1568 = CARTESIAN_POINT ( 'NONE',  ( 27.94687500061451502, 6.054752690667223547, 3.707466751127219781E-16 ) ) ;
#1569 = CARTESIAN_POINT ( 'NONE',  ( 17.93437500061451928, 6.421520780324663323E-16, -5.243569643749999010 ) ) ;
#1570 = CARTESIAN_POINT ( 'NONE',  ( 13.94062500061451892, 6.054752690667223547, 3.707466751127219781E-16 ) ) ;
#1571 = PLANE ( 'NONE',  #40404 ) ;
#1572 = CARTESIAN_POINT ( 'NONE',  ( 25.05000000122903714, 5.773502691896255534, 3.535250795749688894E-16 ) ) ;
#1573 = CARTESIAN_POINT ( 'NONE',  ( 21.83437500061451786, -4.119189519843968306, 2.378215178124996054 ) ) ;
#1574 = CARTESIAN_POINT ( 'NONE',  ( 15.66562500061451857, 3.027376345333612662, -5.243569643749998122 ) ) ;
#1575 = CARTESIAN_POINT ( 'NONE',  ( -3.999999999999999112, 16.81250000000000000, -32.30940107675850470 ) ) ;
#1576 = CARTESIAN_POINT ( 'NONE',  ( 0.000000000000000000, 27.50000000000000000, 26.00000000000000000 ) ) ;
#1577 = CARTESIAN_POINT ( 'NONE',  ( 12.34687500061452070, -3.027376345333614438, 5.243569643749998122 ) ) ;
#1578 = CARTESIAN_POINT ( 'NONE',  ( 11.10937500061451644, -4.541064518000417216, -2.621784821875001281 ) ) ;
#1579 = CARTESIAN_POINT ( 'NONE',  ( 19.09687500061451360, -3.027376345333614438, 5.243569643749998122 ) ) ;
#1580 = VERTEX_POINT ( 'NONE', #26328 ) ;
#1581 = CARTESIAN_POINT ( 'NONE',  ( 9.750000000000001776, 0.000000000000000000, 4.999999999999998224 ) ) ;
#1582 = CARTESIAN_POINT ( 'NONE',  ( 23.61562500061451431, -6.054752690667223547, -1.112240025338166033E-15 ) ) ;
#1583 = CARTESIAN_POINT ( 'NONE',  ( 18.72187500061451360, -6.054752690667223547, -1.112240025338166033E-15 ) ) ;
#1584 = CARTESIAN_POINT ( 'NONE',  ( 24.96562500061451573, -6.054752690667223547, -1.112240025338166033E-15 ) ) ;
#1585 = CARTESIAN_POINT ( 'NONE',  ( 9.675000001229031810, 2.886751345948129099, -4.999999999999997335 ) ) ;
#1586 = CARTESIAN_POINT ( 'NONE',  ( -2.000000000000000000, 14.97499999999999964, 26.53589838486224650 ) ) ;
#1587 = CARTESIAN_POINT ( 'NONE',  ( 2.934375000614518392, -4.541064518000419881, 2.621784821874995952 ) ) ;
#1588 = CARTESIAN_POINT ( 'NONE',  ( 9.525000001229033231, -5.773502691896255534, -1.060575238724906372E-15 ) ) ;
#1589 = CARTESIAN_POINT ( 'NONE',  ( 5.700000001229033941, 5.773502691896255534, 3.535250795749688894E-16 ) ) ;
#1590 = CARTESIAN_POINT ( 'NONE',  ( 21.41250000000000142, 2.886751345948126879, 4.999999999999998224 ) ) ;
#1591 = CARTESIAN_POINT ( 'NONE',  ( 27.60000000122903430, -2.886751345948125991, -5.000000000000000000 ) ) ;
#1592 = CARTESIAN_POINT ( 'NONE',  ( 3.756430356250000546, 12.79062499938548392, 27.83122392262697886 ) ) ;
#1593 = CARTESIAN_POINT ( 'NONE',  ( 8.634375000614518569, 4.541064518000418104, 2.621784821874999949 ) ) ;
#1594 = CARTESIAN_POINT ( 'NONE',  ( 18.21562500061451573, -6.054752690667223547, -1.112240025338166033E-15 ) ) ;
#1595 = CARTESIAN_POINT ( 'NONE',  ( 11.07187500061451679, -6.054752690667223547, -1.112240025338166033E-15 ) ) ;
#1596 = CARTESIAN_POINT ( 'NONE',  ( 3.440625000614518036, -3.027376345333610441, -5.243569643749999898 ) ) ;
#1597 = CARTESIAN_POINT ( 'NONE',  ( 18.64687500061451786, -3.027376345333614438, 5.243569643749998122 ) ) ;
#1598 = CARTESIAN_POINT ( 'NONE',  ( 8.334375000614516082, -4.541064518000419881, 2.621784821874995952 ) ) ;
#1599 = CARTESIAN_POINT ( 'NONE',  ( 3.403125000614518836, -4.541064518000417216, -2.621784821875001281 ) ) ;
#1600 = CARTESIAN_POINT ( 'NONE',  ( -2.000000000000000000, 17.67500000000000071, 26.53589838486224650 ) ) ;
#1601 = CARTESIAN_POINT ( 'NONE',  ( 8.953125000614518214, 4.541064518000418104, -2.621784821874998173 ) ) ;
#1602 = CARTESIAN_POINT ( 'NONE',  ( 17.50312500061451715, 4.541064518000418104, -2.621784821874998173 ) ) ;
#1603 = ORIENTED_EDGE ( 'NONE', *, *, #37808, .F. ) ;
#1604 = CARTESIAN_POINT ( 'NONE',  ( 5.062500001229035540, -4.330127018922190985, -2.500000000000001332 ) ) ;
#1605 = CARTESIAN_POINT ( 'NONE',  ( 13.79062500061451502, -3.027376345333610441, -5.243569643749999898 ) ) ;
#1606 = CARTESIAN_POINT ( 'NONE',  ( 13.67812500061451786, -4.541064518000419881, 2.621784821874995952 ) ) ;
#1607 = CARTESIAN_POINT ( 'NONE',  ( 24.30937500061451573, 4.119189519843966529, -2.378215178124998275 ) ) ;
#1608 = CARTESIAN_POINT ( 'NONE',  ( 13.04999999999999893, -4.330127018922190985, -2.500000000000001332 ) ) ;
#1609 = CARTESIAN_POINT ( 'NONE',  ( 6.862500001229034474, -4.330127018922190985, -2.500000000000001332 ) ) ;
#1610 = CARTESIAN_POINT ( 'NONE',  ( 4.265625000614517326, -6.054752690667223547, -1.112240025338166033E-15 ) ) ;
#1611 = EDGE_CURVE ( 'NONE', #33907, #61284, #66577, .T. ) ;
#1612 = CARTESIAN_POINT ( 'NONE',  ( 15.30937500061451750, 4.541064518000418104, -2.621784821874998173 ) ) ;
#1613 = CARTESIAN_POINT ( 'NONE',  ( 17.58750000122903145, -4.330127018922194537, 2.499999999999995559 ) ) ;
#1614 = CARTESIAN_POINT ( 'NONE',  ( 25.05000000000000071, 0.000000000000000000, 4.999999999999998224 ) ) ;
#1615 = EDGE_CURVE ( 'NONE', #57497, #37161, #42952, .T. ) ;
#1616 = CARTESIAN_POINT ( 'NONE',  ( 4.243569643749999898, 19.57812500061451644, -30.00000000000000000 ) ) ;
#1617 = CARTESIAN_POINT ( 'NONE',  ( 8.587500000000002132, -2.886751345948126435, -5.000000000000000000 ) ) ;
#1618 = DIRECTION ( 'NONE',  ( 0.000000000000000000, 1.000000000000000000, -8.673617379884037937E-17 ) ) ;
#1619 = CARTESIAN_POINT ( 'NONE',  ( 2.955228467731844333, 4.033190387708875946, -2.955228467731844333 ) ) ;
#1620 = FACE_OUTER_BOUND ( 'NONE', #52178, .T. ) ;
#1621 = CARTESIAN_POINT ( 'NONE',  ( 18.64687500061451786, -3.027376345333614438, 5.243569643749998122 ) ) ;
#1622 = EDGE_CURVE ( 'NONE', #69015, #46020, #617, .T. ) ;
#1623 =( BOUNDED_CURVE ( )  B_SPLINE_CURVE ( 2, ( #58786, #30724, #19625, #35894, #2293, #13353, #60526 ),
 .UNSPECIFIED., .F., .F. ) 
 B_SPLINE_CURVE_WITH_KNOTS ( ( 3, 2, 2, 3 ),
 ( 0.8083333333333333481, 0.8111111111111111160, 0.8138888888888888840, 0.8166666666666666519 ),
 .UNSPECIFIED. ) 
 CURVE ( )  GEOMETRIC_REPRESENTATION_ITEM ( )  RATIONAL_B_SPLINE_CURVE ( ( 1.000000000000000000, 0.8660254037844387076, 1.000000000000000000, 0.8660254037844387076, 1.000000000000000000, 0.8660254037844387076, 1.000000000000000000 ) ) 
 REPRESENTATION_ITEM ( '' )  );
#1624 = CARTESIAN_POINT ( 'NONE',  ( 15.29999999999999893, -4.330127018922190985, -2.500000000000001332 ) ) ;
#1625 = CARTESIAN_POINT ( 'NONE',  ( 13.45312500061451466, 4.541064518000418104, -2.621784821874998173 ) ) ;
#1626 = CARTESIAN_POINT ( 'NONE',  ( 8.381250001229034297, 4.330127018922191873, 2.499999999999999556 ) ) ;
#1627 = CARTESIAN_POINT ( 'NONE',  ( 22.68750000122903288, 6.123233995736764310E-16, -4.999999999999998224 ) ) ;
#1628 = CARTESIAN_POINT ( 'NONE',  ( 25.24687500061451573, 6.054752690667223547, 3.707466751127219781E-16 ) ) ;
#1629 = CARTESIAN_POINT ( 'NONE',  ( 17.48437500061451644, 5.492252693125287522, 3.363034840372157021E-16 ) ) ;
#1630 = CARTESIAN_POINT ( 'NONE',  ( 9.478125000614515017, 4.541064518000418104, 2.621784821874999949 ) ) ;
#1631 = CARTESIAN_POINT ( 'NONE',  ( 14.82187500061451679, 3.027376345333613106, -5.243569643749998122 ) ) ;
#1632 = ORIENTED_EDGE ( 'NONE', *, *, #53492, .F. ) ;
#1633 = CARTESIAN_POINT ( 'NONE',  ( 27.36562500061451786, 3.027376345333613106, -5.243569643749998122 ) ) ;
#1634 = CARTESIAN_POINT ( 'NONE',  ( 20.05312500061451431, -4.541064518000417216, -2.621784821875001281 ) ) ;
#1635 = CARTESIAN_POINT ( 'NONE',  ( -5.810221930991193690E-16, 10.88750000000000107, 26.00000000000000355 ) ) ;
#1636 = EDGE_CURVE ( 'NONE', #53798, #61419, #18855, .T. ) ;
#1637 = CARTESIAN_POINT ( 'NONE',  ( -2.000000000000000000, 14.18750000122903288, -33.46410161513775705 ) ) ;
#1638 = CARTESIAN_POINT ( 'NONE',  ( 11.06250000000000000, 2.886751345948126879, 4.999999999999999112 ) ) ;
#1639 = CARTESIAN_POINT ( 'NONE',  ( 18.78750000122903430, 4.330127018922191873, 2.499999999999999556 ) ) ;
#1640 = CARTESIAN_POINT ( 'NONE',  ( 23.25000000122902932, 5.773502691896255534, 3.535250795749688401E-16 ) ) ;
#1641 = CARTESIAN_POINT ( 'NONE',  ( 9.984375000614516438, -2.746126346562646425, 4.756430356249996549 ) ) ;
#1642 = ORIENTED_EDGE ( 'NONE', *, *, #4558, .T. ) ;
#1643 = CARTESIAN_POINT ( 'NONE',  ( 16.94999999999999929, 0.000000000000000000, 4.999999999999998224 ) ) ;
#1644 = CARTESIAN_POINT ( 'NONE',  ( 21.11249999999999716, -5.773502691896255534, -1.060575238724906372E-15 ) ) ;
#1645 = CARTESIAN_POINT ( 'NONE',  ( 18.19687500061451502, -3.027376345333614438, 5.243569643749998122 ) ) ;
#1646 = CARTESIAN_POINT ( 'NONE',  ( 24.02812500061451573, -4.541064518000419881, 2.621784821874995952 ) ) ;
#1647 = EDGE_LOOP ( 'NONE', ( #29345, #9948, #41169, #29072 ) ) ;
#1648 = CARTESIAN_POINT ( 'NONE',  ( 5.390625000614518214, 6.054752690667223547, 3.707466751127219781E-16 ) ) ;
#1649 = CARTESIAN_POINT ( 'NONE',  ( 28.48125000122902861, 6.123233995736764310E-16, -4.999999999999998224 ) ) ;
#1650 = CARTESIAN_POINT ( 'NONE',  ( 12.67499999999999893, 6.123233995736764310E-16, -4.999999999999998224 ) ) ;
#1651 = CARTESIAN_POINT ( 'NONE',  ( 4.243569643749999898, 17.29062500061451502, 32.45002607614398471 ) ) ;
#1652 = CARTESIAN_POINT ( 'NONE',  ( 28.45312500061451289, 0.000000000000000000, 5.243569643749999010 ) ) ;
#1653 = CARTESIAN_POINT ( 'NONE',  ( 10.01250000000000107, 2.886751345948129099, -4.999999999999998224 ) ) ;
#1654 = CARTESIAN_POINT ( 'NONE',  ( -3.756430356249999214, 17.32812499938548356, 27.83122392262697531 ) ) ;
#1655 = CARTESIAN_POINT ( 'NONE',  ( 25.99687500061451928, -3.027376345333610441, -5.243569643749999898 ) ) ;
#1656 = VERTEX_POINT ( 'NONE', #44433 ) ;
#1657 = CARTESIAN_POINT ( 'NONE',  ( 21.14062500061451289, 6.054752690667223547, 3.707466751127219781E-16 ) ) ;
#1658 = CARTESIAN_POINT ( 'NONE',  ( 22.69687500061451857, -3.027376345333614438, 5.243569643749998122 ) ) ;
#1659 = CARTESIAN_POINT ( 'NONE',  ( -2.121784821874996840, 15.82812500061459282, -26.32496088578401583 ) ) ;
#1660 = CARTESIAN_POINT ( 'NONE',  ( 6.215625000614517504, 3.027376345333613106, -5.243569643749998122 ) ) ;
#1661 = CARTESIAN_POINT ( 'NONE',  ( 16.61250000122903359, 0.000000000000000000, 4.999999999999998224 ) ) ;
#1662 = CARTESIAN_POINT ( 'NONE',  ( 22.82812500061451644, 6.421520780324663323E-16, -5.243569643749999010 ) ) ;
#1663 = CARTESIAN_POINT ( 'NONE',  ( 26.97187500061451360, 4.119189519843966529, 2.378215178124999607 ) ) ;
#1664 = CARTESIAN_POINT ( 'NONE',  ( 13.84687500061451537, -2.746126346562642428, -4.756430356249999214 ) ) ;
#1665 = CARTESIAN_POINT ( 'NONE',  ( 17.18437500061451573, 4.541064518000418104, 2.621784821874999949 ) ) ;
#1666 = CARTESIAN_POINT ( 'NONE',  ( 19.99687500061451573, -3.027376345333614438, 5.243569643749998122 ) ) ;
#1667 = CARTESIAN_POINT ( 'NONE',  ( 28.17187500061451644, -6.054752690667223547, -1.112240025338166033E-15 ) ) ;
#1668 = CARTESIAN_POINT ( 'NONE',  ( 2.121784821874999061, 15.65937500061451892, 26.32496088578401583 ) ) ;
#1669 = CARTESIAN_POINT ( 'NONE',  ( 6.928125000614516082, -4.541064518000419881, 2.621784821874995952 ) ) ;
#1670 = CARTESIAN_POINT ( 'NONE',  ( -5.810221930991193690E-16, 18.98750000000000071, 26.00000000000000355 ) ) ;
#1671 = CARTESIAN_POINT ( 'NONE',  ( 5.559375000614517504, 0.000000000000000000, 5.243569643749999010 ) ) ;
#1672 = CARTESIAN_POINT ( 'NONE',  ( 26.51249999999999929, -5.773502691896255534, -1.060575238724906372E-15 ) ) ;
#1673 = CARTESIAN_POINT ( 'NONE',  ( 4.303125000614516971, -4.541064518000417216, -2.621784821875001281 ) ) ;
#1674 = CARTESIAN_POINT ( 'NONE',  ( 10.17187500061451999, -6.054752690667223547, -1.112240025338166033E-15 ) ) ;
#1675 = CARTESIAN_POINT ( 'NONE',  ( 16.12500000122903288, 2.886751345948126879, 4.999999999999999112 ) ) ;
#1676 = CARTESIAN_POINT ( 'NONE',  ( 6.796875000614516438, 6.054752690667223547, 3.707466751127219781E-16 ) ) ;
#1677 = CARTESIAN_POINT ( 'NONE',  ( 8.390625000614518214, -3.027376345333610441, -5.243569643749999898 ) ) ;
#1678 = CARTESIAN_POINT ( 'NONE',  ( 3.999999999999998668, 13.30624999877096748, 32.30940107675850470 ) ) ;
#1679 = CARTESIAN_POINT ( 'NONE',  ( 23.75625000122903074, 0.000000000000000000, 4.999999999999998224 ) ) ;
#1680 = CARTESIAN_POINT ( 'NONE',  ( 15.94687500061451502, -3.027376345333614438, 5.243569643749998122 ) ) ;
#1681 = CARTESIAN_POINT ( 'NONE',  ( 45.00000000000000000, 4.500000000000001776, 5.500000000000000000 ) ) ;
#1682 = ORIENTED_EDGE ( 'NONE', *, *, #71265, .T. ) ;
#1683 = CARTESIAN_POINT ( 'NONE',  ( 25.49062500061451786, -3.027376345333610441, -5.243569643749999898 ) ) ;
#1684 = CARTESIAN_POINT ( 'NONE',  ( 10.00312500061451715, 0.000000000000000000, 5.243569643749999010 ) ) ;
#1685 = CARTESIAN_POINT ( 'NONE',  ( 26.25937500061451857, 0.000000000000000000, 5.243569643749999010 ) ) ;
#1686 = CARTESIAN_POINT ( 'NONE',  ( 8.953125000614518214, 4.541064518000418104, -2.621784821874998173 ) ) ;
#1687 = CARTESIAN_POINT ( 'NONE',  ( -4.243569643749998122, 9.996875000614517504, -27.54997392385601174 ) ) ;
#1688 = CARTESIAN_POINT ( 'NONE',  ( 10.50000000122903465, -2.886751345948125991, -5.000000000000000000 ) ) ;
#1689 = CARTESIAN_POINT ( 'NONE',  ( 25.26562500061451289, 3.027376345333611329, 5.243569643749999010 ) ) ;
#1690 = CARTESIAN_POINT ( 'NONE',  ( -4.243569643749999898, 12.60312500061451679, -30.00000000000000000 ) ) ;
#1691 = CARTESIAN_POINT ( 'NONE',  ( 13.76250000122903394, 4.330127018922192761, -2.499999999999997780 ) ) ;
#1692 = CARTESIAN_POINT ( 'NONE',  ( 22.04062500061451502, 6.054752690667223547, 3.707466751127219781E-16 ) ) ;
#1693 = CARTESIAN_POINT ( 'NONE',  ( 11.28749999999999787, -2.886751345948125991, -5.000000000000000000 ) ) ;
#1694 = CARTESIAN_POINT ( 'NONE',  ( 20.27812500061451573, 4.541064518000418104, 2.621784821874999949 ) ) ;
#1695 = PLANE ( 'NONE',  #41938 ) ;
#1696 = CARTESIAN_POINT ( 'NONE',  ( 21.07499999999999929, -4.330127018922194537, 2.499999999999995559 ) ) ;
#1697 = CARTESIAN_POINT ( 'NONE',  ( 13.16250000122903430, -4.330127018922190985, -2.500000000000001332 ) ) ;
#1698 = CARTESIAN_POINT ( 'NONE',  ( 10.26562500061451644, 3.027376345333613106, -5.243569643749998122 ) ) ;
#1699 = CARTESIAN_POINT ( 'NONE',  ( 16.45312500061451289, -4.541064518000417216, -2.621784821875001281 ) ) ;
#1700 = CARTESIAN_POINT ( 'NONE',  ( 24.90000000122903145, -2.886751345948125991, -5.000000000000000000 ) ) ;
#1701 = CARTESIAN_POINT ( 'NONE',  ( 22.54687500061451999, 6.054752690667223547, 3.707466751127219781E-16 ) ) ;
#1702 = CARTESIAN_POINT ( 'NONE',  ( 25.42500000000000071, 4.330127018922191873, 2.499999999999999556 ) ) ;
#1703 = CARTESIAN_POINT ( 'NONE',  ( 8.887500001229033941, 4.330127018922191873, 2.499999999999999556 ) ) ;
#1704 = CARTESIAN_POINT ( 'NONE',  ( 7.696875000614516793, 6.054752690667223547, 3.707466751127219781E-16 ) ) ;
#1705 = CARTESIAN_POINT ( 'NONE',  ( 25.95937500061451431, -4.541064518000417216, -2.621784821875001281 ) ) ;
#1706 = EDGE_CURVE ( 'NONE', #10824, #25563, #71026, .T. ) ;
#1707 = CARTESIAN_POINT ( 'NONE',  ( 3.571875000614517237, 3.027376345333613106, -5.243569643749998122 ) ) ;
#1708 = AXIS2_PLACEMENT_3D ( 'NONE', #36048, #12430, #40884 ) ;
#1709 = CARTESIAN_POINT ( 'NONE',  ( 20.20312500061451644, 4.541064518000418104, -2.621784821874998173 ) ) ;
#1710 = CARTESIAN_POINT ( 'NONE',  ( 25.54687500061451644, -3.027376345333610441, -5.243569643749999898 ) ) ;
#1711 = CARTESIAN_POINT ( 'NONE',  ( -1.878215178125001827, 16.65312499938548285, 33.25316411605952283 ) ) ;
#1712 = CARTESIAN_POINT ( 'NONE',  ( 3.269147239230635549, -3.783209791728578519, 3.521127183980624409 ) ) ;
#1713 = CARTESIAN_POINT ( 'NONE',  ( 7.471875000614519813, -6.054752690667223547, -1.112240025338166033E-15 ) ) ;
#1714 = CARTESIAN_POINT ( 'NONE',  ( 20.16562500061451146, 3.027376345333613106, -5.243569643749998122 ) ) ;
#1715 = CIRCLE ( 'NONE', #52442, 5.999999999999998224 ) ;
#1716 = ORIENTED_EDGE ( 'NONE', *, *, #4157, .T. ) ;
#1717 = CARTESIAN_POINT ( 'NONE',  ( 45.00000000000000000, 0.000000000000000000, 0.000000000000000000 ) ) ;
#1718 = CARTESIAN_POINT ( 'NONE',  ( 26.95312500061451644, 4.541064518000418104, -2.621784821874998173 ) ) ;
#1719 = CARTESIAN_POINT ( 'NONE',  ( 3.871875000614519280, -6.054752690667223547, -1.112240025338166033E-15 ) ) ;
#1720 = DIRECTION ( 'NONE',  ( 0.000000000000000000, 0.000000000000000000, -1.000000000000000000 ) ) ;
#1721 = DIRECTION ( 'NONE',  ( -1.000000000000000000, -0.000000000000000000, -0.000000000000000000 ) ) ;
#1722 = CARTESIAN_POINT ( 'NONE',  ( 17.66249999999999787, 2.886751345948129099, -4.999999999999998224 ) ) ;
#1723 = CARTESIAN_POINT ( 'NONE',  ( 20.46562500061451928, -6.054752690667223547, -1.112240025338166033E-15 ) ) ;
#1724 = VERTEX_POINT ( 'NONE', #60289 ) ;
#1725 = CARTESIAN_POINT ( 'NONE',  ( 25.46249999999999858, 2.886751345948126879, 4.999999999999999112 ) ) ;
#1726 = CARTESIAN_POINT ( 'NONE',  ( 27.15937500061451360, 0.000000000000000000, 5.243569643749999010 ) ) ;
#1727 = ORIENTED_EDGE ( 'NONE', *, *, #16469, .F. ) ;
#1728 = CARTESIAN_POINT ( 'NONE',  ( 13.37812500061451715, 6.421520780324663323E-16, -5.243569643749999010 ) ) ;
#1729 = CARTESIAN_POINT ( 'NONE',  ( 5.353125000614515905, 4.541064518000418104, -2.621784821874998173 ) ) ;
#1730 = CARTESIAN_POINT ( 'NONE',  ( 19.43437500061451573, -2.746126346562646425, 4.756430356249996549 ) ) ;
#1731 = CARTESIAN_POINT ( 'NONE',  ( 28.90312500061451217, 0.000000000000000000, 5.243569643749999010 ) ) ;
#1732 = CARTESIAN_POINT ( 'NONE',  ( 15.75000000122902932, -2.886751345948129988, 4.999999999999997335 ) ) ;
#1733 = CARTESIAN_POINT ( 'NONE',  ( 21.26249999999999574, 2.886751345948129099, -4.999999999999998224 ) ) ;
#1734 = CARTESIAN_POINT ( 'NONE',  ( 28.72500000000000142, -4.330127018922194537, 2.499999999999995559 ) ) ;
#1735 = CARTESIAN_POINT ( 'NONE',  ( 5.071875000614519458, 3.027376345333611329, 5.243569643749999010 ) ) ;
#1736 = CARTESIAN_POINT ( 'NONE',  ( 9.796875000614519990, -3.027376345333610441, -5.243569643749999898 ) ) ;
#1737 = CARTESIAN_POINT ( 'NONE',  ( 18.64687500061451786, -3.027376345333614438, 5.243569643749998122 ) ) ;
#1738 = CARTESIAN_POINT ( 'NONE',  ( 15.71250000122903501, 0.000000000000000000, 4.999999999999998224 ) ) ;
#1739 = ORIENTED_EDGE ( 'NONE', *, *, #12260, .F. ) ;
#1740 = CARTESIAN_POINT ( 'NONE',  ( 29.46562500061451573, -6.054752690667223547, -1.112240025338166033E-15 ) ) ;
#1741 = CARTESIAN_POINT ( 'NONE',  ( 4.237500000000001599, 5.773502691896255534, 3.535250795749688894E-16 ) ) ;
#1743 = EDGE_CURVE ( 'NONE', #59457, #65810, #46732, .T. ) ;
#1742 = CARTESIAN_POINT ( 'NONE',  ( 3.946875000614517681, -3.027376345333610441, -5.243569643749999898 ) ) ;
#1744 = CARTESIAN_POINT ( 'NONE',  ( 19.76250000000000639, -5.773502691896255534, -1.060575238724906372E-15 ) ) ;
#1745 = CARTESIAN_POINT ( 'NONE',  ( 14.65312500061451573, -4.541064518000417216, -2.621784821875001281 ) ) ;
#1746 = CARTESIAN_POINT ( 'NONE',  ( 2.000000000000000444, 19.32500000000000284, 26.53589838486224650 ) ) ;
#1747 = FACE_OUTER_BOUND ( 'NONE', #55151, .T. ) ;
#1748 = CARTESIAN_POINT ( 'NONE',  ( 20.43750000122903643, 6.123233995736764310E-16, -4.999999999999998224 ) ) ;
#1749 = CARTESIAN_POINT ( 'NONE',  ( 19.39687500061451786, 5.492252693125287522, 3.363034840372157021E-16 ) ) ;
#1750 = CARTESIAN_POINT ( 'NONE',  ( 7.078125000614516438, 6.421520780324663323E-16, -5.243569643749999010 ) ) ;
#1751 = CARTESIAN_POINT ( 'NONE',  ( 25.47187500061451715, -6.054752690667223547, -1.112240025338166033E-15 ) ) ;
#1752 = CARTESIAN_POINT ( 'NONE',  ( 4.243569643749999898, 19.63437500061451857, 30.00000000000000000 ) ) ;
#1753 = CARTESIAN_POINT ( 'NONE',  ( 26.59687500061451360, 6.054752690667223547, 3.707466751127219781E-16 ) ) ;
#1754 = CARTESIAN_POINT ( 'NONE',  ( 7.312500000000000000, 2.886751345948129099, -4.999999999999998224 ) ) ;
#1755 = CARTESIAN_POINT ( 'NONE',  ( -1.999999999999997113, 13.43750000122903465, 33.46410161513775705 ) ) ;
#1756 = CARTESIAN_POINT ( 'NONE',  ( 15.74062500061451608, 6.054752690667223547, 3.707466751127219781E-16 ) ) ;
#1757 = CARTESIAN_POINT ( 'NONE',  ( 6.000000001229033764, -2.886751345948125991, -5.000000000000000000 ) ) ;
#1758 = CARTESIAN_POINT ( 'NONE',  ( 18.04687500061451999, 6.054752690667223547, 3.707466751127219781E-16 ) ) ;
#1759 = CARTESIAN_POINT ( 'NONE',  ( 12.53437500061451537, 6.421520780324663323E-16, -5.243569643749999010 ) ) ;
#1760 = CARTESIAN_POINT ( 'NONE',  ( 1.626862140677534470E-15, 13.68124999877096748, 34.00000000000000000 ) ) ;
#1761 = ORIENTED_EDGE ( 'NONE', *, *, #22002, .T. ) ;
#1762 = AXIS2_PLACEMENT_3D ( 'NONE', #29323, #34855, #68483 ) ;
#1763 = CARTESIAN_POINT ( 'NONE',  ( 11.95312500061451644, -4.541064518000417216, -2.621784821875001281 ) ) ;
#1764 = CARTESIAN_POINT ( 'NONE',  ( 29.06250000122903288, 4.330127018922192761, -2.499999999999997780 ) ) ;
#1765 = CARTESIAN_POINT ( 'NONE',  ( 24.56250000122903288, 4.330127018922192761, -2.499999999999997780 ) ) ;
#1766 = CARTESIAN_POINT ( 'NONE',  ( 13.65937500061451715, 0.000000000000000000, 5.243569643749999010 ) ) ;
#1767 = CARTESIAN_POINT ( 'NONE',  ( 14.31562500061451537, 3.027376345333613106, -5.243569643749998122 ) ) ;
#1768 = ADVANCED_FACE ( 'NONE', ( #39607 ), #11520, .F. ) ;
#1769 = CARTESIAN_POINT ( 'NONE',  ( 23.82187500061451502, 3.027376345333613106, -5.243569643749998122 ) ) ;
#1770 = FACE_OUTER_BOUND ( 'NONE', #41782, .T. ) ;
#1771 = AXIS2_PLACEMENT_3D ( 'NONE', #66490, #15503, #3355 ) ;
#1772 = CARTESIAN_POINT ( 'NONE',  ( 11.77500000122903501, -5.773502691896255534, -1.060575238724906372E-15 ) ) ;
#1773 = CARTESIAN_POINT ( 'NONE',  ( 7.500000000000000000, 0.000000000000000000, 4.999999999999998224 ) ) ;
#1774 = CARTESIAN_POINT ( 'NONE',  ( 3.089506346739232967, 3.931278485869285522, -3.469880700456108968 ) ) ;
#1775 = CARTESIAN_POINT ( 'NONE',  ( 4.243569643749999010, 16.52187500061451786, -32.45002607614398471 ) ) ;
#1776 = CARTESIAN_POINT ( 'NONE',  ( 16.80937500061451573, 0.000000000000000000, 5.243569643749999010 ) ) ;
#1777 = CARTESIAN_POINT ( 'NONE',  ( 16.91250000122903430, 4.330127018922192761, -2.499999999999997780 ) ) ;
#1778 = VECTOR ( 'NONE', #42359, 1000.000000000000000 ) ;
#1779 = CARTESIAN_POINT ( 'NONE',  ( 12.83437500061451786, -4.541064518000419881, 2.621784821874995952 ) ) ;
#1780 = CARTESIAN_POINT ( 'NONE',  ( -4.243569643749999898, 19.35312500061451857, -30.00000000000000000 ) ) ;
#1781 = CARTESIAN_POINT ( 'NONE',  ( 19.87500000122903288, -5.773502691896255534, -1.060575238724906372E-15 ) ) ;
#1782 = CARTESIAN_POINT ( 'NONE',  ( 13.82812500061451466, 6.421520780324663323E-16, -5.243569643749999010 ) ) ;
#1783 = VERTEX_POINT ( 'NONE', #51771 ) ;
#1784 = VERTEX_POINT ( 'NONE', #29238 ) ;
#1785 = VECTOR ( 'NONE', #34589, 1000.000000000000000 ) ;
#1786 = CARTESIAN_POINT ( 'NONE',  ( 18.30000000000000071, 0.000000000000000000, 4.999999999999998224 ) ) ;
#1787 = CARTESIAN_POINT ( 'NONE',  ( -5.810221930991193690E-16, 15.50000000122903465, 26.00000000000000355 ) ) ;
#1788 = CARTESIAN_POINT ( 'NONE',  ( 13.02187500061451786, 3.027376345333612662, -5.243569643749998122 ) ) ;
#1789 = CARTESIAN_POINT ( 'NONE',  ( 3.075856135158071769, 3.942005890571277593, -3.420430885948836153 ) ) ;
#1790 = CARTESIAN_POINT ( 'NONE',  ( 15.48750000122903359, 6.123233995736764310E-16, -4.999999999999998224 ) ) ;
#1791 = CARTESIAN_POINT ( 'NONE',  ( 25.80937500061451928, 0.000000000000000000, 5.243569643749999010 ) ) ;
#1792 = CARTESIAN_POINT ( 'NONE',  ( 19.11562500061451431, -6.054752690667223547, -1.112240025338166033E-15 ) ) ;
#1793 =( BOUNDED_CURVE ( )  B_SPLINE_CURVE ( 2, ( #19419, #25716, #26079, #14255, #41979, #64500, #48618 ),
 .UNSPECIFIED., .F., .F. ) 
 B_SPLINE_CURVE_WITH_KNOTS ( ( 3, 2, 2, 3 ),
 ( 0.9772596827842864320, 0.9777777777777777457, 0.9805555555555555136, 0.9810043224607896128 ),
 .UNSPECIFIED. ) 
 CURVE ( )  GEOMETRIC_REPRESENTATION_ITEM ( )  RATIONAL_B_SPLINE_CURVE ( ( 0.9593449661988595611, 0.9750118356804509112, 1.000000000000000000, 0.8660254037844387076, 1.000000000000000000, 0.9783555886274875046, 0.9637047500201995076 ) ) 
 REPRESENTATION_ITEM ( '' )  );
#1794 = CARTESIAN_POINT ( 'NONE',  ( 21.85312500061451502, -4.541064518000417216, -2.621784821875001281 ) ) ;
#1795 = CARTESIAN_POINT ( 'NONE',  ( 3.665625000614517681, 3.027376345333611329, 5.243569643749999010 ) ) ;
#1796 = CARTESIAN_POINT ( 'NONE',  ( 28.57499999999999929, 4.330127018922191873, 2.499999999999999556 ) ) ;
#1797 = CARTESIAN_POINT ( 'NONE',  ( 27.88125000122903074, -4.330127018922194537, 2.499999999999995559 ) ) ;
#1798 = CARTESIAN_POINT ( 'NONE',  ( 9.534375000614517148, 4.119189519843966529, 2.378215178124999607 ) ) ;
#1799 = CARTESIAN_POINT ( 'NONE',  ( 50.00000000000000000, -5.218601775200160553, -7.332543590861066107 ) ) ;
#1800 = CARTESIAN_POINT ( 'NONE',  ( 3.977933236251851579, -3.029199096778425915, -4.197771185803018668 ) ) ;
#1801 = CARTESIAN_POINT ( 'NONE',  ( 9.001249775931846008E-16, 15.02187500061451608, -25.09994784771203058 ) ) ;
#1802 = CARTESIAN_POINT ( 'NONE',  ( 4.087500001229035007, -4.330127018922194537, 2.499999999999995559 ) ) ;
#1803 = CARTESIAN_POINT ( 'NONE',  ( 6.712500000000000355, -5.773502691896255534, -1.060575238724906372E-15 ) ) ;
#1804 = EDGE_CURVE ( 'NONE', #71417, #44451, #9952, .T. ) ;
#1805 = CARTESIAN_POINT ( 'NONE',  ( 3.015379517359913386, -4.298692091864810827, -3.041586178295606846 ) ) ;
#1806 = CARTESIAN_POINT ( 'NONE',  ( 9.384375000614518569, 6.421520780324663323E-16, -5.243569643749999010 ) ) ;
#1807 = CARTESIAN_POINT ( 'NONE',  ( 28.82812500061451644, 4.541064518000418104, 2.621784821874999949 ) ) ;
#1808 = DIRECTION ( 'NONE',  ( -1.000000000000000000, -0.000000000000000000, -0.000000000000000000 ) ) ;
#1809 = VECTOR ( 'NONE', #70709, 1000.000000000000000 ) ;
#1810 = DIRECTION ( 'NONE',  ( -0.000000000000000000, -1.000000000000000000, -0.000000000000000000 ) ) ;
#1811 = CARTESIAN_POINT ( 'NONE',  ( 7.021875000614518747, -6.054752690667223547, -1.112240025338166033E-15 ) ) ;
#1812 = CARTESIAN_POINT ( 'NONE',  ( 11.14687500061451608, -3.027376345333610441, -5.243569643749999898 ) ) ;
#1813 = CARTESIAN_POINT ( 'NONE',  ( 7.275000000000000355, 6.123233995736764310E-16, -4.999999999999998224 ) ) ;
#1814 = VECTOR ( 'NONE', #48157, 1000.000000000000000 ) ;
#1815 = CARTESIAN_POINT ( 'NONE',  ( -2.121784821874999949, 15.67812500061459247, 26.32496088578401938 ) ) ;
#1816 = CARTESIAN_POINT ( 'NONE',  ( 0.5273506787484333325, 25.53584304230190938, 33.97379189798129318 ) ) ;
#1817 = CARTESIAN_POINT ( 'NONE',  ( 5.625000000000001776, 4.330127018922191873, 2.499999999999999556 ) ) ;
#1818 = CARTESIAN_POINT ( 'NONE',  ( 14.48437500061451644, -2.746126346562646425, 4.756430356249996549 ) ) ;
#1819 = CARTESIAN_POINT ( 'NONE',  ( 21.85312500061451502, -4.541064518000417216, -2.621784821875001281 ) ) ;
#1820 = CARTESIAN_POINT ( 'NONE',  ( 13.34062500061451750, -3.027376345333610441, -5.243569643749999898 ) ) ;
#1821 = CARTESIAN_POINT ( 'NONE',  ( 25.20937500061451431, 2.746126346562643317, 4.756430356249998326 ) ) ;
#1822 = CARTESIAN_POINT ( 'NONE',  ( 10.50937500061451679, 0.000000000000000000, 5.243569643749999010 ) ) ;
#1823 = CARTESIAN_POINT ( 'NONE',  ( 26.43750000000000000, -2.886751345948129988, 4.999999999999997335 ) ) ;
#1824 = CARTESIAN_POINT ( 'NONE',  ( 22.31250000122903288, 4.330127018922192761, -2.499999999999997780 ) ) ;
#1825 = CARTESIAN_POINT ( 'NONE',  ( 11.97187500061451892, -6.054752690667223547, -1.112240025338166033E-15 ) ) ;
#1826 = CARTESIAN_POINT ( 'NONE',  ( 27.60937500061451644, 0.000000000000000000, 5.243569643749999010 ) ) ;
#1827 = CARTESIAN_POINT ( 'NONE',  ( 4.209375000614516971, 0.000000000000000000, 5.243569643749999010 ) ) ;
#1828 = CARTESIAN_POINT ( 'NONE',  ( -1.071796769724475906, 12.82009619066136707, -34.00000000000000711 ) ) ;
#1829 = CARTESIAN_POINT ( 'NONE',  ( 19.73437500061451644, 6.421520780324663323E-16, -5.243569643749999010 ) ) ;
#1830 =( BOUNDED_CURVE ( )  B_SPLINE_CURVE ( 2, ( #4171, #10790, #50685, #88, #22593, #38878, #55498, #61397, #4537 ),
 .UNSPECIFIED., .F., .F. ) 
 B_SPLINE_CURVE_WITH_KNOTS ( ( 3, 2, 2, 2, 3 ),
 ( 0.9027777777777777901, 0.9074074074074074403, 0.9166666666666666297, 0.9259259259259259300, 0.9305555555555555802 ),
 .UNSPECIFIED. ) 
 CURVE ( )  GEOMETRIC_REPRESENTATION_ITEM ( )  RATIONAL_B_SPLINE_CURVE ( ( 0.9330127018922194093, 0.9330127018922194093, 1.000000000000000000, 0.8660254037844387076, 1.000000000000000000, 0.8660254037844387076, 1.000000000000000000, 0.9330127018922194093, 0.9330127018922194093 ) ) 
 REPRESENTATION_ITEM ( '' )  );
#1831 = CARTESIAN_POINT ( 'NONE',  ( 11.59687500061451892, -3.027376345333610441, -5.243569643749999898 ) ) ;
#1832 = CARTESIAN_POINT ( 'NONE',  ( 3.756430356250000102, 17.70312499938548356, 30.00000000000000000 ) ) ;
#1833 = CARTESIAN_POINT ( 'NONE',  ( 25.42500000000000071, 4.330127018922191873, 2.499999999999999556 ) ) ;
#1834 = CARTESIAN_POINT ( 'NONE',  ( -8.484601909799255319E-16, 13.73749999999999893, 34.61880215351700940 ) ) ;
#1835 = CARTESIAN_POINT ( 'NONE',  ( -3.000416591977282496E-16, 11.19687500061451679, -34.90005215228797653 ) ) ;
#1836 = CARTESIAN_POINT ( 'NONE',  ( 27.30937500061451573, -4.119189519843965641, -2.378215178125001383 ) ) ;
#1837 = CARTESIAN_POINT ( 'NONE',  ( 14.69062500061451537, -3.027376345333610441, -5.243569643749999898 ) ) ;
#1838 = CARTESIAN_POINT ( 'NONE',  ( 5.549999999999998934, 4.330127018922192761, -2.499999999999997780 ) ) ;
#1839 = CARTESIAN_POINT ( 'NONE',  ( 65.00000000000000000, 0.000000000000000000, 0.000000000000000000 ) ) ;
#1840 = CARTESIAN_POINT ( 'NONE',  ( 45.00000000000000000, 5.218601775200101045, -7.332543590861111404 ) ) ;
#1841 =( BOUNDED_SURFACE ( )  B_SPLINE_SURFACE ( 1, 2, ( 
 ( #61791, #35169, #11915, #23710, #68800, #63240, #126, #45182, #18156, #844, #45902, #52164, #12634, #67713, #11196, #39646, #67361, #23353, #7098, #22987, #40356, #40003, #6012, #39279, #1567, #33722, #17085, #56968, #22631, #56267, #5658, #62875, #28194, #62164, #68433, #28547, #51802, #51081, #478, #45547, #68077, #17446, #62517, #6372, #17796, #12271, #34802, #57334, #6738, #8920, #7457, #29984, #35528, #18525, #52886, #47703, #19243, #70607, #36620, #30712, #24439, #69166, #41090, #18882, #41445, #52526, #2284, #63963, #36260, #59141, #63602, #3389, #25162, #47344, #30357, #53992, #12992, #31450, #1934, #58775, #42533, #46988, #8184, #25538, #53245, #14080, #3008, #8550, #48079, #24801, #64696, #65059, #69524, #19613, #14450, #58049, #13347, #69878, #31077, #35884, #58409, #53617, #19980, #2643, #41798, #36984, #7822, #59506, #64326, #13719, #42170, #70242, #46623, #48450, #26275, #20349, #38455, #66527, #70974, #55449, #55086, #27376, #32912, #15907, #60981, #66906, #71342, #72432, #37716, #10380, #31818, #4842, #20717, #9650, #43275, #4120, #15538, #44005, #72069, #48812, #15177, #49908, #49547, #32184, #65796, #21816, #65424, #44381, #54357, #21449, #42900, #14814, #59879, #60236, #37357, #54717, #26649, #71715, #16274, #38830, #61345, #3751, #9285, #49185, #55813, #60604, #10741, #21087, #33274, #43638, #66162, #38082, #25910, #10013, #32549, #4486, #27015, #68713, #67275, #756, #40634, #63153, #11103, #16634, #46174, #29184, #33631, #17711, #39, #62076, #50635, #56529, #67987, #23264, #51353, #5569, #67627, #57242, #28815, #11469, #28106, #6655, #44741, #51717, #56176, #45814, #27741, #39189, #61704, #22544, #72804, #45092, #16993, #50991, #68350, #1119, #18073, #39551, #6285, #33992, #62792, #23628, #5922, #28456, #12185, #389, #12548, #50280, #35082, #22896, #45455, #22187, #17361, #5200, #39918, #62432, #11830, #34348, #56881, #40271, #34712, #8462, #47622, #41715, #35439, #7011, #52078, #29902, #52441, #63519, #13263, #1847, #47261, #70154, #29542, #14368, #36174, #58323, #41362, #64977, #1483, #19902, #41004, #69795, #53530, #12906, #19161, #36537, #64241, #25079, #13998, #19532, #59057, #63872, #2559, #2925, #57963, #30630, #25455, #23989, #24355, #35801, #42090, #46536, #7371, #64612, #30997, #13630, #7734, #69078, #47999, #46902, #53162, #18439, #69441, #18798, #30269, #52802, #2203, #24718, #58691, #70527, #42454, #57608, #8102, #37999, #48365, #21367, #55367, #70891, #15096, #43921, #71252, #21732, #59423, #44292, #14729, #25828, #53908, #8831, #72351, #20264, #42816, #65339, #31367, #43190, #60521, #9565, #60893, #26934, #21002, #37271, #3301, #59793, #9199, #31734, #54272, #65710, #3666, #26560, #49459, #26189, #66821, #15454, #37632, #20631, #36903, #48729, #60155, #32097, #49100, #32829, #54629, #71629, #15824, #43554, #4405, #66447, #71993, #38367, #4036, #54999, #4760, #66076, #9927, #27293, #32465, #10298, #49827, #676, #55728, #22103, #34266, #28732, #5842, #39466, #34632, #61265, #17634, #27656, #61988, #11749, #28374, #50194, #38745, #16552, #10659, #51273, #56799, #33189, #45737, #45371, #40194, #23183, #6204, #68272, #57161, #44661, #5122, #6573, #62715, #67191, #12109, #11023, #73081, #61620, #67548, #50911, #29104, #62353, #39104, #5486, #51639, #39839, #22462, #33545, #1040, #45012, #23547, #72720, #46097, #56095, #309, #16194, #28025, #22819, #50553, #67906, #16911, #11389, #33908, #56452, #17277, #13545, #64527, #1401, #41638, #13921, #63072, #40928, #52359, #53081, #35003, #23910, #36092, #8019, #58246, #18720, #36459, #40554, #70073, #6933, #41284, #64157, #7651, #29464, #17995, #68996, #12474, #30555, #58612, #57533, #25001, #24637, #19447, #2476, #47544, #42007, #58974, #46458, #52000, #8381, #30911, #18355, #53452, #63441, #1763, #12827, #46825, #30189, #2842, #25371, #35361, #57885, #68633, #19083, #24276, #7294, #29824, #69362, #63795, #13185, #35724, #52719, #2126, #47183, #69715, #42372, #48281, #70805, #20542, #65995, #49380, #60806, #14284, #49014, #59336, #32375, #66364, #8747, #26106, #54915, #9116, #32747, #70444, #55285, #25744, #36821, #64894, #19820, #10214, #31280, #53822, #3215, #20180, #54187, #71546, #43100, #71910, #37918, #32014, #42735, #65254, #14644, #37185, #59709, #31654, #3584, #48645, #37551, #60436, #71170, #4679, #26474, #65626, #15013, #21284, #60073, #9485, #43471, #54549, #3951, #20919, #15376, #9846, #4322, #26847, #43837, #15739, #38278, #47915, #34184, #17196, #39756, #68188, #33105, #16109, #17552, #51190, #55644, #62274, #22020, #10939, #72636, #5402, #16832, #45289, #231, #27575, #16465, #6121, #50831, #33462, #50107, #28651, #66738, #594, #5039, #22738, #49744, #38660, #61183, #44576, #21649, #67109, #39024, #72998, #67823, #23098, #40113, #10578, #28296, #61538, #11668, #45656, #56008, #27938, #56719, #50471, #12023, #72272, #34547, #22382, #44931, #44206, #67469, #62628, #39385, #61904, #11309, #33830, #56373, #57076, #5765, #27209, #69626, #63704, #57442, #29019, #956, #51913, #1311, #12378, #35274, #23820, #69269, #18988, #51554, #36367, #58156, #7204, #63353, #13827, #23464, #41910, #62983, #18631, #2389, #34915, #41196, #58516, #13096, #47093, #35997, #41550, #7926, #12737, #24548, #24907, #6845, #52631, #47451, #46010, #46371, #57795, #64067, #68547, #29380, #13448, #30463, #35634, #29733, #69983, #7560, #68905, #52271, #18262, #52993, #19353, #40836, #1673, #17906, #64435, #40468, #24182, #46735, #6484, #30095, #2037, #21468, #16651, #67293, #31186, #20085, #4504, #42642, #8656, #53728, #25650, #3121, #47819, #61362, #65166, #58882, #8292, #19726, #48187, #44758, #38847, #10031, #27033, #66924, #53355, #15924, #15555, #10759, #70711, #60998, #30823, #25272, #36726 ),
 ( #49564, #32566, #5217, #2753, #33291, #70350, #55104, #55467, #72085, #42277, #64800, #59248, #14191, #72449, #27393, #38099, #16292, #38474, #55829, #27758, #49925, #21834, #50299, #60621, #44022, #72821, #22204, #66545, #44398, #10397, #32929, #4859, #17377, #28831, #57258, #12201, #39568, #28473, #18088, #62808, #45472, #62093, #40649, #5587, #63169, #45109, #34729, #61721, #28124, #56, #34009, #33649, #11486, #56546, #11846, #6671, #12564, #52093, #50652, #23643, #57623, #22562, #39934, #46189, #406, #24004, #11120, #46552, #17011, #67645, #56193, #5939, #1498, #51009, #22915, #68004, #62448, #34365, #40287, #56897, #35098, #29199, #23280, #6303, #51370, #772, #45830, #68366, #17728, #51733, #1134, #68728, #7026, #29557, #69093, #39207, #19174, #2219, #25842, #12921, #53921, #1862, #8117, #14382, #46917, #53176, #70540, #2574, #59072, #48012, #8476, #19915, #24732, #36552, #36917, #24369, #64626, #59437, #35454, #63886, #47276, #2939, #57978, #69455, #31010, #53543, #30645, #41729, #8845, #63534, #42469, #29916, #64256, #14013, #25093, #52456, #41019, #18813, #7386, #25468, #64992, #41376, #31381, #47636, #3315, #48379, #18455, #13277, #35815, #58337, #7748, #30284, #52817, #69809, #13644, #36188, #58706, #70170, #19546, #42104, #15837, #43934, #71268, #60168, #49840, #21380, #4048, #20646, #72364, #37286, #21745, #3681, #66460, #20278, #59809, #31750, #65723, #65354, #43203, #15109, #43568, #38383, #44307, #10672, #9214, #72005, #54287, #37645, #14744, #38759, #15467, #27306, #4773, #66836, #26205, #48744, #16207, #32479, #49473, #55741, #61279, #9578, #32110, #54644, #27669, #55013, #33202, #26574, #60906, #66089, #49113, #42831, #5135, #70906, #71642, #38012, #21015, #60534, #9941, #10310, #4418, #26947, #32842, #55379, #50567, #51286, #39479, #34280, #33558, #11763, #6946, #45026, #73094, #6219, #688, #28747, #56812, #46109, #16566, #72732, #23195, #56108, #67561, #50926, #67920, #11035, #28038, #5499, #45749, #33923, #62366, #17291, #22832, #34647, #11403, #29118, #40567, #63087, #68285, #39853, #22476, #323, #16925, #57175, #23563, #62002, #45384, #44674, #6588, #22118, #56465, #5856, #40206, #51652, #28387, #17646, #50208, #57544, #62728, #12121, #1053, #68646, #18009, #12488, #35015, #67205, #39118, #61633, #13198, #59349, #29477, #63455, #18732, #14297, #8394, #52733, #69726, #36470, #23922, #58625, #35737, #53464, #46837, #30567, #1415, #69009, #7306, #30923, #41296, #2855, #58257, #69376, #19095, #63806, #7662, #64907, #30202, #2138, #29837, #53093, #24649, #13558, #12841, #64170, #52014, #24289, #52372, #8032, #2488, #25013, #36104, #25384, #18373, #46472, #47555, #35375, #47195, #41650, #70084, #57898, #1777, #19459, #42019, #64540, #13933, #58988, #47928, #70457, #19833, #42385, #36835, #40941, #60450, #71557, #31666, #32025, #26118, #15752, #55297, #48657, #54561, #3229, #38291, #53835, #14655, #54199, #71922, #60818, #15026, #43484, #38675, #16121, #3596, #43112, #26486, #65638, #71182, #20555, #37563, #60086, #70819, #10226, #9496, #8760, #31294, #42747, #3963, #66751, #32760, #49027, #20932, #4691, #25757, #37930, #66008, #27221, #15388, #9858, #48293, #20193, #59721, #49757, #32387, #72284, #54926, #4335, #26860, #49391, #21297, #43850, #65267, #21662, #66376, #44219, #37198, #9129, #67123, #39037, #12038, #22753, #39773, #46027, #40129, #61551, #5052, #33474, #17921, #45304, #34563, #16845, #34200, #33844, #50486, #10591, #29035, #970, #10953, #28308, #44590, #51570, #50121, #56734, #23480, #61918, #5778, #22033, #56023, #16479, #62289, #44944, #244, #50845, #56388, #45670, #22396, #62643, #68563, #61196, #11685, #67838, #5414, #11323, #27954, #68206, #57091, #73011, #17211, #55656, #17567, #33119, #67482, #39399, #51208, #6500, #6137, #28667, #27589, #72652, #608, #23114, #58171, #24197, #63370, #12754, #7220, #35289, #29395, #41926, #46751, #70366, #40484, #1326, #29749, #25291, #19368, #63719, #7576, #47466, #34931, #69641, #69285, #64452, #57811, #41564, #12394, #6862, #18277, #13843, #52287, #36382, #18648, #1688, #30111, #41211, #13111, #35650, #57457, #8307, #52645, #69999, #58897, #30838, #46386, #40852, #53371, #2052, #19003, #47836, #2768, #24563, #51929, #47109, #63000, #64082, #23836, #13464, #36013, #58531, #7941, #68920, #30480, #53008, #2403, #24924, #3138, #10141, #8672, #15302, #55213, #4608, #9045, #48569, #20102, #20845, #31575, #3875, #25667, #54477, #49672, #14573, #42658, #48940, #43398, #71469, #26398, #15665, #59263, #42293, #65922, #48204, #37106, #31203, #53744, #59632, #14207, #65182, #54114, #65552, #37841, #21210, #32673, #70726, #60361, #3511, #4246, #38204, #26031, #71096, #26773, #20470, #27138, #64817, #19744, #43024, #14942, #36743, #37480, #60000, #9410, #31940, #9771, #32304, #54839, #49305, #71839, #43762, #66287, #60730, #4968, #21578, #44132, #72561, #50035, #33034, #10865, #21947, #22310, #28228, #66659, #23028, #61830, #55934, #38952, #517, #16036, #28583, #10506, #44862, #34115, #55573, #67399, #17123, #16760, #50758, #67751, #161, #39682, #61470, #5692, #56654, #27501, #56303, #6049, #38584, #44504, #33398, #22667, #61109, #67037, #45217, #62202, #39318, #5330, #51120, #16397, #11598, #27871, #50403, #72199, #72928, #11235, #33758, #65406, #59489, #4468, #32531, #36967, #21431, #21070, #66509, #72052, #55067, #26998, #32892, #70957, #53973, #55432, #15890, #20330, #49528, #59862, #48795, #37339, #43256, #54698, #9996, #38063, #14796, #54339, #43988, #15521, #71323, #9266, #38436, #31433, #60962, #42883, #60587, #14432, #4103, #10361, #8901, #21796, #43621, #65777, #20698, #72414, #3371, #27358, #48432, #26630, #4824, #31801, #49167, #49889, #71698, #65042, #25892, #3733, #26258, #15159 ) ),
 .UNSPECIFIED., .F., .F., .F. ) 
 B_SPLINE_SURFACE_WITH_KNOTS ( ( 2, 2 ),
 ( 3, 2, 2, 2, 2, 2, 2, 2, 2, 2, 2, 2, 2, 2, 2, 2, 2, 2, 2, 2, 2, 2, 2, 2, 2, 2, 2, 2, 2, 2, 2, 2, 2, 2, 2, 2, 2, 2, 2, 2, 2, 2, 2, 2, 2, 2, 2, 2, 2, 2, 2, 2, 2, 2, 2, 2, 2, 2, 2, 2, 2, 2, 2, 2, 2, 2, 2, 2, 2, 2, 2, 2, 2, 2, 2, 2, 2, 2, 2, 2, 2, 2, 2, 2, 2, 2, 2, 2, 2, 2, 2, 2, 2, 2, 2, 2, 2, 2, 2, 2, 2, 2, 2, 2, 2, 2, 2, 2, 2, 2, 2, 2, 2, 2, 2, 2, 2, 2, 2, 2, 2, 2, 2, 2, 2, 2, 2, 2, 2, 2, 2, 2, 2, 2, 2, 2, 2, 2, 2, 2, 2, 2, 2, 2, 2, 2, 2, 2, 2, 2, 2, 2, 2, 2, 2, 2, 2, 2, 2, 2, 2, 2, 2, 2, 2, 2, 2, 2, 2, 2, 2, 2, 2, 2, 2, 2, 2, 2, 2, 2, 2, 2, 2, 2, 2, 2, 2, 2, 2, 2, 2, 2, 2, 2, 2, 2, 2, 2, 2, 2, 2, 2, 2, 2, 2, 2, 2, 2, 2, 2, 2, 2, 2, 2, 2, 2, 2, 2, 2, 2, 2, 2, 2, 2, 2, 2, 2, 2, 2, 2, 2, 2, 2, 2, 2, 2, 2, 2, 2, 2, 2, 2, 2, 2, 2, 2, 2, 2, 2, 2, 2, 2, 2, 2, 2, 2, 2, 2, 2, 2, 2, 2, 2, 2, 2, 2, 2, 2, 2, 2, 2, 2, 2, 2, 2, 2, 2, 2, 2, 2, 2, 2, 2, 2, 2, 2, 2, 2, 2, 2, 2, 2, 2, 2, 2, 2, 2, 2, 2, 2, 2, 2, 2, 2, 2, 2, 2, 2, 2, 2, 2, 2, 2, 2, 2, 2, 2, 2, 2, 2, 2, 2, 2, 2, 2, 2, 2, 2, 2, 2, 2, 2, 2, 2, 2, 2, 2, 2, 2, 2, 2, 2, 2, 2, 2, 2, 2, 2, 2, 2, 2, 2, 2, 2, 2, 2, 2, 2, 2, 2, 3 ),
 ( 0.000000000000000000, 1.000000000000000000 ),
 ( 0.000000000000000000, 0.002777777777777777884, 0.005555555555555555768, 0.008333333333333333218, 0.01111111111111111154, 0.01388888888888888812, 0.01666666666666666644, 0.01944444444444444475, 0.02222222222222222307, 0.02500000000000000139, 0.02777777777777777624, 0.03055555555555555455, 0.03333333333333333287, 0.03611111111111110772, 0.03888888888888888951, 0.04166666666666666435, 0.04444444444444444614, 0.04722222222222222099, 0.05000000000000000278, 0.05277777777777777762, 0.05555555555555555247, 0.05833333333333333426, 0.06111111111111110911, 0.06388888888888888395, 0.06666666666666666574, 0.06944444444444444753, 0.07222222222222221544, 0.07499999999999999722, 0.07777777777777777901, 0.08055555555555556080, 0.08333333333333332871, 0.08611111111111111049, 0.08888888888888889228, 0.09166666666666666019, 0.09444444444444444198, 0.09722222222222222376, 0.1000000000000000056, 0.1027777777777777735, 0.1055555555555555552, 0.1083333333333333370, 0.1111111111111111049, 0.1138888888888888867, 0.1166666666666666685, 0.1194444444444444503, 0.1222222222222222182, 0.1250000000000000000, 0.1277777777777777679, 0.1305555555555555636, 0.1333333333333333315, 0.1361111111111110994, 0.1388888888888888951, 0.1416666666666666630, 0.1444444444444444309, 0.1472222222222222265, 0.1499999999999999944, 0.1527777777777777901, 0.1555555555555555580, 0.1583333333333333259, 0.1611111111111111216, 0.1638888888888888895, 0.1666666666666666574, 0.1694444444444444531, 0.1722222222222222210, 0.1749999999999999889, 0.1777777777777777846, 0.1805555555555555525, 0.1833333333333333204, 0.1861111111111111160, 0.1888888888888888840, 0.1916666666666666796, 0.1944444444444444475, 0.1972222222222222154, 0.2000000000000000111, 0.2027777777777777790, 0.2055555555555555469, 0.2083333333333333426, 0.2111111111111111105, 0.2138888888888888784, 0.2166666666666666741, 0.2194444444444444420, 0.2222222222222222099, 0.2250000000000000056, 0.2277777777777777735, 0.2305555555555555691, 0.2333333333333333370, 0.2361111111111111049, 0.2388888888888889006, 0.2416666666666666685, 0.2444444444444444364, 0.2472222222222222321, 0.2500000000000000000, 0.2527777777777777679, 0.2555555555555555358, 0.2583333333333333592, 0.2611111111111111271, 0.2638888888888888951, 0.2666666666666666630, 0.2694444444444444309, 0.2722222222222221988, 0.2750000000000000222, 0.2777777777777777901, 0.2805555555555555580, 0.2833333333333333259, 0.2861111111111110938, 0.2888888888888888618, 0.2916666666666666852, 0.2944444444444444531, 0.2972222222222222210, 0.2999999999999999889, 0.3027777777777777568, 0.3055555555555555802, 0.3083333333333333481, 0.3111111111111111160, 0.3138888888888888840, 0.3166666666666666519, 0.3194444444444444198, 0.3222222222222222432, 0.3250000000000000111, 0.3277777777777777790, 0.3305555555555555469, 0.3333333333333333148, 0.3361111111111111382, 0.3388888888888889062, 0.3416666666666666741, 0.3444444444444444420, 0.3472222222222222099, 0.3499999999999999778, 0.3527777777777778012, 0.3555555555555555691, 0.3583333333333333370, 0.3611111111111111049, 0.3638888888888888729, 0.3666666666666666408, 0.3694444444444444642, 0.3722222222222222321, 0.3750000000000000000, 0.3777777777777777679, 0.3805555555555555358, 0.3833333333333333592, 0.3861111111111111271, 0.3888888888888888951, 0.3916666666666666630, 0.3944444444444444309, 0.3972222222222221988, 0.4000000000000000222, 0.4027777777777777901, 0.4055555555555555580, 0.4083333333333333259, 0.4111111111111110938, 0.4138888888888888618, 0.4166666666666666852, 0.4194444444444444531, 0.4222222222222222210, 0.4249999999999999889, 0.4277777777777777568, 0.4305555555555555802, 0.4333333333333333481, 0.4361111111111111160, 0.4388888888888888840, 0.4416666666666666519, 0.4444444444444444198, 0.4472222222222222432, 0.4500000000000000111, 0.4527777777777777790, 0.4555555555555555469, 0.4583333333333333148, 0.4611111111111111382, 0.4638888888888889062, 0.4666666666666666741, 0.4694444444444444420, 0.4722222222222222099, 0.4749999999999999778, 0.4777777777777778012, 0.4805555555555555691, 0.4833333333333333370, 0.4861111111111111049, 0.4888888888888888729, 0.4916666666666666408, 0.4944444444444444642, 0.4972222222222222321, 0.5000000000000000000, 0.5027777777777777679, 0.5055555555555555358, 0.5083333333333333037, 0.5111111111111110716, 0.5138888888888888395, 0.5166666666666667185, 0.5194444444444444864, 0.5222222222222222543, 0.5250000000000000222, 0.5277777777777777901, 0.5305555555555555580, 0.5333333333333333259, 0.5361111111111110938, 0.5388888888888888618, 0.5416666666666666297, 0.5444444444444443976, 0.5472222222222222765, 0.5500000000000000444, 0.5527777777777778123, 0.5555555555555555802, 0.5583333333333333481, 0.5611111111111111160, 0.5638888888888888840, 0.5666666666666666519, 0.5694444444444444198, 0.5722222222222221877, 0.5749999999999999556, 0.5777777777777777235, 0.5805555555555556024, 0.5833333333333333703, 0.5861111111111111382, 0.5888888888888889062, 0.5916666666666666741, 0.5944444444444444420, 0.5972222222222222099, 0.5999999999999999778, 0.6027777777777777457, 0.6055555555555555136, 0.6083333333333332815, 0.6111111111111111605, 0.6138888888888889284, 0.6166666666666666963, 0.6194444444444444642, 0.6222222222222222321, 0.6250000000000000000, 0.6277777777777777679, 0.6305555555555555358, 0.6333333333333333037, 0.6361111111111110716, 0.6388888888888888395, 0.6416666666666667185, 0.6444444444444444864, 0.6472222222222222543, 0.6500000000000000222, 0.6527777777777777901, 0.6555555555555555580, 0.6583333333333333259, 0.6611111111111110938, 0.6638888888888888618, 0.6666666666666666297, 0.6694444444444443976, 0.6722222222222222765, 0.6750000000000000444, 0.6777777777777778123, 0.6805555555555555802, 0.6833333333333333481, 0.6861111111111111160, 0.6888888888888888840, 0.6916666666666666519, 0.6944444444444444198, 0.6972222222222221877, 0.6999999999999999556, 0.7027777777777777235, 0.7055555555555556024, 0.7083333333333333703, 0.7111111111111111382, 0.7138888888888889062, 0.7166666666666666741, 0.7194444444444444420, 0.7222222222222222099, 0.7249999999999999778, 0.7277777777777777457, 0.7305555555555555136, 0.7333333333333332815, 0.7361111111111111605, 0.7388888888888889284, 0.7416666666666666963, 0.7444444444444444642, 0.7472222222222222321, 0.7500000000000000000, 0.7527777777777777679, 0.7555555555555555358, 0.7583333333333333037, 0.7611111111111110716, 0.7638888888888888395, 0.7666666666666667185, 0.7694444444444444864, 0.7722222222222222543, 0.7750000000000000222, 0.7777777777777777901, 0.7805555555555555580, 0.7833333333333333259, 0.7861111111111110938, 0.7888888888888888618, 0.7916666666666666297, 0.7944444444444443976, 0.7972222222222222765, 0.8000000000000000444, 0.8027777777777778123, 0.8055555555555555802, 0.8083333333333333481, 0.8111111111111111160, 0.8138888888888888840, 0.8166666666666666519, 0.8194444444444444198, 0.8222222222222221877, 0.8249999999999999556, 0.8277777777777777235, 0.8305555555555556024, 0.8333333333333333703, 0.8361111111111111382, 0.8388888888888889062, 0.8416666666666666741, 0.8444444444444444420, 0.8472222222222222099, 0.8499999999999999778, 0.8527777777777777457, 0.8555555555555555136, 0.8583333333333332815, 0.8611111111111111605, 0.8638888888888889284, 0.8666666666666666963, 0.8694444444444444642, 0.8722222222222222321, 0.8750000000000000000, 0.8777777777777777679, 0.8805555555555555358, 0.8833333333333333037, 0.8861111111111110716, 0.8888888888888888395, 0.8916666666666667185, 0.8944444444444444864, 0.8972222222222222543, 0.9000000000000000222, 0.9027777777777777901, 0.9055555555555555580, 0.9083333333333333259, 0.9111111111111110938, 0.9138888888888888618, 0.9166666666666666297, 0.9194444444444443976, 0.9222222222222222765, 0.9250000000000000444, 0.9277777777777778123, 0.9305555555555555802, 0.9333333333333333481, 0.9361111111111111160, 0.9388888888888888840, 0.9416666666666666519, 0.9444444444444444198, 0.9472222222222221877, 0.9499999999999999556, 0.9527777777777777235, 0.9555555555555556024, 0.9583333333333333703, 0.9611111111111111382, 0.9638888888888889062, 0.9666666666666666741, 0.9694444444444444420, 0.9722222222222222099, 0.9749999999999999778, 0.9777777777777777457, 0.9805555555555555136, 0.9833333333333332815, 0.9861111111111111605, 0.9888888888888889284, 0.9916666666666666963, 0.9944444444444444642, 0.9972222222222222321, 1.000000000000000000 ),
 .UNSPECIFIED. ) 
 GEOMETRIC_REPRESENTATION_ITEM ( )  RATIONAL_B_SPLINE_SURFACE ( (
 ( 1.000000000000000000, 0.8660254037844387076, 1.000000000000000000, 0.8660254037844387076, 1.000000000000000000, 0.8660254037844387076, 1.000000000000000000, 0.8660254037844387076, 1.000000000000000000, 0.8660254037844387076, 1.000000000000000000, 0.8660254037844387076, 1.000000000000000000, 0.8660254037844387076, 1.000000000000000000, 0.8660254037844387076, 1.000000000000000000, 0.8660254037844387076, 1.000000000000000000, 0.8660254037844387076, 1.000000000000000000, 0.8660254037844387076, 1.000000000000000000, 0.8660254037844387076, 1.000000000000000000, 0.8660254037844387076, 1.000000000000000000, 0.8660254037844387076, 1.000000000000000000, 0.8660254037844387076, 1.000000000000000000, 0.8660254037844387076, 1.000000000000000000, 0.8660254037844387076, 1.000000000000000000, 0.8660254037844387076, 1.000000000000000000, 0.8660254037844387076, 1.000000000000000000, 0.8660254037844387076, 1.000000000000000000, 0.8660254037844387076, 1.000000000000000000, 0.8660254037844387076, 1.000000000000000000, 0.8660254037844387076, 1.000000000000000000, 0.8660254037844387076, 1.000000000000000000, 0.8660254037844387076, 1.000000000000000000, 0.8660254037844387076, 1.000000000000000000, 0.8660254037844387076, 1.000000000000000000, 0.8660254037844387076, 1.000000000000000000, 0.8660254037844387076, 1.000000000000000000, 0.8660254037844387076, 1.000000000000000000, 0.8660254037844387076, 1.000000000000000000, 0.8660254037844387076, 1.000000000000000000, 0.8660254037844387076, 1.000000000000000000, 0.8660254037844387076, 1.000000000000000000, 0.8660254037844387076, 1.000000000000000000, 0.8660254037844387076, 1.000000000000000000, 0.8660254037844387076, 1.000000000000000000, 0.8660254037844387076, 1.000000000000000000, 0.8660254037844387076, 1.000000000000000000, 0.8660254037844387076, 1.000000000000000000, 0.8660254037844387076, 1.000000000000000000, 0.8660254037844387076, 1.000000000000000000, 0.8660254037844387076, 1.000000000000000000, 0.8660254037844387076, 1.000000000000000000, 0.8660254037844387076, 1.000000000000000000, 0.8660254037844387076, 1.000000000000000000, 0.8660254037844387076, 1.000000000000000000, 0.8660254037844387076, 1.000000000000000000, 0.8660254037844387076, 1.000000000000000000, 0.8660254037844387076, 1.000000000000000000, 0.8660254037844387076, 1.000000000000000000, 0.8660254037844387076, 1.000000000000000000, 0.8660254037844387076, 1.000000000000000000, 0.8660254037844387076, 1.000000000000000000, 0.8660254037844387076, 1.000000000000000000, 0.8660254037844387076, 1.000000000000000000, 0.8660254037844387076, 1.000000000000000000, 0.8660254037844387076, 1.000000000000000000, 0.8660254037844387076, 1.000000000000000000, 0.8660254037844387076, 1.000000000000000000, 0.8660254037844387076, 1.000000000000000000, 0.8660254037844387076, 1.000000000000000000, 0.8660254037844387076, 1.000000000000000000, 0.8660254037844387076, 1.000000000000000000, 0.8660254037844387076, 1.000000000000000000, 0.8660254037844387076, 1.000000000000000000, 0.8660254037844387076, 1.000000000000000000, 0.8660254037844387076, 1.000000000000000000, 0.8660254037844387076, 1.000000000000000000, 0.8660254037844387076, 1.000000000000000000, 0.8660254037844387076, 1.000000000000000000, 0.8660254037844387076, 1.000000000000000000, 0.8660254037844387076, 1.000000000000000000, 0.8660254037844387076, 1.000000000000000000, 0.8660254037844387076, 1.000000000000000000, 0.8660254037844387076, 1.000000000000000000, 0.8660254037844387076, 1.000000000000000000, 0.8660254037844387076, 1.000000000000000000, 0.8660254037844387076, 1.000000000000000000, 0.8660254037844387076, 1.000000000000000000, 0.8660254037844387076, 1.000000000000000000, 0.8660254037844387076, 1.000000000000000000, 0.8660254037844387076, 1.000000000000000000, 0.8660254037844387076, 1.000000000000000000, 0.8660254037844387076, 1.000000000000000000, 0.8660254037844387076, 1.000000000000000000, 0.8660254037844387076, 1.000000000000000000, 0.8660254037844387076, 1.000000000000000000, 0.8660254037844387076, 1.000000000000000000, 0.8660254037844387076, 1.000000000000000000, 0.8660254037844387076, 1.000000000000000000, 0.8660254037844387076, 1.000000000000000000, 0.8660254037844387076, 1.000000000000000000, 0.8660254037844387076, 1.000000000000000000, 0.8660254037844387076, 1.000000000000000000, 0.8660254037844387076, 1.000000000000000000, 0.8660254037844387076, 1.000000000000000000, 0.8660254037844387076, 1.000000000000000000, 0.8660254037844387076, 1.000000000000000000, 0.8660254037844387076, 1.000000000000000000, 0.8660254037844387076, 1.000000000000000000, 0.8660254037844387076, 1.000000000000000000, 0.8660254037844387076, 1.000000000000000000, 0.8660254037844387076, 1.000000000000000000, 0.8660254037844387076, 1.000000000000000000, 0.8660254037844387076, 1.000000000000000000, 0.8660254037844387076, 1.000000000000000000, 0.8660254037844387076, 1.000000000000000000, 0.8660254037844387076, 1.000000000000000000, 0.8660254037844387076, 1.000000000000000000, 0.8660254037844387076, 1.000000000000000000, 0.8660254037844387076, 1.000000000000000000, 0.8660254037844387076, 1.000000000000000000, 0.8660254037844387076, 1.000000000000000000, 0.8660254037844387076, 1.000000000000000000, 0.8660254037844387076, 1.000000000000000000, 0.8660254037844387076, 1.000000000000000000, 0.8660254037844387076, 1.000000000000000000, 0.8660254037844387076, 1.000000000000000000, 0.8660254037844387076, 1.000000000000000000, 0.8660254037844387076, 1.000000000000000000, 0.8660254037844387076, 1.000000000000000000, 0.8660254037844387076, 1.000000000000000000, 0.8660254037844387076, 1.000000000000000000, 0.8660254037844387076, 1.000000000000000000, 0.8660254037844387076, 1.000000000000000000, 0.8660254037844387076, 1.000000000000000000, 0.8660254037844387076, 1.000000000000000000, 0.8660254037844387076, 1.000000000000000000, 0.8660254037844387076, 1.000000000000000000, 0.8660254037844387076, 1.000000000000000000, 0.8660254037844387076, 1.000000000000000000, 0.8660254037844387076, 1.000000000000000000, 0.8660254037844387076, 1.000000000000000000, 0.8660254037844387076, 1.000000000000000000, 0.8660254037844387076, 1.000000000000000000, 0.8660254037844387076, 1.000000000000000000, 0.8660254037844387076, 1.000000000000000000, 0.8660254037844387076, 1.000000000000000000, 0.8660254037844387076, 1.000000000000000000, 0.8660254037844387076, 1.000000000000000000, 0.8660254037844387076, 1.000000000000000000, 0.8660254037844387076, 1.000000000000000000, 0.8660254037844387076, 1.000000000000000000, 0.8660254037844387076, 1.000000000000000000, 0.8660254037844387076, 1.000000000000000000, 0.8660254037844387076, 1.000000000000000000, 0.8660254037844387076, 1.000000000000000000, 0.8660254037844387076, 1.000000000000000000, 0.8660254037844387076, 1.000000000000000000, 0.8660254037844387076, 1.000000000000000000, 0.8660254037844387076, 1.000000000000000000, 0.8660254037844387076, 1.000000000000000000, 0.8660254037844387076, 1.000000000000000000, 0.8660254037844387076, 1.000000000000000000, 0.8660254037844387076, 1.000000000000000000, 0.8660254037844387076, 1.000000000000000000, 0.8660254037844387076, 1.000000000000000000, 0.8660254037844387076, 1.000000000000000000, 0.8660254037844387076, 1.000000000000000000, 0.8660254037844387076, 1.000000000000000000, 0.8660254037844387076, 1.000000000000000000, 0.8660254037844387076, 1.000000000000000000, 0.8660254037844387076, 1.000000000000000000, 0.8660254037844387076, 1.000000000000000000, 0.8660254037844387076, 1.000000000000000000, 0.8660254037844387076, 1.000000000000000000, 0.8660254037844387076, 1.000000000000000000, 0.8660254037844387076, 1.000000000000000000, 0.8660254037844387076, 1.000000000000000000, 0.8660254037844387076, 1.000000000000000000, 0.8660254037844387076, 1.000000000000000000, 0.8660254037844387076, 1.000000000000000000, 0.8660254037844387076, 1.000000000000000000, 0.8660254037844387076, 1.000000000000000000, 0.8660254037844387076, 1.000000000000000000, 0.8660254037844387076, 1.000000000000000000, 0.8660254037844387076, 1.000000000000000000, 0.8660254037844387076, 1.000000000000000000, 0.8660254037844387076, 1.000000000000000000, 0.8660254037844387076, 1.000000000000000000, 0.8660254037844387076, 1.000000000000000000, 0.8660254037844387076, 1.000000000000000000, 0.8660254037844387076, 1.000000000000000000, 0.8660254037844387076, 1.000000000000000000, 0.8660254037844387076, 1.000000000000000000, 0.8660254037844387076, 1.000000000000000000, 0.8660254037844387076, 1.000000000000000000, 0.8660254037844387076, 1.000000000000000000, 0.8660254037844387076, 1.000000000000000000, 0.8660254037844387076, 1.000000000000000000, 0.8660254037844387076, 1.000000000000000000, 0.8660254037844387076, 1.000000000000000000, 0.8660254037844387076, 1.000000000000000000, 0.8660254037844387076, 1.000000000000000000, 0.8660254037844387076, 1.000000000000000000, 0.8660254037844387076, 1.000000000000000000, 0.8660254037844387076, 1.000000000000000000, 0.8660254037844387076, 1.000000000000000000, 0.8660254037844387076, 1.000000000000000000, 0.8660254037844387076, 1.000000000000000000, 0.8660254037844387076, 1.000000000000000000, 0.8660254037844387076, 1.000000000000000000, 0.8660254037844387076, 1.000000000000000000, 0.8660254037844387076, 1.000000000000000000, 0.8660254037844387076, 1.000000000000000000, 0.8660254037844387076, 1.000000000000000000, 0.8660254037844387076, 1.000000000000000000, 0.8660254037844387076, 1.000000000000000000, 0.8660254037844387076, 1.000000000000000000, 0.8660254037844387076, 1.000000000000000000, 0.8660254037844387076, 1.000000000000000000, 0.8660254037844387076, 1.000000000000000000, 0.8660254037844387076, 1.000000000000000000, 0.8660254037844387076, 1.000000000000000000, 0.8660254037844387076, 1.000000000000000000, 0.8660254037844387076, 1.000000000000000000, 0.8660254037844387076, 1.000000000000000000, 0.8660254037844387076, 1.000000000000000000, 0.8660254037844387076, 1.000000000000000000, 0.8660254037844387076, 1.000000000000000000, 0.8660254037844387076, 1.000000000000000000, 0.8660254037844387076, 1.000000000000000000, 0.8660254037844387076, 1.000000000000000000, 0.8660254037844387076, 1.000000000000000000, 0.8660254037844387076, 1.000000000000000000, 0.8660254037844387076, 1.000000000000000000, 0.8660254037844387076, 1.000000000000000000, 0.8660254037844387076, 1.000000000000000000, 0.8660254037844387076, 1.000000000000000000, 0.8660254037844387076, 1.000000000000000000, 0.8660254037844387076, 1.000000000000000000, 0.8660254037844387076, 1.000000000000000000, 0.8660254037844387076, 1.000000000000000000, 0.8660254037844387076, 1.000000000000000000, 0.8660254037844387076, 1.000000000000000000, 0.8660254037844387076, 1.000000000000000000, 0.8660254037844387076, 1.000000000000000000, 0.8660254037844387076, 1.000000000000000000, 0.8660254037844387076, 1.000000000000000000, 0.8660254037844387076, 1.000000000000000000, 0.8660254037844387076, 1.000000000000000000, 0.8660254037844387076, 1.000000000000000000, 0.8660254037844387076, 1.000000000000000000, 0.8660254037844387076, 1.000000000000000000, 0.8660254037844387076, 1.000000000000000000, 0.8660254037844387076, 1.000000000000000000, 0.8660254037844387076, 1.000000000000000000, 0.8660254037844387076, 1.000000000000000000, 0.8660254037844387076, 1.000000000000000000, 0.8660254037844387076, 1.000000000000000000, 0.8660254037844387076, 1.000000000000000000, 0.8660254037844387076, 1.000000000000000000, 0.8660254037844387076, 1.000000000000000000, 0.8660254037844387076, 1.000000000000000000, 0.8660254037844387076, 1.000000000000000000, 0.8660254037844387076, 1.000000000000000000, 0.8660254037844387076, 1.000000000000000000, 0.8660254037844387076, 1.000000000000000000, 0.8660254037844387076, 1.000000000000000000, 0.8660254037844387076, 1.000000000000000000, 0.8660254037844387076, 1.000000000000000000, 0.8660254037844387076, 1.000000000000000000, 0.8660254037844387076, 1.000000000000000000, 0.8660254037844387076, 1.000000000000000000, 0.8660254037844387076, 1.000000000000000000, 0.8660254037844387076, 1.000000000000000000, 0.8660254037844387076, 1.000000000000000000, 0.8660254037844387076, 1.000000000000000000, 0.8660254037844387076, 1.000000000000000000, 0.8660254037844387076, 1.000000000000000000, 0.8660254037844387076, 1.000000000000000000, 0.8660254037844387076, 1.000000000000000000, 0.8660254037844387076, 1.000000000000000000, 0.8660254037844387076, 1.000000000000000000, 0.8660254037844387076, 1.000000000000000000, 0.8660254037844387076, 1.000000000000000000, 0.8660254037844387076, 1.000000000000000000, 0.8660254037844387076, 1.000000000000000000, 0.8660254037844387076, 1.000000000000000000, 0.8660254037844387076, 1.000000000000000000, 0.8660254037844387076, 1.000000000000000000, 0.8660254037844387076, 1.000000000000000000, 0.8660254037844387076, 1.000000000000000000, 0.8660254037844387076, 1.000000000000000000, 0.8660254037844387076, 1.000000000000000000, 0.8660254037844387076, 1.000000000000000000, 0.8660254037844387076, 1.000000000000000000, 0.8660254037844387076, 1.000000000000000000, 0.8660254037844387076, 1.000000000000000000, 0.8660254037844387076, 1.000000000000000000, 0.8660254037844387076, 1.000000000000000000, 0.8660254037844387076, 1.000000000000000000, 0.8660254037844387076, 1.000000000000000000, 0.8660254037844387076, 1.000000000000000000, 0.8660254037844387076, 1.000000000000000000, 0.8660254037844387076, 1.000000000000000000, 0.8660254037844387076, 1.000000000000000000, 0.8660254037844387076, 1.000000000000000000, 0.8660254037844387076, 1.000000000000000000, 0.8660254037844387076, 1.000000000000000000, 0.8660254037844387076, 1.000000000000000000, 0.8660254037844387076, 1.000000000000000000, 0.8660254037844387076, 1.000000000000000000, 0.8660254037844387076, 1.000000000000000000, 0.8660254037844387076, 1.000000000000000000, 0.8660254037844387076, 1.000000000000000000, 0.8660254037844387076, 1.000000000000000000, 0.8660254037844387076, 1.000000000000000000, 0.8660254037844387076, 1.000000000000000000, 0.8660254037844387076, 1.000000000000000000, 0.8660254037844387076, 1.000000000000000000, 0.8660254037844387076, 1.000000000000000000, 0.8660254037844387076, 1.000000000000000000, 0.8660254037844387076, 1.000000000000000000, 0.8660254037844387076, 1.000000000000000000, 0.8660254037844387076, 1.000000000000000000, 0.8660254037844387076, 1.000000000000000000, 0.8660254037844387076, 1.000000000000000000, 0.8660254037844387076, 1.000000000000000000, 0.8660254037844387076, 1.000000000000000000, 0.8660254037844387076, 1.000000000000000000, 0.8660254037844387076, 1.000000000000000000, 0.8660254037844387076, 1.000000000000000000, 0.8660254037844387076, 1.000000000000000000, 0.8660254037844387076, 1.000000000000000000, 0.8660254037844387076, 1.000000000000000000, 0.8660254037844387076, 1.000000000000000000, 0.8660254037844387076, 1.000000000000000000, 0.8660254037844387076, 1.000000000000000000, 0.8660254037844387076, 1.000000000000000000, 0.8660254037844387076, 1.000000000000000000, 0.8660254037844387076, 1.000000000000000000, 0.8660254037844387076, 1.000000000000000000, 0.8660254037844387076, 1.000000000000000000, 0.8660254037844387076, 1.000000000000000000, 0.8660254037844387076, 1.000000000000000000, 0.8660254037844387076, 1.000000000000000000, 0.8660254037844387076, 1.000000000000000000, 0.8660254037844387076, 1.000000000000000000, 0.8660254037844387076, 1.000000000000000000, 0.8660254037844387076, 1.000000000000000000, 0.8660254037844387076, 1.000000000000000000, 0.8660254037844387076, 1.000000000000000000, 0.8660254037844387076, 1.000000000000000000, 0.8660254037844387076, 1.000000000000000000, 0.8660254037844387076, 1.000000000000000000, 0.8660254037844387076, 1.000000000000000000, 0.8660254037844387076, 1.000000000000000000, 0.8660254037844387076, 1.000000000000000000, 0.8660254037844387076, 1.000000000000000000, 0.8660254037844387076, 1.000000000000000000, 0.8660254037844387076, 1.000000000000000000, 0.8660254037844387076, 1.000000000000000000, 0.8660254037844387076, 1.000000000000000000, 0.8660254037844387076, 1.000000000000000000, 0.8660254037844387076, 1.000000000000000000, 0.8660254037844387076, 1.000000000000000000, 0.8660254037844387076, 1.000000000000000000, 0.8660254037844387076, 1.000000000000000000),
 ( 1.000000000000000000, 0.8660254037844387076, 1.000000000000000000, 0.8660254037844387076, 1.000000000000000000, 0.8660254037844387076, 1.000000000000000000, 0.8660254037844387076, 1.000000000000000000, 0.8660254037844387076, 1.000000000000000000, 0.8660254037844387076, 1.000000000000000000, 0.8660254037844387076, 1.000000000000000000, 0.8660254037844387076, 1.000000000000000000, 0.8660254037844387076, 1.000000000000000000, 0.8660254037844387076, 1.000000000000000000, 0.8660254037844387076, 1.000000000000000000, 0.8660254037844387076, 1.000000000000000000, 0.8660254037844387076, 1.000000000000000000, 0.8660254037844387076, 1.000000000000000000, 0.8660254037844387076, 1.000000000000000000, 0.8660254037844387076, 1.000000000000000000, 0.8660254037844387076, 1.000000000000000000, 0.8660254037844387076, 1.000000000000000000, 0.8660254037844387076, 1.000000000000000000, 0.8660254037844387076, 1.000000000000000000, 0.8660254037844387076, 1.000000000000000000, 0.8660254037844387076, 1.000000000000000000, 0.8660254037844387076, 1.000000000000000000, 0.8660254037844387076, 1.000000000000000000, 0.8660254037844387076, 1.000000000000000000, 0.8660254037844387076, 1.000000000000000000, 0.8660254037844387076, 1.000000000000000000, 0.8660254037844387076, 1.000000000000000000, 0.8660254037844387076, 1.000000000000000000, 0.8660254037844387076, 1.000000000000000000, 0.8660254037844387076, 1.000000000000000000, 0.8660254037844387076, 1.000000000000000000, 0.8660254037844387076, 1.000000000000000000, 0.8660254037844387076, 1.000000000000000000, 0.8660254037844387076, 1.000000000000000000, 0.8660254037844387076, 1.000000000000000000, 0.8660254037844387076, 1.000000000000000000, 0.8660254037844387076, 1.000000000000000000, 0.8660254037844387076, 1.000000000000000000, 0.8660254037844387076, 1.000000000000000000, 0.8660254037844387076, 1.000000000000000000, 0.8660254037844387076, 1.000000000000000000, 0.8660254037844387076, 1.000000000000000000, 0.8660254037844387076, 1.000000000000000000, 0.8660254037844387076, 1.000000000000000000, 0.8660254037844387076, 1.000000000000000000, 0.8660254037844387076, 1.000000000000000000, 0.8660254037844387076, 1.000000000000000000, 0.8660254037844387076, 1.000000000000000000, 0.8660254037844387076, 1.000000000000000000, 0.8660254037844387076, 1.000000000000000000, 0.8660254037844387076, 1.000000000000000000, 0.8660254037844387076, 1.000000000000000000, 0.8660254037844387076, 1.000000000000000000, 0.8660254037844387076, 1.000000000000000000, 0.8660254037844387076, 1.000000000000000000, 0.8660254037844387076, 1.000000000000000000, 0.8660254037844387076, 1.000000000000000000, 0.8660254037844387076, 1.000000000000000000, 0.8660254037844387076, 1.000000000000000000, 0.8660254037844387076, 1.000000000000000000, 0.8660254037844387076, 1.000000000000000000, 0.8660254037844387076, 1.000000000000000000, 0.8660254037844387076, 1.000000000000000000, 0.8660254037844387076, 1.000000000000000000, 0.8660254037844387076, 1.000000000000000000, 0.8660254037844387076, 1.000000000000000000, 0.8660254037844387076, 1.000000000000000000, 0.8660254037844387076, 1.000000000000000000, 0.8660254037844387076, 1.000000000000000000, 0.8660254037844387076, 1.000000000000000000, 0.8660254037844387076, 1.000000000000000000, 0.8660254037844387076, 1.000000000000000000, 0.8660254037844387076, 1.000000000000000000, 0.8660254037844387076, 1.000000000000000000, 0.8660254037844387076, 1.000000000000000000, 0.8660254037844387076, 1.000000000000000000, 0.8660254037844387076, 1.000000000000000000, 0.8660254037844387076, 1.000000000000000000, 0.8660254037844387076, 1.000000000000000000, 0.8660254037844387076, 1.000000000000000000, 0.8660254037844387076, 1.000000000000000000, 0.8660254037844387076, 1.000000000000000000, 0.8660254037844387076, 1.000000000000000000, 0.8660254037844387076, 1.000000000000000000, 0.8660254037844387076, 1.000000000000000000, 0.8660254037844387076, 1.000000000000000000, 0.8660254037844387076, 1.000000000000000000, 0.8660254037844387076, 1.000000000000000000, 0.8660254037844387076, 1.000000000000000000, 0.8660254037844387076, 1.000000000000000000, 0.8660254037844387076, 1.000000000000000000, 0.8660254037844387076, 1.000000000000000000, 0.8660254037844387076, 1.000000000000000000, 0.8660254037844387076, 1.000000000000000000, 0.8660254037844387076, 1.000000000000000000, 0.8660254037844387076, 1.000000000000000000, 0.8660254037844387076, 1.000000000000000000, 0.8660254037844387076, 1.000000000000000000, 0.8660254037844387076, 1.000000000000000000, 0.8660254037844387076, 1.000000000000000000, 0.8660254037844387076, 1.000000000000000000, 0.8660254037844387076, 1.000000000000000000, 0.8660254037844387076, 1.000000000000000000, 0.8660254037844387076, 1.000000000000000000, 0.8660254037844387076, 1.000000000000000000, 0.8660254037844387076, 1.000000000000000000, 0.8660254037844387076, 1.000000000000000000, 0.8660254037844387076, 1.000000000000000000, 0.8660254037844387076, 1.000000000000000000, 0.8660254037844387076, 1.000000000000000000, 0.8660254037844387076, 1.000000000000000000, 0.8660254037844387076, 1.000000000000000000, 0.8660254037844387076, 1.000000000000000000, 0.8660254037844387076, 1.000000000000000000, 0.8660254037844387076, 1.000000000000000000, 0.8660254037844387076, 1.000000000000000000, 0.8660254037844387076, 1.000000000000000000, 0.8660254037844387076, 1.000000000000000000, 0.8660254037844387076, 1.000000000000000000, 0.8660254037844387076, 1.000000000000000000, 0.8660254037844387076, 1.000000000000000000, 0.8660254037844387076, 1.000000000000000000, 0.8660254037844387076, 1.000000000000000000, 0.8660254037844387076, 1.000000000000000000, 0.8660254037844387076, 1.000000000000000000, 0.8660254037844387076, 1.000000000000000000, 0.8660254037844387076, 1.000000000000000000, 0.8660254037844387076, 1.000000000000000000, 0.8660254037844387076, 1.000000000000000000, 0.8660254037844387076, 1.000000000000000000, 0.8660254037844387076, 1.000000000000000000, 0.8660254037844387076, 1.000000000000000000, 0.8660254037844387076, 1.000000000000000000, 0.8660254037844387076, 1.000000000000000000, 0.8660254037844387076, 1.000000000000000000, 0.8660254037844387076, 1.000000000000000000, 0.8660254037844387076, 1.000000000000000000, 0.8660254037844387076, 1.000000000000000000, 0.8660254037844387076, 1.000000000000000000, 0.8660254037844387076, 1.000000000000000000, 0.8660254037844387076, 1.000000000000000000, 0.8660254037844387076, 1.000000000000000000, 0.8660254037844387076, 1.000000000000000000, 0.8660254037844387076, 1.000000000000000000, 0.8660254037844387076, 1.000000000000000000, 0.8660254037844387076, 1.000000000000000000, 0.8660254037844387076, 1.000000000000000000, 0.8660254037844387076, 1.000000000000000000, 0.8660254037844387076, 1.000000000000000000, 0.8660254037844387076, 1.000000000000000000, 0.8660254037844387076, 1.000000000000000000, 0.8660254037844387076, 1.000000000000000000, 0.8660254037844387076, 1.000000000000000000, 0.8660254037844387076, 1.000000000000000000, 0.8660254037844387076, 1.000000000000000000, 0.8660254037844387076, 1.000000000000000000, 0.8660254037844387076, 1.000000000000000000, 0.8660254037844387076, 1.000000000000000000, 0.8660254037844387076, 1.000000000000000000, 0.8660254037844387076, 1.000000000000000000, 0.8660254037844387076, 1.000000000000000000, 0.8660254037844387076, 1.000000000000000000, 0.8660254037844387076, 1.000000000000000000, 0.8660254037844387076, 1.000000000000000000, 0.8660254037844387076, 1.000000000000000000, 0.8660254037844387076, 1.000000000000000000, 0.8660254037844387076, 1.000000000000000000, 0.8660254037844387076, 1.000000000000000000, 0.8660254037844387076, 1.000000000000000000, 0.8660254037844387076, 1.000000000000000000, 0.8660254037844387076, 1.000000000000000000, 0.8660254037844387076, 1.000000000000000000, 0.8660254037844387076, 1.000000000000000000, 0.8660254037844387076, 1.000000000000000000, 0.8660254037844387076, 1.000000000000000000, 0.8660254037844387076, 1.000000000000000000, 0.8660254037844387076, 1.000000000000000000, 0.8660254037844387076, 1.000000000000000000, 0.8660254037844387076, 1.000000000000000000, 0.8660254037844387076, 1.000000000000000000, 0.8660254037844387076, 1.000000000000000000, 0.8660254037844387076, 1.000000000000000000, 0.8660254037844387076, 1.000000000000000000, 0.8660254037844387076, 1.000000000000000000, 0.8660254037844387076, 1.000000000000000000, 0.8660254037844387076, 1.000000000000000000, 0.8660254037844387076, 1.000000000000000000, 0.8660254037844387076, 1.000000000000000000, 0.8660254037844387076, 1.000000000000000000, 0.8660254037844387076, 1.000000000000000000, 0.8660254037844387076, 1.000000000000000000, 0.8660254037844387076, 1.000000000000000000, 0.8660254037844387076, 1.000000000000000000, 0.8660254037844387076, 1.000000000000000000, 0.8660254037844387076, 1.000000000000000000, 0.8660254037844387076, 1.000000000000000000, 0.8660254037844387076, 1.000000000000000000, 0.8660254037844387076, 1.000000000000000000, 0.8660254037844387076, 1.000000000000000000, 0.8660254037844387076, 1.000000000000000000, 0.8660254037844387076, 1.000000000000000000, 0.8660254037844387076, 1.000000000000000000, 0.8660254037844387076, 1.000000000000000000, 0.8660254037844387076, 1.000000000000000000, 0.8660254037844387076, 1.000000000000000000, 0.8660254037844387076, 1.000000000000000000, 0.8660254037844387076, 1.000000000000000000, 0.8660254037844387076, 1.000000000000000000, 0.8660254037844387076, 1.000000000000000000, 0.8660254037844387076, 1.000000000000000000, 0.8660254037844387076, 1.000000000000000000, 0.8660254037844387076, 1.000000000000000000, 0.8660254037844387076, 1.000000000000000000, 0.8660254037844387076, 1.000000000000000000, 0.8660254037844387076, 1.000000000000000000, 0.8660254037844387076, 1.000000000000000000, 0.8660254037844387076, 1.000000000000000000, 0.8660254037844387076, 1.000000000000000000, 0.8660254037844387076, 1.000000000000000000, 0.8660254037844387076, 1.000000000000000000, 0.8660254037844387076, 1.000000000000000000, 0.8660254037844387076, 1.000000000000000000, 0.8660254037844387076, 1.000000000000000000, 0.8660254037844387076, 1.000000000000000000, 0.8660254037844387076, 1.000000000000000000, 0.8660254037844387076, 1.000000000000000000, 0.8660254037844387076, 1.000000000000000000, 0.8660254037844387076, 1.000000000000000000, 0.8660254037844387076, 1.000000000000000000, 0.8660254037844387076, 1.000000000000000000, 0.8660254037844387076, 1.000000000000000000, 0.8660254037844387076, 1.000000000000000000, 0.8660254037844387076, 1.000000000000000000, 0.8660254037844387076, 1.000000000000000000, 0.8660254037844387076, 1.000000000000000000, 0.8660254037844387076, 1.000000000000000000, 0.8660254037844387076, 1.000000000000000000, 0.8660254037844387076, 1.000000000000000000, 0.8660254037844387076, 1.000000000000000000, 0.8660254037844387076, 1.000000000000000000, 0.8660254037844387076, 1.000000000000000000, 0.8660254037844387076, 1.000000000000000000, 0.8660254037844387076, 1.000000000000000000, 0.8660254037844387076, 1.000000000000000000, 0.8660254037844387076, 1.000000000000000000, 0.8660254037844387076, 1.000000000000000000, 0.8660254037844387076, 1.000000000000000000, 0.8660254037844387076, 1.000000000000000000, 0.8660254037844387076, 1.000000000000000000, 0.8660254037844387076, 1.000000000000000000, 0.8660254037844387076, 1.000000000000000000, 0.8660254037844387076, 1.000000000000000000, 0.8660254037844387076, 1.000000000000000000, 0.8660254037844387076, 1.000000000000000000, 0.8660254037844387076, 1.000000000000000000, 0.8660254037844387076, 1.000000000000000000, 0.8660254037844387076, 1.000000000000000000, 0.8660254037844387076, 1.000000000000000000, 0.8660254037844387076, 1.000000000000000000, 0.8660254037844387076, 1.000000000000000000, 0.8660254037844387076, 1.000000000000000000, 0.8660254037844387076, 1.000000000000000000, 0.8660254037844387076, 1.000000000000000000, 0.8660254037844387076, 1.000000000000000000, 0.8660254037844387076, 1.000000000000000000, 0.8660254037844387076, 1.000000000000000000, 0.8660254037844387076, 1.000000000000000000, 0.8660254037844387076, 1.000000000000000000, 0.8660254037844387076, 1.000000000000000000, 0.8660254037844387076, 1.000000000000000000, 0.8660254037844387076, 1.000000000000000000, 0.8660254037844387076, 1.000000000000000000, 0.8660254037844387076, 1.000000000000000000, 0.8660254037844387076, 1.000000000000000000, 0.8660254037844387076, 1.000000000000000000, 0.8660254037844387076, 1.000000000000000000, 0.8660254037844387076, 1.000000000000000000, 0.8660254037844387076, 1.000000000000000000, 0.8660254037844387076, 1.000000000000000000, 0.8660254037844387076, 1.000000000000000000, 0.8660254037844387076, 1.000000000000000000, 0.8660254037844387076, 1.000000000000000000, 0.8660254037844387076, 1.000000000000000000, 0.8660254037844387076, 1.000000000000000000, 0.8660254037844387076, 1.000000000000000000, 0.8660254037844387076, 1.000000000000000000, 0.8660254037844387076, 1.000000000000000000, 0.8660254037844387076, 1.000000000000000000, 0.8660254037844387076, 1.000000000000000000, 0.8660254037844387076, 1.000000000000000000, 0.8660254037844387076, 1.000000000000000000, 0.8660254037844387076, 1.000000000000000000, 0.8660254037844387076, 1.000000000000000000, 0.8660254037844387076, 1.000000000000000000, 0.8660254037844387076, 1.000000000000000000, 0.8660254037844387076, 1.000000000000000000, 0.8660254037844387076, 1.000000000000000000, 0.8660254037844387076, 1.000000000000000000, 0.8660254037844387076, 1.000000000000000000, 0.8660254037844387076, 1.000000000000000000, 0.8660254037844387076, 1.000000000000000000, 0.8660254037844387076, 1.000000000000000000, 0.8660254037844387076, 1.000000000000000000, 0.8660254037844387076, 1.000000000000000000, 0.8660254037844387076, 1.000000000000000000, 0.8660254037844387076, 1.000000000000000000, 0.8660254037844387076, 1.000000000000000000, 0.8660254037844387076, 1.000000000000000000, 0.8660254037844387076, 1.000000000000000000, 0.8660254037844387076, 1.000000000000000000, 0.8660254037844387076, 1.000000000000000000, 0.8660254037844387076, 1.000000000000000000, 0.8660254037844387076, 1.000000000000000000, 0.8660254037844387076, 1.000000000000000000, 0.8660254037844387076, 1.000000000000000000, 0.8660254037844387076, 1.000000000000000000, 0.8660254037844387076, 1.000000000000000000, 0.8660254037844387076, 1.000000000000000000, 0.8660254037844387076, 1.000000000000000000, 0.8660254037844387076, 1.000000000000000000, 0.8660254037844387076, 1.000000000000000000, 0.8660254037844387076, 1.000000000000000000, 0.8660254037844387076, 1.000000000000000000, 0.8660254037844387076, 1.000000000000000000, 0.8660254037844387076, 1.000000000000000000, 0.8660254037844387076, 1.000000000000000000, 0.8660254037844387076, 1.000000000000000000, 0.8660254037844387076, 1.000000000000000000, 0.8660254037844387076, 1.000000000000000000, 0.8660254037844387076, 1.000000000000000000, 0.8660254037844387076, 1.000000000000000000, 0.8660254037844387076, 1.000000000000000000, 0.8660254037844387076, 1.000000000000000000, 0.8660254037844387076, 1.000000000000000000, 0.8660254037844387076, 1.000000000000000000, 0.8660254037844387076, 1.000000000000000000, 0.8660254037844387076, 1.000000000000000000, 0.8660254037844387076, 1.000000000000000000, 0.8660254037844387076, 1.000000000000000000, 0.8660254037844387076, 1.000000000000000000, 0.8660254037844387076, 1.000000000000000000, 0.8660254037844387076, 1.000000000000000000, 0.8660254037844387076, 1.000000000000000000, 0.8660254037844387076, 1.000000000000000000, 0.8660254037844387076, 1.000000000000000000, 0.8660254037844387076, 1.000000000000000000, 0.8660254037844387076, 1.000000000000000000, 0.8660254037844387076, 1.000000000000000000, 0.8660254037844387076, 1.000000000000000000, 0.8660254037844387076, 1.000000000000000000, 0.8660254037844387076, 1.000000000000000000, 0.8660254037844387076, 1.000000000000000000, 0.8660254037844387076, 1.000000000000000000, 0.8660254037844387076, 1.000000000000000000, 0.8660254037844387076, 1.000000000000000000, 0.8660254037844387076, 1.000000000000000000, 0.8660254037844387076, 1.000000000000000000, 0.8660254037844387076, 1.000000000000000000, 0.8660254037844387076, 1.000000000000000000) ) ) 
 REPRESENTATION_ITEM ( '' )  SURFACE ( )  );
#1842 = CARTESIAN_POINT ( 'NONE',  ( 15.03749999999999964, 5.773502691896255534, 3.535250795749688894E-16 ) ) ;
#1843 = CARTESIAN_POINT ( 'NONE',  ( 4.243569643749999898, 10.12812500061451715, 30.00000000000000000 ) ) ;
#1844 = CARTESIAN_POINT ( 'NONE',  ( 14.77500000122903501, 2.886751345948126879, 4.999999999999999112 ) ) ;
#1845 = CARTESIAN_POINT ( 'NONE',  ( 24.49687500061451573, -3.027376345333614438, 5.243569643749998122 ) ) ;
#1846 = VERTEX_POINT ( 'NONE', #34042 ) ;
#1847 = CARTESIAN_POINT ( 'NONE',  ( 20.39062500061451644, -3.027376345333614438, 5.243569643749998122 ) ) ;
#1848 = CARTESIAN_POINT ( 'NONE',  ( 19.73437500061451644, 6.421520780324663323E-16, -5.243569643749999010 ) ) ;
#1849 = CARTESIAN_POINT ( 'NONE',  ( 4.949999999999999289, -4.330127018922190985, -2.500000000000001332 ) ) ;
#1850 = CARTESIAN_POINT ( 'NONE',  ( 8.240625000614516082, -3.027376345333614438, 5.243569643749998122 ) ) ;
#1851 = CARTESIAN_POINT ( 'NONE',  ( 21.92812500061451431, 6.421520780324663323E-16, -5.243569643749999010 ) ) ;
#1852 = EDGE_CURVE ( 'NONE', #15973, #9585, #41547, .T. ) ;
#1853 = CARTESIAN_POINT ( 'NONE',  ( 15.75937500061451857, 4.541064518000418104, -2.621784821874998173 ) ) ;
#1854 = CARTESIAN_POINT ( 'NONE',  ( 4.243569643749999898, 14.59062500061451750, 32.45002607614398471 ) ) ;
#1855 = CARTESIAN_POINT ( 'NONE',  ( 18.63750000122903216, 6.123233995736764310E-16, -4.999999999999998224 ) ) ;
#1856 = CARTESIAN_POINT ( 'NONE',  ( 11.63437500061451857, 5.824947211148865298E-16, -4.756430356249998326 ) ) ;
#1857 = CARTESIAN_POINT ( 'NONE',  ( 8.353125000614518569, -4.541064518000417216, -2.621784821875001281 ) ) ;
#1858 = CARTESIAN_POINT ( 'NONE',  ( 13.79999999999999893, 0.000000000000000000, 4.999999999999998224 ) ) ;
#1859 = CARTESIAN_POINT ( 'NONE',  ( 3.084375000614519191, 6.421520780324663323E-16, -5.243569643749999010 ) ) ;
#1860 = CARTESIAN_POINT ( 'NONE',  ( 25.47187500061451715, -6.054752690667223547, -1.112240025338166033E-15 ) ) ;
#1861 = CARTESIAN_POINT ( 'NONE',  ( 15.32812500061451644, 4.541064518000418104, 2.621784821874999949 ) ) ;
#1862 = CARTESIAN_POINT ( 'NONE',  ( 25.87500000122903288, 2.886751345948129099, -4.999999999999998224 ) ) ;
#1863 =( BOUNDED_CURVE ( )  B_SPLINE_CURVE ( 2, ( #55253, #66705, #16078, #38627, #33075, #27911, #61151, #10546, #65962 ),
 .UNSPECIFIED., .F., .F. ) 
 B_SPLINE_CURVE_WITH_KNOTS ( ( 3, 2, 2, 2, 3 ),
 ( 0.1847826086956521896, 0.1884057971014492794, 0.1956521739130434867, 0.2028985507246376940, 0.2065217391304347838 ),
 .UNSPECIFIED. ) 
 CURVE ( )  GEOMETRIC_REPRESENTATION_ITEM ( )  RATIONAL_B_SPLINE_CURVE ( ( 0.9330127018922194093, 0.9330127018922196314, 1.000000000000000000, 0.8660254037844387076, 1.000000000000000000, 0.8660254037844387076, 1.000000000000000000, 0.9330127018922194093, 0.9330127018922194093 ) ) 
 REPRESENTATION_ITEM ( '' )  );
#1864 = CARTESIAN_POINT ( 'NONE',  ( 25.97812500061451502, 6.421520780324663323E-16, -5.243569643749999010 ) ) ;
#1865 = CARTESIAN_POINT ( 'NONE',  ( 20.89687500061452141, -3.027376345333614438, 5.243569643749998122 ) ) ;
#1866 = CARTESIAN_POINT ( 'NONE',  ( 15.32812500061451644, 4.541064518000418104, 2.621784821874999949 ) ) ;
#1867 = CARTESIAN_POINT ( 'NONE',  ( 9.001249775931846008E-16, 18.17187500061451999, 34.90005215228797653 ) ) ;
#1868 = CARTESIAN_POINT ( 'NONE',  ( 21.59062500061451928, 6.054752690667223547, 3.707466751127219781E-16 ) ) ;
#1869 = DIRECTION ( 'NONE',  ( -0.000000000000000000, -1.000000000000000000, -0.000000000000000000 ) ) ;
#1870 = VERTEX_POINT ( 'NONE', #51407 ) ;
#1871 = CARTESIAN_POINT ( 'NONE',  ( 25.72499999999999787, 6.123233995736764310E-16, -4.999999999999998224 ) ) ;
#1872 = CARTESIAN_POINT ( 'NONE',  ( 8.484601909799253346E-16, 12.46250000000000213, -25.38119784648299770 ) ) ;
#1873 = CARTESIAN_POINT ( 'NONE',  ( -3.756430356250001434, 19.76562499938548356, 32.16877607737301048 ) ) ;
#1874 = CARTESIAN_POINT ( 'NONE',  ( 28.75312500061451715, 4.541064518000418104, -2.621784821874998173 ) ) ;
#1875 = CARTESIAN_POINT ( 'NONE',  ( 8.240625000614516082, -3.027376345333614438, 5.243569643749998122 ) ) ;
#1876 = CARTESIAN_POINT ( 'NONE',  ( 21.03750000122903074, 4.330127018922191873, 2.499999999999999556 ) ) ;
#1877 = VECTOR ( 'NONE', #39271, 1000.000000000000000 ) ;
#1878 = CARTESIAN_POINT ( 'NONE',  ( 27.29062500061451502, -3.027376345333610441, -5.243569643749999898 ) ) ;
#1879 = CARTESIAN_POINT ( 'NONE',  ( 25.53750000000000142, -2.886751345948129988, 4.999999999999997335 ) ) ;
#1880 = CARTESIAN_POINT ( 'NONE',  ( 1.999999999999998668, 16.36250000122903359, -33.46410161513775705 ) ) ;
#1881 = CARTESIAN_POINT ( 'NONE',  ( 11.27812500061451573, 4.541064518000418104, 2.621784821874999949 ) ) ;
#1882 = ORIENTED_EDGE ( 'NONE', *, *, #22378, .F. ) ;
#1883 = AXIS2_PLACEMENT_3D ( 'NONE', #31887, #72139, #43707 ) ;
#1884 = CARTESIAN_POINT ( 'NONE',  ( 25.60312500061451502, 4.541064518000418104, -2.621784821874998173 ) ) ;
#1885 = CARTESIAN_POINT ( 'NONE',  ( 7.340625000614518392, -3.027376345333614438, 5.243569643749998122 ) ) ;
#1886 = UNCERTAINTY_MEASURE_WITH_UNIT (LENGTH_MEASURE( 1.000000000000000082E-05 ), #37411, 'distance_accuracy_value', 'NONE');
#1887 = VECTOR ( 'NONE', #21892, 1000.000000000000000 ) ;
#1888 = CARTESIAN_POINT ( 'NONE',  ( 3.290625000614516793, -3.027376345333614438, 5.243569643749998122 ) ) ;
#1889 = CARTESIAN_POINT ( 'NONE',  ( 17.55937500061451573, 4.119189519843966529, -2.378215178124998275 ) ) ;
#1890 = CARTESIAN_POINT ( 'NONE',  ( 17.85000000122903430, 5.773502691896255534, 3.535250795749688401E-16 ) ) ;
#1891 = CARTESIAN_POINT ( 'NONE',  ( 13.01249999999999929, -5.773502691896255534, -1.060575238724906372E-15 ) ) ;
#1892 = EDGE_CURVE ( 'NONE', #44258, #8626, #72202, .T. ) ;
#1893 = CARTESIAN_POINT ( 'NONE',  ( 14.37187500061451928, 3.027376345333613106, -5.243569643749998122 ) ) ;
#1894 = CARTESIAN_POINT ( 'NONE',  ( 8.962500001229033231, 0.000000000000000000, 4.999999999999998224 ) ) ;
#1895 = CARTESIAN_POINT ( 'NONE',  ( 15.98437500061451821, -4.541064518000419881, 2.621784821874995952 ) ) ;
#1896 = CARTESIAN_POINT ( 'NONE',  ( 16.42500000000000071, 4.330127018922191873, 2.499999999999999556 ) ) ;
#1897 = CARTESIAN_POINT ( 'NONE',  ( 9.421875000614519990, 3.027376345333613106, -5.243569643749998122 ) ) ;
#1898 = CARTESIAN_POINT ( 'NONE',  ( -4.243569643749997233, 12.19062500061451715, -27.54997392385601174 ) ) ;
#1899 = CARTESIAN_POINT ( 'NONE',  ( 1.071796769724491893, 16.53259618943233278, 33.99999999999999289 ) ) ;
#1900 = CARTESIAN_POINT ( 'NONE',  ( 22.80937500061451573, 2.746126346562645981, -4.756430356249997438 ) ) ;
#1901 = CARTESIAN_POINT ( 'NONE',  ( 30.00000000000000000, 0.000000000000000000, 0.000000000000000000 ) ) ;
#1902 = CARTESIAN_POINT ( 'NONE',  ( 24.36562500061451786, 3.027376345333611329, 5.243569643749999010 ) ) ;
#1903 = CARTESIAN_POINT ( 'NONE',  ( -1.999999999999997113, 17.48750000122903359, 33.46410161513775705 ) ) ;
#1904 = CARTESIAN_POINT ( 'NONE',  ( 29.44687500061451857, -3.027376345333614438, 5.243569643749998122 ) ) ;
#1905 = CARTESIAN_POINT ( 'NONE',  ( 22.05000000000000071, -4.330127018922190985, -2.500000000000001332 ) ) ;
#1906 = CARTESIAN_POINT ( 'NONE',  ( 6.440625000614517148, -3.027376345333614438, 5.243569643749998122 ) ) ;
#1907 = CARTESIAN_POINT ( 'NONE',  ( 24.34687500061451715, 0.000000000000000000, 4.756430356249998326 ) ) ;
#1908 = CARTESIAN_POINT ( 'NONE',  ( 16.35937500061451644, 0.000000000000000000, 5.243569643749999010 ) ) ;
#1909 = CARTESIAN_POINT ( 'NONE',  ( 8.521875000614517859, 4.119189519843966529, 2.378215178124999607 ) ) ;
#1910 = AXIS2_PLACEMENT_3D ( 'NONE', #26304, #64724, #37013 ) ;
#1911 = CARTESIAN_POINT ( 'NONE',  ( 3.253125000614518036, 0.000000000000000000, 5.243569643749999010 ) ) ;
#1912 = CARTESIAN_POINT ( 'NONE',  ( 7.921875000614517326, -6.054752690667223547, -1.112240025338166033E-15 ) ) ;
#1913 = ORIENTED_EDGE ( 'NONE', *, *, #7167, .T. ) ;
#1914 = CARTESIAN_POINT ( 'NONE',  ( 18.23437500061451999, -4.541064518000419881, 2.621784821874995952 ) ) ;
#1915 = CARTESIAN_POINT ( 'NONE',  ( -0.2617081364693537582, 25.54316770519903557, 33.99999999999999289 ) ) ;
#1916 = CARTESIAN_POINT ( 'NONE',  ( 26.39999999999999858, 0.000000000000000000, 4.999999999999998224 ) ) ;
#1917 = CARTESIAN_POINT ( 'NONE',  ( 28.43437500061451573, 4.541064518000418104, 2.621784821874999949 ) ) ;
#1918 = CARTESIAN_POINT ( 'NONE',  ( 0.000000000000000000, 27.50000000000000000, 26.00000000000000000 ) ) ;
#1919 = ORIENTED_EDGE ( 'NONE', *, *, #12871, .T. ) ;
#1920 = CARTESIAN_POINT ( 'NONE',  ( 10.01250000000000107, 2.886751345948129099, -4.999999999999998224 ) ) ;
#1921 = CARTESIAN_POINT ( 'NONE',  ( 12.94687500061451502, 4.119189519843966529, -2.378215178124998275 ) ) ;
#1922 = CARTESIAN_POINT ( 'NONE',  ( 23.42812500061451786, 4.541064518000418104, 2.621784821874999949 ) ) ;
#1923 = CARTESIAN_POINT ( 'NONE',  ( 14.66249999999999964, 2.886751345948126879, 4.999999999999999112 ) ) ;
#1924 = CARTESIAN_POINT ( 'NONE',  ( 8.512500001229033941, 0.000000000000000000, 4.999999999999998224 ) ) ;
#1925 = CARTESIAN_POINT ( 'NONE',  ( 6.253125000614517148, 4.541064518000418104, -2.621784821874998173 ) ) ;
#1926 = CARTESIAN_POINT ( 'NONE',  ( 20.88749999999999929, 5.773502691896255534, 3.535250795749688894E-16 ) ) ;
#1927 = CARTESIAN_POINT ( 'NONE',  ( 19.82812500061451644, 4.541064518000418104, 2.621784821874999949 ) ) ;
#1928 = CARTESIAN_POINT ( 'NONE',  ( 4.866723945449144217, 3.205296881438017387, 4.448262948007274176 ) ) ;
#1929 = CARTESIAN_POINT ( 'NONE',  ( 24.67500000122903359, 2.886751345948126879, 4.999999999999999112 ) ) ;
#1930 = CARTESIAN_POINT ( 'NONE',  ( -3.756430356250000990, 18.30312499938548143, 32.16877607737301048 ) ) ;
#1931 = CARTESIAN_POINT ( 'NONE',  ( 5.737499999999998934, -2.886751345948129988, 4.999999999999997335 ) ) ;
#1932 = ORIENTED_EDGE ( 'NONE', *, *, #20120, .T. ) ;
#1933 = CARTESIAN_POINT ( 'NONE',  ( 22.15312500061451573, 0.000000000000000000, 5.243569643749999010 ) ) ;
#1934 = CARTESIAN_POINT ( 'NONE',  ( 26.87812500061451360, 6.421520780324663323E-16, -5.243569643749999010 ) ) ;
#1935 = CARTESIAN_POINT ( 'NONE',  ( 27.64687500061452141, -3.027376345333614438, 5.243569643749998122 ) ) ;
#1936 = CARTESIAN_POINT ( 'NONE',  ( 15.47812500061451679, -4.541064518000419881, 2.621784821874995952 ) ) ;
#1937 = CARTESIAN_POINT ( 'NONE',  ( 4.804181228667060211, 1.395135997737601663, -4.980880193036001380 ) ) ;
#1938 = CARTESIAN_POINT ( 'NONE',  ( 25.53750000122903074, 4.330127018922191873, 2.499999999999999556 ) ) ;
#1939 = CARTESIAN_POINT ( 'NONE',  ( 19.77187500061451786, 2.746126346562645981, -4.756430356249997438 ) ) ;
#1940 = CARTESIAN_POINT ( 'NONE',  ( 16.37812500061451715, -4.541064518000419881, 2.621784821874995952 ) ) ;
#1941 = CARTESIAN_POINT ( 'NONE',  ( 3.999999999999998668, 14.52500000122903323, -32.30940107675850470 ) ) ;
#1942 = CARTESIAN_POINT ( 'NONE',  ( 5.925000001229033586, -5.773502691896255534, -1.060575238724906372E-15 ) ) ;
#1943 = CARTESIAN_POINT ( 'NONE',  ( 10.43437500061451750, 4.541064518000418104, 2.621784821874999949 ) ) ;
#1944 = CARTESIAN_POINT ( 'NONE',  ( 9.609375000614518214, 0.000000000000000000, 5.243569643749999010 ) ) ;
#1945 = CARTESIAN_POINT ( 'NONE',  ( 19.73437500061451644, 6.421520780324663323E-16, -5.243569643749999010 ) ) ;
#1946 = EDGE_LOOP ( 'NONE', ( #50933, #40270, #7996, #53284, #61619, #7313, #13137, #57510 ) ) ;
#1947 = CARTESIAN_POINT ( 'NONE',  ( -3.980704297455874840, 9.178376072143944242, 25.49448230662654780 ) ) ;
#1948 = CARTESIAN_POINT ( 'NONE',  ( 25.30312500061451431, 0.000000000000000000, 5.243569643749999010 ) ) ;
#1949 = CARTESIAN_POINT ( 'NONE',  ( 18.75937500061451857, -4.541064518000417216, -2.621784821875001281 ) ) ;
#1950 = CARTESIAN_POINT ( 'NONE',  ( 20.99062500061451431, -3.027376345333610441, -5.243569643749999898 ) ) ;
#1951 = CARTESIAN_POINT ( 'NONE',  ( -2.556497649636125342E-15, 18.87500000122903288, -26.00000000000000000 ) ) ;
#1952 = CARTESIAN_POINT ( 'NONE',  ( -2.000000000000000000, 14.52500000000000036, 26.53589838486224650 ) ) ;
#1953 = CARTESIAN_POINT ( 'NONE',  ( 3.121875000614518836, 3.027376345333613106, -5.243569643749998122 ) ) ;
#1954 = CARTESIAN_POINT ( 'NONE',  ( 8.625000001229034652, -5.773502691896255534, -1.060575238724906372E-15 ) ) ;
#1955 = ORIENTED_EDGE ( 'NONE', *, *, #51760, .T. ) ;
#1956 = CARTESIAN_POINT ( 'NONE',  ( 3.562500001229033764, 0.000000000000000000, 4.999999999999998224 ) ) ;
#1957 = CARTESIAN_POINT ( 'NONE',  ( -2.000000000000000000, 19.47499999999999787, -33.46410161513775705 ) ) ;
#1958 = CARTESIAN_POINT ( 'NONE',  ( 28.35000000122903430, -2.886751345948129988, 4.999999999999997335 ) ) ;
#1959 = CARTESIAN_POINT ( 'NONE',  ( -4.000000000000000888, 19.90624999877096357, 32.30940107675850470 ) ) ;
#1960 = CARTESIAN_POINT ( 'NONE',  ( 10.65937500061451715, -4.541064518000417216, -2.621784821875001281 ) ) ;
#1961 = CARTESIAN_POINT ( 'NONE',  ( 3.999999999999999112, 9.987500001229033586, 30.00000000000000000 ) ) ;
#1962 = CARTESIAN_POINT ( 'NONE',  ( 17.95312500061451644, 4.541064518000418104, -2.621784821874998173 ) ) ;
#1963 = CARTESIAN_POINT ( 'NONE',  ( 11.22187500061451892, 3.027376345333613106, -5.243569643749998122 ) ) ;
#1964 = CARTESIAN_POINT ( 'NONE',  ( 28.80000000122903003, -2.886751345948129988, 4.999999999999997335 ) ) ;
#1965 = CARTESIAN_POINT ( 'NONE',  ( 20.63437500061451857, 6.421520780324663323E-16, -5.243569643749999010 ) ) ;
#1966 = CARTESIAN_POINT ( 'NONE',  ( 7.134375000614516793, 6.421520780324663323E-16, -5.243569643749999010 ) ) ;
#1967 = CARTESIAN_POINT ( 'NONE',  ( 3.999999999999998668, 16.32500000122903216, 27.69059892324149530 ) ) ;
#1968 = CARTESIAN_POINT ( 'NONE',  ( 7.640625000614517326, 6.054752690667223547, 3.707466751127219781E-16 ) ) ;
#1969 = CARTESIAN_POINT ( 'NONE',  ( 18.81562500061452070, 3.027376345333613106, -5.243569643749998122 ) ) ;
#1970 = VERTEX_POINT ( 'NONE', #68042 ) ;
#1971 = EDGE_CURVE ( 'NONE', #40431, #36300, #21687, .T. ) ;
#1972 = CARTESIAN_POINT ( 'NONE',  ( 5.550000001229032698, -2.886751345948125991, -5.000000000000000000 ) ) ;
#1973 = CARTESIAN_POINT ( 'NONE',  ( 14.80312500061451608, 4.541064518000418104, -2.621784821874998173 ) ) ;
#1974 = CARTESIAN_POINT ( 'NONE',  ( 11.12812500061451715, 6.421520780324663323E-16, -5.243569643749999010 ) ) ;
#1975 = CARTESIAN_POINT ( 'NONE',  ( 23.14687500061451786, -2.746126346562646425, 4.756430356249996549 ) ) ;
#1976 = CARTESIAN_POINT ( 'NONE',  ( 11.36250000000000071, 2.886751345948129099, -4.999999999999998224 ) ) ;
#1977 = CARTESIAN_POINT ( 'NONE',  ( 5.400000001229032343, -2.886751345948129988, 4.999999999999997335 ) ) ;
#1978 = EDGE_CURVE ( 'NONE', #11117, #72537, #991, .T. ) ;
#1979 = CARTESIAN_POINT ( 'NONE',  ( 14.59687500061452070, -3.027376345333614438, 5.243569643749998122 ) ) ;
#1980 = CARTESIAN_POINT ( 'NONE',  ( 18.48750000122903359, -4.330127018922194537, 2.499999999999995559 ) ) ;
#1981 = CARTESIAN_POINT ( 'NONE',  ( 25.83749999999999858, 5.773502691896255534, 3.535250795749688894E-16 ) ) ;
#1982 = CARTESIAN_POINT ( 'NONE',  ( -4.243569643749997233, 18.94062500061451715, -27.54997392385601174 ) ) ;
#1983 = DIRECTION ( 'NONE',  ( 0.000000000000000000, 0.000000000000000000, -1.000000000000000000 ) ) ;
#1984 = CARTESIAN_POINT ( 'NONE',  ( 2.000000000000001332, 10.81250000122903465, -26.53589838486224650 ) ) ;
#1985 = CARTESIAN_POINT ( 'NONE',  ( 4.546875000614517326, 6.054752690667223547, 3.707466751127219781E-16 ) ) ;
#1986 = CARTESIAN_POINT ( 'NONE',  ( 18.94687500061451502, 6.054752690667223547, 3.707466751127219781E-16 ) ) ;
#1987 = FACE_OUTER_BOUND ( 'NONE', #53907, .T. ) ;
#1988 = CARTESIAN_POINT ( 'NONE',  ( 13.64062500061451644, -3.027376345333614438, 5.243569643749998122 ) ) ;
#1989 = CARTESIAN_POINT ( 'NONE',  ( 9.206250001229033586, 4.330127018922192761, -2.499999999999997780 ) ) ;
#1990 = CARTESIAN_POINT ( 'NONE',  ( 1.626862140677534273E-15, 17.52500000122903145, 34.00000000000000000 ) ) ;
#1991 = CARTESIAN_POINT ( 'NONE',  ( 23.82187500061451502, 3.027376345333613106, -5.243569643749998122 ) ) ;
#1992 = CARTESIAN_POINT ( 'NONE',  ( 17.97187500061451360, 4.119189519843966529, 2.378215178124999607 ) ) ;
#1993 = CARTESIAN_POINT ( 'NONE',  ( 11.09062500061451573, -3.027376345333610441, -5.243569643749999898 ) ) ;
#1994 = CARTESIAN_POINT ( 'NONE',  ( 15.57187500061451679, -6.054752690667223547, -1.112240025338166033E-15 ) ) ;
#1995 = ORIENTED_EDGE ( 'NONE', *, *, #58401, .T. ) ;
#1996 = CARTESIAN_POINT ( 'NONE',  ( 26.33437500061451431, -4.541064518000419881, 2.621784821874995952 ) ) ;
#1997 = VECTOR ( 'NONE', #2916, 1000.000000000000000 ) ;
#1998 = CARTESIAN_POINT ( 'NONE',  ( 26.46562500061451573, 3.027376345333613106, -5.243569643749998122 ) ) ;
#1999 = CARTESIAN_POINT ( 'NONE',  ( 19.67812500061451786, 6.421520780324663323E-16, -5.243569643749999010 ) ) ;
#2000 = CARTESIAN_POINT ( 'NONE',  ( 28.94062500061452070, -3.027376345333614438, 5.243569643749998122 ) ) ;
#2001 = FACE_OUTER_BOUND ( 'NONE', #10841, .T. ) ;
#2002 = CARTESIAN_POINT ( 'NONE',  ( 8.849999999999999645, 0.000000000000000000, 4.999999999999998224 ) ) ;
#2003 = CARTESIAN_POINT ( 'NONE',  ( 19.87500000122903288, -5.773502691896255534, -1.060575238724906372E-15 ) ) ;
#2004 = CARTESIAN_POINT ( 'NONE',  ( 9.909375000614517148, 2.746126346562643317, 4.756430356249998326 ) ) ;
#2005 = ORIENTED_EDGE ( 'NONE', *, *, #60921, .F. ) ;
#2006 = CARTESIAN_POINT ( 'NONE',  ( 17.21249999999999858, 2.886751345948129099, -4.999999999999998224 ) ) ;
#2007 = CARTESIAN_POINT ( 'NONE',  ( 20.28750000000000142, -2.886751345948125991, -5.000000000000000000 ) ) ;
#2008 = CARTESIAN_POINT ( 'NONE',  ( 18.87187500061451573, 3.027376345333613106, -5.243569643749998122 ) ) ;
#2009 = CARTESIAN_POINT ( 'NONE',  ( 12.85312500061451502, -4.541064518000417216, -2.621784821875001281 ) ) ;
#2010 = ORIENTED_EDGE ( 'NONE', *, *, #40326, .T. ) ;
#2011 = DIRECTION ( 'NONE',  ( 0.000000000000000000, 0.000000000000000000, 1.000000000000000000 ) ) ;
#2012 = CARTESIAN_POINT ( 'NONE',  ( 4.828125000614518214, 6.421520780324663323E-16, -5.243569643749999010 ) ) ;
#2013 = CARTESIAN_POINT ( 'NONE',  ( 3.144856541311010556, 3.887142566792906706, -3.519253510942787599 ) ) ;
#2014 = CARTESIAN_POINT ( 'NONE',  ( 11.40000000000000036, 4.330127018922192761, -2.499999999999997780 ) ) ;
#2015 = CARTESIAN_POINT ( 'NONE',  ( 27.49687500061451573, 0.000000000000000000, 4.756430356249998326 ) ) ;
#2016 = CARTESIAN_POINT ( 'NONE',  ( -4.243569643749997233, 15.34062500061451750, 32.45002607614398471 ) ) ;
#2017 = CARTESIAN_POINT ( 'NONE',  ( 28.56562500061451715, -6.054752690667223547, -1.112240025338166033E-15 ) ) ;
#2018 = CARTESIAN_POINT ( 'NONE',  ( 8.437500000000000000, -2.886751345948129988, 4.999999999999997335 ) ) ;
#2019 = CARTESIAN_POINT ( 'NONE',  ( 3.756430356250000102, 17.14062499938548356, 30.00000000000000000 ) ) ;
#2020 = CARTESIAN_POINT ( 'NONE',  ( 24.19687500061451857, -3.027376345333610441, -5.243569643749999898 ) ) ;
#2021 = ORIENTED_EDGE ( 'NONE', *, *, #59244, .T. ) ;
#2022 = CARTESIAN_POINT ( 'NONE',  ( 22.22812500061451502, -4.541064518000419881, 2.621784821874995952 ) ) ;
#2023 = CARTESIAN_POINT ( 'NONE',  ( 23.59687500061451715, -3.027376345333614438, 5.243569643749998122 ) ) ;
#2024 = CARTESIAN_POINT ( 'NONE',  ( -3.000416591977282496E-16, 16.09062500061459744, -34.90005215228797653 ) ) ;
#2025 = CARTESIAN_POINT ( 'NONE',  ( 6.890625000614516438, -3.027376345333614438, 5.243569643749998122 ) ) ;
#2026 = CARTESIAN_POINT ( 'NONE',  ( 28.80937500061451573, 4.119189519843966529, -2.378215178124998275 ) ) ;
#2027 = CARTESIAN_POINT ( 'NONE',  ( 24.96562500061451217, -6.054752690667223547, -1.112240025338166033E-15 ) ) ;
#2028 = CARTESIAN_POINT ( 'NONE',  ( 28.73437500061451644, 5.492252693125287522, 3.363034840372157021E-16 ) ) ;
#2029 = CARTESIAN_POINT ( 'NONE',  ( 9.571875000614518569, 2.746126346562643317, 4.756430356249998326 ) ) ;
#2030 = CARTESIAN_POINT ( 'NONE',  ( 18.00937500061451502, 4.541064518000418104, -2.621784821874998173 ) ) ;
#2031 = CARTESIAN_POINT ( 'NONE',  ( 27.79687500061451999, -3.027376345333610441, -5.243569643749999898 ) ) ;
#2032 = CARTESIAN_POINT ( 'NONE',  ( -4.243569643749999898, 17.12187500061451573, 27.54997392385601529 ) ) ;
#2033 = CARTESIAN_POINT ( 'NONE',  ( 7.940625000614518036, -3.027376345333610441, -5.243569643749999898 ) ) ;
#2034 = CARTESIAN_POINT ( 'NONE',  ( 1.999999999999998668, 16.25000000000000000, 26.53589838486224650 ) ) ;
#2035 = CARTESIAN_POINT ( 'NONE',  ( 4.359375000614517326, -4.541064518000417216, -2.621784821875001281 ) ) ;
#2036 = CARTESIAN_POINT ( 'NONE',  ( 4.311958327294343363, 2.531208285321026263, 4.311958327294242999 ) ) ;
#2037 = CARTESIAN_POINT ( 'NONE',  ( 4.003125000614518925, 4.541064518000418104, -2.621784821874998173 ) ) ;
#2038 = CARTESIAN_POINT ( 'NONE',  ( 10.54687500061451644, -3.027376345333614438, 5.243569643749998122 ) ) ;
#2039 = CARTESIAN_POINT ( 'NONE',  ( 17.13750000122903216, -4.330127018922194537, 2.499999999999995559 ) ) ;
#2040 = CARTESIAN_POINT ( 'NONE',  ( 6.459375000614518747, 0.000000000000000000, 5.243569643749999010 ) ) ;
#2041 = CARTESIAN_POINT ( 'NONE',  ( 7.453125000614516438, -4.541064518000417216, -2.621784821875001281 ) ) ;
#2042 = CARTESIAN_POINT ( 'NONE',  ( -4.000000000000000000, 14.46874999877096712, 30.00000000000000000 ) ) ;
#2043 = CARTESIAN_POINT ( 'NONE',  ( 22.06875000122903074, -5.773502691896255534, -1.060575238724906372E-15 ) ) ;
#2044 = CARTESIAN_POINT ( 'NONE',  ( 15.72187500061451892, 3.027376345333613106, -5.243569643749998122 ) ) ;
#2045 = CYLINDRICAL_SURFACE ( 'NONE', #63174, 4.000000000000000000 ) ;
#2046 = ORIENTED_EDGE ( 'NONE', *, *, #3025, .F. ) ;
#2047 = CARTESIAN_POINT ( 'NONE',  ( 23.72812500061451502, 6.421520780324663323E-16, -5.243569643749999010 ) ) ;
#2048 = CARTESIAN_POINT ( 'NONE',  ( 10.26562500061451644, 3.027376345333613106, -5.243569643749998122 ) ) ;
#2049 = CARTESIAN_POINT ( 'NONE',  ( 27.12187500061451573, 3.027376345333611329, 5.243569643749999010 ) ) ;
#2050 = CARTESIAN_POINT ( 'NONE',  ( 8.803125000614517859, -4.541064518000417216, -2.621784821875001281 ) ) ;
#2051 = DIRECTION ( 'NONE',  ( -1.000000000000000000, -0.000000000000000000, -0.000000000000000000 ) ) ;
#2052 = CARTESIAN_POINT ( 'NONE',  ( 9.975000001229034297, -5.773502691896255534, -1.060575238724906372E-15 ) ) ;
#2053 = CARTESIAN_POINT ( 'NONE',  ( 24.06562500061451715, -6.054752690667223547, -1.112240025338166033E-15 ) ) ;
#2054 = CARTESIAN_POINT ( 'NONE',  ( -4.243569643749999898, 13.05312500061451786, -30.00000000000000000 ) ) ;
#2055 = CARTESIAN_POINT ( 'NONE',  ( 13.16250000122903430, -4.330127018922190985, -2.500000000000001332 ) ) ;
#2056 = CARTESIAN_POINT ( 'NONE',  ( 20.95312500061451999, -4.541064518000417216, -2.621784821875001281 ) ) ;
#2057 = CARTESIAN_POINT ( 'NONE',  ( 21.40312500061451573, -4.541064518000417216, -2.621784821875001281 ) ) ;
#2058 = CARTESIAN_POINT ( 'NONE',  ( 29.74687500061451217, 5.492252693125287522, 3.363034840372157021E-16 ) ) ;
#2059 = ADVANCED_FACE ( 'NONE', ( #61757 ), #11160, .F. ) ;
#2060 = CARTESIAN_POINT ( 'NONE',  ( 21.41250000000000497, 2.886751345948126879, 4.999999999999999112 ) ) ;
#2061 = CARTESIAN_POINT ( 'NONE',  ( 14.70000000122903394, 5.773502691896255534, 3.535250795749688894E-16 ) ) ;
#2062 = AXIS2_PLACEMENT_3D ( 'NONE', #23719, #34449, #45557 ) ;
#2063 = CARTESIAN_POINT ( 'NONE',  ( 10.34062500061451750, 6.054752690667223547, 3.707466751127219781E-16 ) ) ;
#2064 = CARTESIAN_POINT ( 'NONE',  ( 14.50312500061451537, 0.000000000000000000, 5.243569643749999010 ) ) ;
#2065 =( BOUNDED_CURVE ( )  B_SPLINE_CURVE ( 2, ( #13330, #17779, #35512, #51426, #57318, #7441, #24423 ),
 .UNSPECIFIED., .F., .F. ) 
 B_SPLINE_CURVE_WITH_KNOTS ( ( 3, 2, 2, 3 ),
 ( 0.07499999999999996947, 0.07777777777777775126, 0.08055555555555551916, 0.08333333333333328707 ),
 .UNSPECIFIED. ) 
 CURVE ( )  GEOMETRIC_REPRESENTATION_ITEM ( )  RATIONAL_B_SPLINE_CURVE ( ( 1.000000000000001332, 0.8660254037844373753, 1.000000000000000000, 0.8660254037844387076, 1.000000000000000000, 0.8660254037844407060, 0.9999999999999980016 ) ) 
 REPRESENTATION_ITEM ( '' )  );
#2066 = CARTESIAN_POINT ( 'NONE',  ( 24.86250000122903359, -4.330127018922190985, -2.500000000000001332 ) ) ;
#2067 = CARTESIAN_POINT ( 'NONE',  ( 20.74687500061451573, 6.054752690667223547, 3.707466751127219781E-16 ) ) ;
#2068 = FACE_OUTER_BOUND ( 'NONE', #6092, .T. ) ;
#2069 = CARTESIAN_POINT ( 'NONE',  ( 8.137500001229033941, -4.330127018922194537, 2.499999999999995559 ) ) ;
#2070 = CARTESIAN_POINT ( 'NONE',  ( 5.634375000614519458, -4.541064518000419881, 2.621784821874995952 ) ) ;
#2071 = CARTESIAN_POINT ( 'NONE',  ( 26.40937500061451715, -4.541064518000417216, -2.621784821875001281 ) ) ;
#2072 = CARTESIAN_POINT ( 'NONE',  ( 2.934375000614518392, -4.541064518000419881, 2.621784821874995952 ) ) ;
#2073 = CARTESIAN_POINT ( 'NONE',  ( 21.44062500061452070, -3.027376345333610441, -5.243569643749999898 ) ) ;
#2074 = CARTESIAN_POINT ( 'NONE',  ( 26.82187500061451857, -6.054752690667223547, -1.112240025338166033E-15 ) ) ;
#2075 = CARTESIAN_POINT ( 'NONE',  ( -1.878215178125001827, 17.55312499938548498, 33.25316411605952283 ) ) ;
#2076 = DIRECTION ( 'NONE',  ( 0.000000000000000000, 0.000000000000000000, 1.000000000000000000 ) ) ;
#2077 = CARTESIAN_POINT ( 'NONE',  ( 28.25625000122903074, 0.000000000000000000, 4.999999999999998224 ) ) ;
#2078 = CARTESIAN_POINT ( 'NONE',  ( 7.359375000614516438, 0.000000000000000000, 5.243569643749999010 ) ) ;
#2079 = CARTESIAN_POINT ( 'NONE',  ( 17.84062500061451573, -3.027376345333610441, -5.243569643749999898 ) ) ;
#2080 = VERTEX_POINT ( 'NONE', #36056 ) ;
#2081 = CARTESIAN_POINT ( 'NONE',  ( -5.810221930991193690E-16, 12.68750000000000000, -34.00000000000000000 ) ) ;
#2082 = CARTESIAN_POINT ( 'NONE',  ( 26.69062500061451715, -3.027376345333614438, 5.243569643749998122 ) ) ;
#2083 = CARTESIAN_POINT ( 'NONE',  ( 4.434375000614519280, 6.421520780324663323E-16, -5.243569643749999010 ) ) ;
#2084 = LINE ( 'NONE', #13876, #33673 ) ;
#2085 = CARTESIAN_POINT ( 'NONE',  ( 4.093805572639152679, 3.908117946951304766, 3.718080441408566195 ) ) ;
#2086 = CARTESIAN_POINT ( 'NONE',  ( 17.96250000000000213, -5.773502691896255534, -1.060575238724906372E-15 ) ) ;
#2087 = CARTESIAN_POINT ( 'NONE',  ( 20.54062500061451502, -3.027376345333610441, -5.243569643749999898 ) ) ;
#2088 = ORIENTED_EDGE ( 'NONE', *, *, #50142, .T. ) ;
#2089 = CARTESIAN_POINT ( 'NONE',  ( 24.41250000000000142, 2.886751345948129099, -4.999999999999998224 ) ) ;
#2090 = CARTESIAN_POINT ( 'NONE',  ( 25.80937500061451928, 0.000000000000000000, 5.243569643749999010 ) ) ;
#2091 = VERTEX_POINT ( 'NONE', #26072 ) ;
#2092 = CARTESIAN_POINT ( 'NONE',  ( 13.30312500061451786, -4.541064518000417216, -2.621784821875001281 ) ) ;
#2093 = CARTESIAN_POINT ( 'NONE',  ( 4.865625000614517859, 3.027376345333613106, -5.243569643749998122 ) ) ;
#2094 = CARTESIAN_POINT ( 'NONE',  ( 15.42187500061451466, -4.119189519843968306, 2.378215178124996054 ) ) ;
#2095 = CARTESIAN_POINT ( 'NONE',  ( 3.084375000614519191, 6.421520780324663323E-16, -5.243569643749999010 ) ) ;
#2096 = CARTESIAN_POINT ( 'NONE',  ( 15.82500000122903216, -5.773502691896255534, -1.060575238724906372E-15 ) ) ;
#2097 = CARTESIAN_POINT ( 'NONE',  ( 20.32499999999999929, 6.123233995736764310E-16, -4.999999999999998224 ) ) ;
#2098 = CARTESIAN_POINT ( 'NONE',  ( 27.93750000000000000, -2.886751345948125991, -5.000000000000000000 ) ) ;
#2099 = CARTESIAN_POINT ( 'NONE',  ( 4.809375000614516615, -4.541064518000417216, -2.621784821875001281 ) ) ;
#2100 = CARTESIAN_POINT ( 'NONE',  ( 9.871875000614517504, 3.027376345333613106, -5.243569643749998122 ) ) ;
#2101 = CARTESIAN_POINT ( 'NONE',  ( 18.23437500061451999, -4.541064518000419881, 2.621784821874995952 ) ) ;
#2102 = CARTESIAN_POINT ( 'NONE',  ( 11.49375000122903145, 5.773502691896255534, 3.535250795749688401E-16 ) ) ;
#2103 = VERTEX_POINT ( 'NONE', #30875 ) ;
#2104 = CARTESIAN_POINT ( 'NONE',  ( 28.19062500061451715, -3.027376345333610441, -5.243569643749999898 ) ) ;
#2105 = CARTESIAN_POINT ( 'NONE',  ( 3.825000000000001954, 4.330127018922191873, 2.499999999999999556 ) ) ;
#2106 = CARTESIAN_POINT ( 'NONE',  ( 3.759375000614517681, 0.000000000000000000, 5.243569643749999010 ) ) ;
#2107 = CARTESIAN_POINT ( 'NONE',  ( 17.28750000000000142, 5.773502691896255534, 3.535250795749688894E-16 ) ) ;
#2108 = CARTESIAN_POINT ( 'NONE',  ( 14.61562500061451608, -6.054752690667223547, -1.112240025338166033E-15 ) ) ;
#2109 = CARTESIAN_POINT ( 'NONE',  ( 1.626862140677534273E-15, 13.92500000122903181, 34.00000000000000000 ) ) ;
#2110 = CARTESIAN_POINT ( 'NONE',  ( 26.84999999999999787, 0.000000000000000000, 4.999999999999998224 ) ) ;
#2111 = CARTESIAN_POINT ( 'NONE',  ( 18.97500000122903074, -5.773502691896255534, -1.060575238724906372E-15 ) ) ;
#2112 = CARTESIAN_POINT ( 'NONE',  ( 1.009598436472905814, 9.950840295117078682, 24.08220839835972527 ) ) ;
#2113 = CARTESIAN_POINT ( 'NONE',  ( 18.49687500061452283, 5.492252693125287522, 3.363034840372157021E-16 ) ) ;
#2114 = CARTESIAN_POINT ( 'NONE',  ( 7.303125000614516082, 0.000000000000000000, 5.243569643749999010 ) ) ;
#2115 = CARTESIAN_POINT ( 'NONE',  ( 23.85937500061451644, 4.541064518000418104, -2.621784821874998173 ) ) ;
#2116 = CARTESIAN_POINT ( 'NONE',  ( 27.18750000122903288, 6.123233995736764310E-16, -4.999999999999998224 ) ) ;
#2117 = CARTESIAN_POINT ( 'NONE',  ( 27.34687500061451360, -3.027376345333610441, -5.243569643749999898 ) ) ;
#2118 = CARTESIAN_POINT ( 'NONE',  ( 8.512499999999999289, -5.773502691896255534, -1.060575238724906372E-15 ) ) ;
#2119 = CARTESIAN_POINT ( 'NONE',  ( 8.484601909799253346E-16, 13.02500000122903501, 34.61880215351700230 ) ) ;
#2120 = CARTESIAN_POINT ( 'NONE',  ( 13.79062500061451502, -3.027376345333610441, -5.243569643749999898 ) ) ;
#2121 = CARTESIAN_POINT ( 'NONE',  ( 7.800000001229035362, -2.886751345948125991, -5.000000000000000000 ) ) ;
#2122 = EDGE_CURVE ( 'NONE', #31702, #69475, #39613, .T. ) ;
#2123 = CARTESIAN_POINT ( 'NONE',  ( 11.97187500061451892, -6.054752690667223547, -1.112240025338166033E-15 ) ) ;
#2124 = CARTESIAN_POINT ( 'NONE',  ( -2.674018119152294037, 4.230323444455001969, -27.01458192567231364 ) ) ;
#2125 = EDGE_LOOP ( 'NONE', ( #61952, #62682, #70320, #3688 ) ) ;
#2126 = CARTESIAN_POINT ( 'NONE',  ( 11.27812500061451573, 4.541064518000418104, 2.621784821874999949 ) ) ;
#2127 = CARTESIAN_POINT ( 'NONE',  ( 5.810221930991193690E-16, 13.96249999999999858, 26.00000000000000000 ) ) ;
#2128 = CARTESIAN_POINT ( 'NONE',  ( 24.60000000122903430, 5.773502691896255534, 3.535250795749688894E-16 ) ) ;
#2129 = CARTESIAN_POINT ( 'NONE',  ( 13.43437500061451750, 6.421520780324663323E-16, -5.243569643749999010 ) ) ;
#2130 = CARTESIAN_POINT ( 'NONE',  ( 14.87812500061451537, 4.541064518000418104, 2.621784821874999949 ) ) ;
#2131 = CARTESIAN_POINT ( 'NONE',  ( 1.626862140677534273E-15, 18.76250000000000284, -26.00000000000000355 ) ) ;
#2132 = CARTESIAN_POINT ( 'NONE',  ( 23.14687500061451786, -3.027376345333614438, 5.243569643749998122 ) ) ;
#2133 = DIRECTION ( 'NONE',  ( 0.000000000000000000, 0.000000000000000000, 1.000000000000000000 ) ) ;
#2134 = CARTESIAN_POINT ( 'NONE',  ( 1.626862140677534273E-15, 18.42500000122903359, -26.00000000000000355 ) ) ;
#2135 = CARTESIAN_POINT ( 'NONE',  ( -2.000000000000000000, 19.47499999999999787, 26.53589838486224650 ) ) ;
#2136 = CARTESIAN_POINT ( 'NONE',  ( -2.121784821874996840, 15.43437500061451928, -26.32496088578401583 ) ) ;
#2137 = CARTESIAN_POINT ( 'NONE',  ( 16.28437500061452070, 4.541064518000418104, 2.621784821874999949 ) ) ;
#2138 = CARTESIAN_POINT ( 'NONE',  ( 17.77500000122903145, 2.886751345948129099, -4.999999999999998224 ) ) ;
#2139 = CARTESIAN_POINT ( 'NONE',  ( 12.90937500061451537, -4.541064518000417216, -2.621784821875001281 ) ) ;
#2140 = CARTESIAN_POINT ( 'NONE',  ( 9.001249775931846008E-16, 10.52187500061451964, 34.90005215228797653 ) ) ;
#2141 = CARTESIAN_POINT ( 'NONE',  ( 19.38750000122903216, -4.330127018922194537, 2.499999999999995559 ) ) ;
#2142 = CARTESIAN_POINT ( 'NONE',  ( 11.69062500061451360, 6.054752690667223547, 3.707466751127219781E-16 ) ) ;
#2143 = EDGE_LOOP ( 'NONE', ( #13027, #58345, #56433, #44405 ) ) ;
#2144 = EDGE_LOOP ( 'NONE', ( #2437, #31615, #54378, #3537 ) ) ;
#2145 = CARTESIAN_POINT ( 'NONE',  ( 17.58749999999999858, -2.886751345948125991, -5.000000000000000000 ) ) ;
#2146 = CARTESIAN_POINT ( 'NONE',  ( 27.48749999999999716, -2.886751345948092684, -5.000000000000057732 ) ) ;
#2147 = CARTESIAN_POINT ( 'NONE',  ( 11.82187500061451857, 3.027376345333611329, 5.243569643749999010 ) ) ;
#2148 = CARTESIAN_POINT ( 'NONE',  ( 22.38750000000000284, -2.886751345948096681, 5.000000000000054179 ) ) ;
#2149 = CARTESIAN_POINT ( 'NONE',  ( 13.68750000122903288, 6.123233995736764310E-16, -4.999999999999998224 ) ) ;
#2150 = CARTESIAN_POINT ( 'NONE',  ( 21.71250000122903501, -4.330127018922190985, -2.500000000000001332 ) ) ;
#2151 = CARTESIAN_POINT ( 'NONE',  ( 18.55312500061451431, 0.000000000000000000, 5.243569643749999010 ) ) ;
#2152 = CARTESIAN_POINT ( 'NONE',  ( 20.27812500061451573, 4.541064518000418104, 2.621784821874999949 ) ) ;
#2153 = CARTESIAN_POINT ( 'NONE',  ( 29.06250000122903288, 4.330127018922192761, -2.499999999999997780 ) ) ;
#2154 = CARTESIAN_POINT ( 'NONE',  ( 27.44999999999999929, -4.330127018922190985, -2.500000000000001332 ) ) ;
#2155 = CARTESIAN_POINT ( 'NONE',  ( 27.07499999999999929, 6.123233995736764310E-16, -4.999999999999998224 ) ) ;
#2156 = CARTESIAN_POINT ( 'NONE',  ( 28.46249999999999858, 2.886751345948129099, -4.999999999999998224 ) ) ;
#2157 = CARTESIAN_POINT ( 'NONE',  ( 27.49687500061451217, 6.054752690667223547, 3.707466751127219781E-16 ) ) ;
#2158 = CARTESIAN_POINT ( 'NONE',  ( 4.243569643749999010, 16.07187500061451857, -32.45002607614398471 ) ) ;
#2159 = ADVANCED_FACE ( 'NONE', ( #64859 ), #37519, .F. ) ;
#2160 = CARTESIAN_POINT ( 'NONE',  ( 3.225000001229033408, -5.773502691896255534, -1.060575238724906372E-15 ) ) ;
#2161 = CARTESIAN_POINT ( 'NONE',  ( 6.225000000000001421, -4.330127018922194537, 2.499999999999995559 ) ) ;
#2162 = CARTESIAN_POINT ( 'NONE',  ( 3.598871848003822649, 4.117104574466481814, -3.356104984449806761 ) ) ;
#2163 = CARTESIAN_POINT ( 'NONE',  ( 10.58437500061451964, -4.541064518000419881, 2.621784821874995952 ) ) ;
#2164 = CARTESIAN_POINT ( 'NONE',  ( 29.35312500061451502, 0.000000000000000000, 5.243569643749999010 ) ) ;
#2165 = CYLINDRICAL_SURFACE ( 'NONE', #11436, 4.999999999999998224 ) ;
#2166 = CARTESIAN_POINT ( 'NONE',  ( -3.671862074746357063, 9.302863167343950579, -25.25083824868577764 ) ) ;
#2167 = CARTESIAN_POINT ( 'NONE',  ( -3.999999999999997335, 19.25000000122903288, 32.30940107675850470 ) ) ;
#2168 = CARTESIAN_POINT ( 'NONE',  ( 8.296875000614516438, -3.027376345333614438, 5.243569643749998122 ) ) ;
#2169 = CARTESIAN_POINT ( 'NONE',  ( 10.58437500061451964, -4.541064518000419881, 2.621784821874995952 ) ) ;
#2170 = CARTESIAN_POINT ( 'NONE',  ( 6.937499999999999112, 5.773502691896255534, 3.535250795749688894E-16 ) ) ;
#2171 = CARTESIAN_POINT ( 'NONE',  ( 4.243569643749999010, 14.66562500061459495, 27.54997392385601174 ) ) ;
#2172 = CARTESIAN_POINT ( 'NONE',  ( 3.197688915245457508, 25.19820453330248000, 32.45943478522090686 ) ) ;
#2173 = CARTESIAN_POINT ( 'NONE',  ( 6.075000000000000178, 4.330127018922191873, 2.499999999999999556 ) ) ;
#2174 = CARTESIAN_POINT ( 'NONE',  ( 16.47187500061451715, 5.824947211148865298E-16, -4.756430356249998326 ) ) ;
#2175 = CARTESIAN_POINT ( 'NONE',  ( 21.47812500061451502, 6.421520780324663323E-16, -5.243569643749999010 ) ) ;
#2176 = CARTESIAN_POINT ( 'NONE',  ( 12.40312500061451573, -4.541064518000417216, -2.621784821875001281 ) ) ;
#2177 = CARTESIAN_POINT ( 'NONE',  ( 23.48437500061451644, -2.746126346562646425, 4.756430356249996549 ) ) ;
#2178 = CARTESIAN_POINT ( 'NONE',  ( 9.834375000614517859, 6.421520780324663323E-16, -5.243569643749999010 ) ) ;
#2179 = CARTESIAN_POINT ( 'NONE',  ( 25.76249999999999929, 2.886751345948129099, -4.999999999999998224 ) ) ;
#2180 = CARTESIAN_POINT ( 'NONE',  ( 23.70000000122903216, 5.773502691896255534, 3.535250795749688894E-16 ) ) ;
#2181 = CARTESIAN_POINT ( 'NONE',  ( 1.626862140677534273E-15, 18.42500000122903359, -26.00000000000000355 ) ) ;
#2182 = CARTESIAN_POINT ( 'NONE',  ( 11.78437500061451892, 4.541064518000418104, 2.621784821874999949 ) ) ;
#2183 = CARTESIAN_POINT ( 'NONE',  ( 26.03437500061451715, 6.421520780324663323E-16, -5.243569643749999010 ) ) ;
#2184 = DIRECTION ( 'NONE',  ( -0.000000000000000000, -1.000000000000000000, -0.000000000000000000 ) ) ;
#2185 = CARTESIAN_POINT ( 'NONE',  ( 18.52499999999999858, 6.123233995736764310E-16, -4.999999999999998224 ) ) ;
#2186 = CARTESIAN_POINT ( 'NONE',  ( 19.80937500061451573, 4.541064518000418104, -2.621784821874998173 ) ) ;
#2187 = CARTESIAN_POINT ( 'NONE',  ( 11.29687500061451644, 6.054752690667223547, 3.707466751127219781E-16 ) ) ;
#2188 = CARTESIAN_POINT ( 'NONE',  ( 2.655984681222220721E-16, 17.36562499938548498, 25.66244784525396483 ) ) ;
#2189 = CARTESIAN_POINT ( 'NONE',  ( 22.42500000000000071, -4.330127018922194537, 2.499999999999995559 ) ) ;
#2190 = CARTESIAN_POINT ( 'NONE',  ( 2.000000000000000444, 12.57500000000000107, 26.53589838486224650 ) ) ;
#2191 = CARTESIAN_POINT ( 'NONE',  ( 4.243569643749999010, 12.92187500061451644, -32.45002607614398471 ) ) ;
#2192 = CARTESIAN_POINT ( 'NONE',  ( 27.27187500061451431, -5.492252693125287522, -1.008910452111647106E-15 ) ) ;
#2193 = CARTESIAN_POINT ( 'NONE',  ( 15.32812500061451644, 4.541064518000418104, 2.621784821874999949 ) ) ;
#2194 = CARTESIAN_POINT ( 'NONE',  ( 4.912499999999999645, -5.773502691896255534, -1.060575238724906372E-15 ) ) ;
#2195 = DIRECTION ( 'NONE',  ( -0.000000000000000000, -1.000000000000000000, -0.000000000000000000 ) ) ;
#2196 = CARTESIAN_POINT ( 'NONE',  ( 3.242103837493086330E-14, 13.13749999999999929, -34.00000000000000000 ) ) ;
#2197 = CARTESIAN_POINT ( 'NONE',  ( 14.84999999999999964, -4.330127018922190985, -2.500000000000001332 ) ) ;
#2198 = CARTESIAN_POINT ( 'NONE',  ( 2.121784821874999061, 11.55312500061451786, 26.32496088578401583 ) ) ;
#2199 = CARTESIAN_POINT ( 'NONE',  ( 13.38750000122903394, 4.330127018922191873, 2.499999999999999556 ) ) ;
#2200 = CARTESIAN_POINT ( 'NONE',  ( 25.43437500061451573, -4.541064518000419881, 2.621784821874995952 ) ) ;
#2201 = CARTESIAN_POINT ( 'NONE',  ( 4.027635003466097707, 2.962795348797195416, -4.326299380533228600 ) ) ;
#2202 = EDGE_LOOP ( 'NONE', ( #21465, #47503 ) ) ;
#2203 = CARTESIAN_POINT ( 'NONE',  ( 18.62812500061451715, -4.541064518000419881, 2.621784821874995952 ) ) ;
#2204 = CARTESIAN_POINT ( 'NONE',  ( 3.665625000614517681, 3.027376345333611329, 5.243569643749999010 ) ) ;
#2205 = CARTESIAN_POINT ( 'NONE',  ( 18.98437500061451644, 4.541064518000418104, 2.621784821874999949 ) ) ;
#2206 = CARTESIAN_POINT ( 'NONE',  ( 3.937500000000000444, -2.886751345948129988, 4.999999999999997335 ) ) ;
#2207 = CARTESIAN_POINT ( 'NONE',  ( 6.328125000614515550, 4.541064518000418104, 2.621784821874999949 ) ) ;
#2208 = CARTESIAN_POINT ( 'NONE',  ( 21.89062500061451289, -3.027376345333610441, -5.243569643749999898 ) ) ;
#2209 = CARTESIAN_POINT ( 'NONE',  ( -4.243569643749999898, 15.30312500061451608, 30.00000000000000000 ) ) ;
#2210 = CARTESIAN_POINT ( 'NONE',  ( 18.15000000122903501, -2.886751345948125991, -5.000000000000000000 ) ) ;
#2211 = CARTESIAN_POINT ( 'NONE',  ( 13.17187500061451821, 2.746126346562643317, 4.756430356249998326 ) ) ;
#2212 = CARTESIAN_POINT ( 'NONE',  ( 10.30312500061451431, 4.541064518000418104, -2.621784821874998173 ) ) ;
#2213 = CARTESIAN_POINT ( 'NONE',  ( 3.084375000614519191, 6.421520780324663323E-16, -5.243569643749999010 ) ) ;
#2214 = CARTESIAN_POINT ( 'NONE',  ( 3.496875000614518836, -3.027376345333610441, -5.243569643749999898 ) ) ;
#2215 =( BOUNDED_CURVE ( )  B_SPLINE_CURVE ( 2, ( #15681, #21961, #60746, #10157, #29678, #12683, #12320, #13040, #47036 ),
 .UNSPECIFIED., .F., .F. ) 
 B_SPLINE_CURVE_WITH_KNOTS ( ( 3, 2, 2, 2, 3 ),
 ( 0.1805555555555555525, 0.1851851851851851749, 0.1944444444444444475, 0.2037037037037036924, 0.2083333333333333426 ),
 .UNSPECIFIED. ) 
 CURVE ( )  GEOMETRIC_REPRESENTATION_ITEM ( )  RATIONAL_B_SPLINE_CURVE ( ( 0.9330127018922194093, 0.9330127018922194093, 1.000000000000000000, 0.8660254037844387076, 1.000000000000000000, 0.8660254037844387076, 1.000000000000000000, 0.9330127018922191873, 0.9330127018922194093 ) ) 
 REPRESENTATION_ITEM ( '' )  );
#2216 = ADVANCED_FACE ( 'NONE', ( #14247 ), #53785, .T. ) ;
#2217 = CARTESIAN_POINT ( 'NONE',  ( 23.14687500061451786, -3.027376345333614438, 5.243569643749998122 ) ) ;
#2218 = CARTESIAN_POINT ( 'NONE',  ( 13.37812500061451715, 6.421520780324663323E-16, -5.243569643749999010 ) ) ;
#2219 = CARTESIAN_POINT ( 'NONE',  ( 26.02500000122903145, 2.886751345948126879, 4.999999999999999112 ) ) ;
#2220 = CARTESIAN_POINT ( 'NONE',  ( 26.50312500061451360, 4.541064518000418104, -2.621784821874998173 ) ) ;
#2221 = CARTESIAN_POINT ( 'NONE',  ( 19.28437500061451360, 6.421520780324663323E-16, -5.243569643749999010 ) ) ;
#2222 = CARTESIAN_POINT ( 'NONE',  ( 14.20312500061451644, -4.541064518000417216, -2.621784821875001281 ) ) ;
#2223 = CARTESIAN_POINT ( 'NONE',  ( 2.121784821874999061, 16.55937500061451573, 26.32496088578401583 ) ) ;
#2224 = CARTESIAN_POINT ( 'NONE',  ( 20.57812500061451644, 6.421520780324663323E-16, -5.243569643749999010 ) ) ;
#2225 = CARTESIAN_POINT ( 'NONE',  ( 21.93750000000000000, -2.886751345948130876, 4.999999999999996447 ) ) ;
#2226 = VERTEX_POINT ( 'NONE', #59675 ) ;
#2227 = CARTESIAN_POINT ( 'NONE',  ( 24.41250000000000142, 2.886751345948129099, -4.999999999999998224 ) ) ;
#2228 = CARTESIAN_POINT ( 'NONE',  ( 9.001249775931846008E-16, 19.52187500061451786, -25.09994784771203058 ) ) ;
#2229 = CARTESIAN_POINT ( 'NONE',  ( -3.756430356249999214, 19.69062499938548427, 27.83122392262697531 ) ) ;
#2230 = CARTESIAN_POINT ( 'NONE',  ( 27.44062500061451715, 6.054752690667223547, 3.707466751127219781E-16 ) ) ;
#2231 = CARTESIAN_POINT ( 'NONE',  ( 8.690625000614515372, -3.027376345333614438, 5.243569643749998122 ) ) ;
#2232 = CARTESIAN_POINT ( 'NONE',  ( 20.73750000122903359, -4.330127018922194537, 2.499999999999995559 ) ) ;
#2233 = CARTESIAN_POINT ( 'NONE',  ( 23.80312500061451786, 4.541064518000418104, -2.621784821874998173 ) ) ;
#2234 = CARTESIAN_POINT ( 'NONE',  ( 26.13749999999999929, -2.886751345948125991, -5.000000000000000000 ) ) ;
#2235 = CARTESIAN_POINT ( 'NONE',  ( 1.999999999999998668, 15.01250000122903394, -33.46410161513775705 ) ) ;
#2236 = CARTESIAN_POINT ( 'NONE',  ( 9.553125000614517859, 0.000000000000000000, 5.243569643749999010 ) ) ;
#2237 = VERTEX_POINT ( 'NONE', #13509 ) ;
#2238 = CARTESIAN_POINT ( 'NONE',  ( 25.11562500061451431, 3.027376345333613106, -5.243569643749998122 ) ) ;
#2239 = CARTESIAN_POINT ( 'NONE',  ( 7.828125000614517326, -4.541064518000419881, 2.621784821874995952 ) ) ;
#2240 = CARTESIAN_POINT ( 'NONE',  ( 13.88437500061451679, 5.824947211148865298E-16, -4.756430356249998326 ) ) ;
#2241 = FACE_OUTER_BOUND ( 'NONE', #15117, .T. ) ;
#2242 = CARTESIAN_POINT ( 'NONE',  ( 12.37500000000000000, 4.330127018922191873, 2.499999999999999556 ) ) ;
#2243 = CARTESIAN_POINT ( 'NONE',  ( 14.14687500061451786, -3.027376345333614438, 5.243569643749998122 ) ) ;
#2244 = CARTESIAN_POINT ( 'NONE',  ( 8.362500001229031810, 4.330127018922192761, -2.499999999999997780 ) ) ;
#2245 = CARTESIAN_POINT ( 'NONE',  ( 17.44687500061451857, -3.027376345333610441, -5.243569643749999898 ) ) ;
#2246 = CARTESIAN_POINT ( 'NONE',  ( 18.00000000000000355, -4.330127018922190985, -2.500000000000001332 ) ) ;
#2247 = CARTESIAN_POINT ( 'NONE',  ( 9.121875000614517504, 3.027376345333611329, 5.243569643749999010 ) ) ;
#2248 = CARTESIAN_POINT ( 'NONE',  ( -4.243569643749999898, 12.15312500061451573, -30.00000000000000000 ) ) ;
#2249 = CARTESIAN_POINT ( 'NONE',  ( -0.7368881354385758975, 9.803648613939513368, 25.82089971438751519 ) ) ;
#2250 = CARTESIAN_POINT ( 'NONE',  ( 23.93437500061451573, -2.746126346562646425, 4.756430356249996549 ) ) ;
#2251 = ORIENTED_EDGE ( 'NONE', *, *, #16220, .T. ) ;
#2252 = EDGE_CURVE ( 'NONE', #8622, #23877, #8520, .T. ) ;
#2253 = CARTESIAN_POINT ( 'NONE',  ( 23.35312500061451857, 4.541064518000418104, -2.621784821874998173 ) ) ;
#2254 = CARTESIAN_POINT ( 'NONE',  ( 26.43750000000000355, -2.886751345948143310, 4.999999999999972466 ) ) ;
#2255 = CARTESIAN_POINT ( 'NONE',  ( 25.62187500061451573, 3.027376345333613106, -5.243569643749998122 ) ) ;
#2256 = CARTESIAN_POINT ( 'NONE',  ( 28.32187500061451502, 3.027376345333613106, -5.243569643749998122 ) ) ;
#2257 =( BOUNDED_CURVE ( )  B_SPLINE_CURVE ( 2, ( #19511, #64956, #8081, #42435, #36883, #59401, #8810 ),
 .UNSPECIFIED., .F., .F. ) 
 B_SPLINE_CURVE_WITH_KNOTS ( ( 3, 2, 2, 3 ),
 ( 0.2600000000000000644, 0.2633333333333333637, 0.2666666666666667185, 0.2700000000000000733 ),
 .UNSPECIFIED. ) 
 CURVE ( )  GEOMETRIC_REPRESENTATION_ITEM ( )  RATIONAL_B_SPLINE_CURVE ( ( 0.9999999999999977796, 0.8660254037844409281, 1.000000000000000000, 0.8660254037844387076, 1.000000000000000000, 0.8660254037844364872, 1.000000000000002220 ) ) 
 REPRESENTATION_ITEM ( '' )  );
#2258 = CARTESIAN_POINT ( 'NONE',  ( 21.48750000000000071, -2.886751345948129988, 4.999999999999997335 ) ) ;
#2259 = CARTESIAN_POINT ( 'NONE',  ( 7.453125000614516438, -4.541064518000417216, -2.621784821875001281 ) ) ;
#2260 = CARTESIAN_POINT ( 'NONE',  ( 23.52187500061451431, -4.119189519843968306, 2.378215178124996054 ) ) ;
#2261 = CARTESIAN_POINT ( 'NONE',  ( 15.57187500061451679, -6.054752690667223547, -1.112240025338166033E-15 ) ) ;
#2262 = CARTESIAN_POINT ( 'NONE',  ( 8.034375000614515372, 5.492252693125287522, 3.363034840372157021E-16 ) ) ;
#2263 = CARTESIAN_POINT ( 'NONE',  ( 3.553125000614516082, 4.541064518000418104, -2.621784821874998173 ) ) ;
#2264 = CARTESIAN_POINT ( 'NONE',  ( 8.446875000614518569, -3.027376345333610441, -5.243569643749999898 ) ) ;
#2265 = CARTESIAN_POINT ( 'NONE',  ( 19.13437500061451857, -4.541064518000419881, 2.621784821874995952 ) ) ;
#2266 = CARTESIAN_POINT ( 'NONE',  ( 27.41250000000000142, -5.773502691896255534, -1.060575238724906372E-15 ) ) ;
#2267 = CARTESIAN_POINT ( 'NONE',  ( 27.19687500061451857, -3.027376345333614438, 5.243569643749998122 ) ) ;
#2268 = CARTESIAN_POINT ( 'NONE',  ( 1.071796769724489895, 10.41740381056766473, -34.00000000000000000 ) ) ;
#2269 = EDGE_LOOP ( 'NONE', ( #54628, #66842, #1379, #38711 ) ) ;
#2270 = CARTESIAN_POINT ( 'NONE',  ( 11.17500000000000071, -4.330127018922194537, 2.499999999999995559 ) ) ;
#2271 = CARTESIAN_POINT ( 'NONE',  ( 11.37187500061451573, -4.119189519843968306, 2.378215178124996054 ) ) ;
#2272 = CARTESIAN_POINT ( 'NONE',  ( 22.11562500061451786, 3.027376345333611329, 5.243569643749999010 ) ) ;
#2273 = CARTESIAN_POINT ( 'NONE',  ( 11.02500000000000036, 4.330127018922191873, 2.499999999999999556 ) ) ;
#2274 = CARTESIAN_POINT ( 'NONE',  ( 9.000000001229034652, -2.886751345948129988, 4.999999999999997335 ) ) ;
#2275 = CARTESIAN_POINT ( 'NONE',  ( 7.078125000614516438, 6.421520780324663323E-16, -5.243569643749999010 ) ) ;
#2276 = CARTESIAN_POINT ( 'NONE',  ( 22.98749999999999716, -2.886751345948125991, -5.000000000000000000 ) ) ;
#2277 = CARTESIAN_POINT ( 'NONE',  ( 21.17812500061451431, 4.541064518000418104, 2.621784821874999949 ) ) ;
#2278 = CARTESIAN_POINT ( 'NONE',  ( 12.03749999999999964, -2.886751345948130876, 4.999999999999996447 ) ) ;
#2279 = CARTESIAN_POINT ( 'NONE',  ( 25.95000000122903216, 5.773502691896255534, 3.535250795749688894E-16 ) ) ;
#2280 = CARTESIAN_POINT ( 'NONE',  ( 1.878215178125000495, 20.36562499938548143, 26.74683588394047007 ) ) ;
#2281 = CARTESIAN_POINT ( 'NONE',  ( 4.237500000000001599, 5.773502691896255534, 3.535250795749688894E-16 ) ) ;
#2282 = EDGE_LOOP ( 'NONE', ( #16211, #35541, #8208, #37007 ) ) ;
#2283 = CARTESIAN_POINT ( 'NONE',  ( 20.31562500061451715, 3.027376345333611329, 5.243569643749999010 ) ) ;
#2284 = CARTESIAN_POINT ( 'NONE',  ( 27.32812500061451644, 6.421520780324663323E-16, -5.243569643749999010 ) ) ;
#2285 = CARTESIAN_POINT ( 'NONE',  ( 26.37187500061451217, -6.054752690667223547, -1.112240025338166033E-15 ) ) ;
#2286 = CARTESIAN_POINT ( 'NONE',  ( 14.50312500061451537, 0.000000000000000000, 5.243569643749999010 ) ) ;
#2287 = CARTESIAN_POINT ( 'NONE',  ( 28.64062500061451289, -3.027376345333610441, -5.243569643749999898 ) ) ;
#2288 = CARTESIAN_POINT ( 'NONE',  ( 7.828125000614517326, -4.541064518000419881, 2.621784821874995952 ) ) ;
#2289 = CARTESIAN_POINT ( 'NONE',  ( 4.711411573247316298, 1.674097066322985938, -4.711411573247316298 ) ) ;
#2290 = CARTESIAN_POINT ( 'NONE',  ( 26.77500000122903145, 2.886751345948129099, -4.999999999999998224 ) ) ;
#2291 = CARTESIAN_POINT ( 'NONE',  ( 19.50937500061451857, 0.000000000000000000, 4.756430356249998326 ) ) ;
#2292 = CARTESIAN_POINT ( 'NONE',  ( 16.56562500061451715, 3.027376345333612662, -5.243569643749998122 ) ) ;
#2293 = CARTESIAN_POINT ( 'NONE',  ( 8.025000000000000355, -4.330127018922194537, 2.499999999999995559 ) ) ;
#2294 = ADVANCED_FACE ( 'NONE', ( #20509 ), #58939, .F. ) ;
#2295 = CARTESIAN_POINT ( 'NONE',  ( 29.67187500061451644, 3.027376345333613106, -5.243569643749998122 ) ) ;
#2296 = CARTESIAN_POINT ( 'NONE',  ( 9.796875000614519990, -3.027376345333610441, -5.243569643749999898 ) ) ;
#2297 = CARTESIAN_POINT ( 'NONE',  ( 9.421875000614519990, 3.027376345333613106, -5.243569643749998122 ) ) ;
#2298 = CARTESIAN_POINT ( 'NONE',  ( 17.63437500061451502, 4.541064518000418104, 2.621784821874999949 ) ) ;
#2299 = ORIENTED_EDGE ( 'NONE', *, *, #58543, .T. ) ;
#2300 = CARTESIAN_POINT ( 'NONE',  ( 15.26249999999999929, -5.773502691896255534, -1.060575238724906372E-15 ) ) ;
#2301 = CARTESIAN_POINT ( 'NONE',  ( 21.21562500061451573, 3.027376345333611329, 5.243569643749999010 ) ) ;
#2302 = CARTESIAN_POINT ( 'NONE',  ( 15.57187500061451679, -6.054752690667223547, -1.112240025338166033E-15 ) ) ;
#2303 = CARTESIAN_POINT ( 'NONE',  ( 22.71562500061451573, -6.054752690667223547, -1.112240025338166033E-15 ) ) ;
#2304 = CARTESIAN_POINT ( 'NONE',  ( -1.999999999999997113, 13.32499999999999929, 33.46410161513775705 ) ) ;
#2305 = CARTESIAN_POINT ( 'NONE',  ( 3.234375000614516438, 4.541064518000418104, 2.621784821874999949 ) ) ;
#2306 = CARTESIAN_POINT ( 'NONE',  ( 8.512500001229033941, 0.000000000000000000, 4.999999999999998224 ) ) ;
#2307 = ORIENTED_EDGE ( 'NONE', *, *, #42591, .T. ) ;
#2308 = CARTESIAN_POINT ( 'NONE',  ( 4.837500001229035895, 4.330127018922191873, 2.499999999999999556 ) ) ;
#2309 = CARTESIAN_POINT ( 'NONE',  ( 8.484601909799253346E-16, 17.86250000000000071, -25.38119784648299770 ) ) ;
#2310 = CARTESIAN_POINT ( 'NONE',  ( 24.60000000122903430, 5.773502691896255534, 3.535250795749688894E-16 ) ) ;
#2311 = CARTESIAN_POINT ( 'NONE',  ( 3.756430356250000102, 13.20312499938548356, 30.00000000000000000 ) ) ;
#2312 = CARTESIAN_POINT ( 'NONE',  ( 8.184375000614515727, 4.541064518000418104, 2.621784821874999949 ) ) ;
#2313 = CARTESIAN_POINT ( 'NONE',  ( 24.37500000000000000, 6.123233995736764310E-16, -4.999999999999998224 ) ) ;
#2314 = CARTESIAN_POINT ( 'NONE',  ( 14.54062500061451679, -3.027376345333614438, 5.243569643749998122 ) ) ;
#2315 = CARTESIAN_POINT ( 'NONE',  ( 11.70937500061451608, 4.541064518000418104, -2.621784821874998173 ) ) ;
#2316 = CARTESIAN_POINT ( 'NONE',  ( 25.83750000122903501, 6.123233995736764310E-16, -4.999999999999998224 ) ) ;
#2317 = CARTESIAN_POINT ( 'NONE',  ( 17.97187500061451715, 3.027376345333612662, -5.243569643749998122 ) ) ;
#2318 = CARTESIAN_POINT ( 'NONE',  ( 6.459375000614518747, 0.000000000000000000, 5.243569643749999010 ) ) ;
#2319 = CARTESIAN_POINT ( 'NONE',  ( -2.498395430326213790E-14, 18.91249999999999787, 26.00000000000000000 ) ) ;
#2320 = CARTESIAN_POINT ( 'NONE',  ( 7.190625000614518036, 6.054752690667223547, 3.707466751127219781E-16 ) ) ;
#2321 = CARTESIAN_POINT ( 'NONE',  ( 18.36562500061451431, 3.027376345333613106, -5.243569643749998122 ) ) ;
#2322 = EDGE_LOOP ( 'NONE', ( #17460, #59592, #43723 ) ) ;
#2323 = CARTESIAN_POINT ( 'NONE',  ( 15.70312500061451644, 4.541064518000418104, -2.621784821874998173 ) ) ;
#2324 = CARTESIAN_POINT ( 'NONE',  ( 10.00312500061451715, 0.000000000000000000, 5.243569643749999010 ) ) ;
#2325 = CARTESIAN_POINT ( 'NONE',  ( 22.50937500061451857, 4.119189519843966529, -2.378215178124998275 ) ) ;
#2326 = CARTESIAN_POINT ( 'NONE',  ( 12.11250000000000249, -5.773502691896255534, -1.060575238724906372E-15 ) ) ;
#2327 = CARTESIAN_POINT ( 'NONE',  ( 6.900000001229035007, -2.886751345948125991, -5.000000000000000000 ) ) ;
#2328 = CARTESIAN_POINT ( 'NONE',  ( 14.37187500061451928, 3.027376345333613106, -5.243569643749998122 ) ) ;
#2329 = CARTESIAN_POINT ( 'NONE',  ( 16.16250000122903430, 0.000000000000000000, 4.999999999999998224 ) ) ;
#2330 = CARTESIAN_POINT ( 'NONE',  ( 24.07499999999999929, 4.330127018922191873, 2.499999999999999556 ) ) ;
#2331 = CARTESIAN_POINT ( 'NONE',  ( 4.243569643749999898, 19.12812500061451715, -30.00000000000000000 ) ) ;
#2332 = CARTESIAN_POINT ( 'NONE',  ( -1.999999999999999112, 13.10000000000000142, 26.53589838486224650 ) ) ;
#2333 = CARTESIAN_POINT ( 'NONE',  ( 4.898587196589411843E-16, 20.00000000000000000, 33.99999999999999289 ) ) ;
#2334 = CARTESIAN_POINT ( 'NONE',  ( 23.43750000122902932, -4.330127018922194537, 2.499999999999995559 ) ) ;
#2335 = CARTESIAN_POINT ( 'NONE',  ( 45.00000000000000000, 0.000000000000000000, 4.999999999999998224 ) ) ;
#2336 = FACE_OUTER_BOUND ( 'NONE', #2346, .T. ) ;
#2337 = CARTESIAN_POINT ( 'NONE',  ( 15.79687500061451821, 6.054752690667223547, 3.707466751127219781E-16 ) ) ;
#2338 = EDGE_CURVE ( 'NONE', #68777, #36937, #65592, .T. ) ;
#2339 = CARTESIAN_POINT ( 'NONE',  ( 29.62500000000000000, -4.330127018922194537, 2.499999999999995559 ) ) ;
#2340 = CARTESIAN_POINT ( 'NONE',  ( 13.82812500061451466, 6.421520780324663323E-16, -5.243569643749999010 ) ) ;
#2341 = CARTESIAN_POINT ( 'NONE',  ( 28.62187500061451217, 5.824947211148865298E-16, -4.756430356249998326 ) ) ;
#2342 = CARTESIAN_POINT ( 'NONE',  ( 23.29687500061451644, -3.027376345333610441, -5.243569643749999898 ) ) ;
#2343 = CARTESIAN_POINT ( 'NONE',  ( 16.17187500061451644, 4.119189519843966529, 2.378215178124999607 ) ) ;
#2344 = CARTESIAN_POINT ( 'NONE',  ( 9.253125000614517148, -4.541064518000417216, -2.621784821875001281 ) ) ;
#2345 = CARTESIAN_POINT ( 'NONE',  ( 15.30937500061451750, 4.541064518000418104, -2.621784821874998173 ) ) ;
#2346 = EDGE_LOOP ( 'NONE', ( #15475, #56072, #64393, #27480 ) ) ;
#2347 = CARTESIAN_POINT ( 'NONE',  ( 26.82187500061451857, -6.054752690667223547, -1.112240025338166033E-15 ) ) ;
#2348 = VECTOR ( 'NONE', #18941, 1000.000000000000000 ) ;
#2349 = CARTESIAN_POINT ( 'NONE',  ( 28.64062500061451289, -3.027376345333610441, -5.243569643749999898 ) ) ;
#2350 = CARTESIAN_POINT ( 'NONE',  ( 17.72812500061451502, -4.541064518000419881, 2.621784821874995952 ) ) ;
#2351 = CARTESIAN_POINT ( 'NONE',  ( 3.999999999999999112, 12.68750000122903465, -30.00000000000000000 ) ) ;
#2352 = CARTESIAN_POINT ( 'NONE',  ( 7.912499999999999645, 2.886751345948126879, 4.999999999999999112 ) ) ;
#2353 = CARTESIAN_POINT ( 'NONE',  ( 19.91250000122903074, -4.330127018922190985, -2.500000000000001332 ) ) ;
#2354 = DIRECTION ( 'NONE',  ( 0.000000000000000000, 0.000000000000000000, -1.000000000000000000 ) ) ;
#2355 = CARTESIAN_POINT ( 'NONE',  ( 11.40937500061451360, -5.492252693125287522, -1.008910452111647106E-15 ) ) ;
#2356 = VERTEX_POINT ( 'NONE', #8346 ) ;
#2357 = CARTESIAN_POINT ( 'NONE',  ( 17.28750000000000142, 5.773502691896255534, 3.535250795749688894E-16 ) ) ;
#2358 = CARTESIAN_POINT ( 'NONE',  ( 20.02500000000000213, 4.330127018922191873, 2.499999999999999556 ) ) ;
#2359 = CARTESIAN_POINT ( 'NONE',  ( 17.89687500061451431, -3.027376345333610441, -5.243569643749999898 ) ) ;
#2360 = CARTESIAN_POINT ( 'NONE',  ( 14.87812500061451537, 4.541064518000418104, 2.621784821874999949 ) ) ;
#2361 = ORIENTED_EDGE ( 'NONE', *, *, #36318, .T. ) ;
#2362 = DIRECTION ( 'NONE',  ( -1.000000000000000000, -0.000000000000000000, -0.000000000000000000 ) ) ;
#2363 = CARTESIAN_POINT ( 'NONE',  ( 6.740625000614516082, 6.054752690667223547, 3.707466751127219781E-16 ) ) ;
#2364 = CARTESIAN_POINT ( 'NONE',  ( 10.27499999999999858, -4.330127018922194537, 2.499999999999995559 ) ) ;
#2365 = CARTESIAN_POINT ( 'NONE',  ( 12.18750000000000000, -2.886751345948125991, -5.000000000000000000 ) ) ;
#2366 = CARTESIAN_POINT ( 'NONE',  ( 28.28437500061451360, 5.492252693125287522, 3.363034840372157021E-16 ) ) ;
#2367 = CARTESIAN_POINT ( 'NONE',  ( -4.243569643749999898, 14.81562500061451715, 27.54997392385601529 ) ) ;
#2368 = CARTESIAN_POINT ( 'NONE',  ( 26.35312500061451857, -4.541064518000417216, -2.621784821875001281 ) ) ;
#2369 = CARTESIAN_POINT ( 'NONE',  ( 8.062500000000000000, -5.773502691896255534, -1.060575238724906372E-15 ) ) ;
#2370 = CARTESIAN_POINT ( 'NONE',  ( -1.878215178125001827, 18.34062499938548285, 33.25316411605952283 ) ) ;
#2371 = CARTESIAN_POINT ( 'NONE',  ( 23.78437500061451360, 6.421520780324663323E-16, -5.243569643749999010 ) ) ;
#2372 = VERTEX_POINT ( 'NONE', #65221 ) ;
#2373 = CARTESIAN_POINT ( 'NONE',  ( 20.99062500061451431, -3.027376345333610441, -5.243569643749999898 ) ) ;
#2374 = CARTESIAN_POINT ( 'NONE',  ( 23.97187500061451360, 3.027376345333611329, 5.243569643749999010 ) ) ;
#2375 = CARTESIAN_POINT ( 'NONE',  ( -4.243569643749998122, 15.34062500061459389, -27.54997392385601174 ) ) ;
#2376 = CARTESIAN_POINT ( 'NONE',  ( 5.615625000614517859, -6.054752690667223547, -1.112240025338166033E-15 ) ) ;
#2377 = CARTESIAN_POINT ( 'NONE',  ( 27.90937500061451715, 4.119189519843966529, -2.378215178124998275 ) ) ;
#2378 = CARTESIAN_POINT ( 'NONE',  ( 24.21562500061451573, 3.027376345333612662, -5.243569643749998122 ) ) ;
#2379 = CARTESIAN_POINT ( 'NONE',  ( 10.54687500061451644, -2.746126346562646425, 4.756430356249996549 ) ) ;
#2380 = CARTESIAN_POINT ( 'NONE',  ( 3.756430356250000546, 16.27812499938548285, 27.83122392262697886 ) ) ;
#2381 = CARTESIAN_POINT ( 'NONE',  ( 17.10937500061451999, 4.541064518000418104, -2.621784821874998173 ) ) ;
#2382 = CARTESIAN_POINT ( 'NONE',  ( 24.94687500061451502, -3.027376345333614438, 5.243569643749998122 ) ) ;
#2383 = CARTESIAN_POINT ( 'NONE',  ( 2.121784821875001281, 14.15937500061451715, 33.67503911421598417 ) ) ;
#2384 = CARTESIAN_POINT ( 'NONE',  ( 8.578125000614518214, 4.541064518000418104, 2.621784821874999949 ) ) ;
#2385 = CARTESIAN_POINT ( 'NONE',  ( 16.42500000122903359, 2.886751345948129099, -4.999999999999997335 ) ) ;
#2386 = EDGE_CURVE ( 'NONE', #2494, #43350, #16995, .T. ) ;
#2387 = CARTESIAN_POINT ( 'NONE',  ( 29.46562500061451573, -6.054752690667223547, -1.112240025338166033E-15 ) ) ;
#2388 = CARTESIAN_POINT ( 'NONE',  ( -4.000000000000000888, 15.01250000000000107, 32.30940107675850470 ) ) ;
#2389 = CARTESIAN_POINT ( 'NONE',  ( 5.540625000614515905, -3.027376345333614438, 5.243569643749998122 ) ) ;
#2390 = CARTESIAN_POINT ( 'NONE',  ( 8.521875000614516082, 3.027376345333613106, -5.243569643749998122 ) ) ;
#2391 = CARTESIAN_POINT ( 'NONE',  ( 16.42500000122903359, 2.886751345948129099, -4.999999999999998224 ) ) ;
#2392 = CARTESIAN_POINT ( 'NONE',  ( 2.934375000614518392, -4.541064518000419881, 2.621784821874995952 ) ) ;
#2393 = CARTESIAN_POINT ( 'NONE',  ( 4.790625000614518569, -3.027376345333610441, -5.243569643749999898 ) ) ;
#2394 = CARTESIAN_POINT ( 'NONE',  ( 20.38125000122903430, 6.123233995736764310E-16, -4.999999999999998224 ) ) ;
#2395 = CARTESIAN_POINT ( 'NONE',  ( 16.39687500061451786, -3.027376345333614438, 5.243569643749998122 ) ) ;
#2396 = CARTESIAN_POINT ( 'NONE',  ( -2.000000000000000000, 10.47500000000000142, 26.53589838486224650 ) ) ;
#2397 = ORIENTED_EDGE ( 'NONE', *, *, #3296, .F. ) ;
#2398 = CARTESIAN_POINT ( 'NONE',  ( 21.74062500061451431, -3.027376345333614438, 5.243569643749998122 ) ) ;
#2399 = CARTESIAN_POINT ( 'NONE',  ( 9.365625000614519635, 3.027376345333613106, -5.243569643749998122 ) ) ;
#2400 = CARTESIAN_POINT ( 'NONE',  ( 26.10937500061451644, 4.541064518000418104, -2.621784821874998173 ) ) ;
#2401 = CARTESIAN_POINT ( 'NONE',  ( 9.965625000614517504, 3.027376345333611329, 5.243569643749999010 ) ) ;
#2402 = CARTESIAN_POINT ( 'NONE',  ( 3.397178649298551179, 3.668675132081069101, -3.397178649298551179 ) ) ;
#2403 = CARTESIAN_POINT ( 'NONE',  ( 9.337500001229033231, 4.330127018922191873, 2.499999999999999556 ) ) ;
#2404 = CARTESIAN_POINT ( 'NONE',  ( 24.17812500061451786, 6.421520780324663323E-16, -5.243569643749999010 ) ) ;
#2405 = CARTESIAN_POINT ( 'NONE',  ( 2.121784821875001281, 10.50312500061451715, -26.32496088578401938 ) ) ;
#2406 = CARTESIAN_POINT ( 'NONE',  ( 13.83750000122903323, 4.330127018922191873, 2.499999999999999556 ) ) ;
#2407 = CARTESIAN_POINT ( 'NONE',  ( 21.77812500061451928, -4.541064518000419881, 2.621784821874995952 ) ) ;
#2408 = CARTESIAN_POINT ( 'NONE',  ( 18.14062500061451644, -3.027376345333614438, 5.243569643749998122 ) ) ;
#2409 = CARTESIAN_POINT ( 'NONE',  ( 5.521875000614517859, 3.027376345333611329, 5.243569643749999010 ) ) ;
#2410 = CARTESIAN_POINT ( 'NONE',  ( 19.23749999999999716, -2.886751345948129988, 4.999999999999997335 ) ) ;
#2411 = CARTESIAN_POINT ( 'NONE',  ( 12.82500000122903394, 2.886751345948129099, -4.999999999999998224 ) ) ;
#2412 = CARTESIAN_POINT ( 'NONE',  ( 11.20312500061451644, 4.541064518000418104, -2.621784821874998173 ) ) ;
#2413 = CARTESIAN_POINT ( 'NONE',  ( 13.07812500061451821, 4.541064518000418104, 2.621784821874999949 ) ) ;
#2414 = CARTESIAN_POINT ( 'NONE',  ( 22.83750000122903501, 4.330127018922191873, 2.499999999999999556 ) ) ;
#2415 = CARTESIAN_POINT ( 'NONE',  ( 20.67187500061451289, 3.027376345333613106, -5.243569643749998122 ) ) ;
#2416 = CARTESIAN_POINT ( 'NONE',  ( 22.02187500061452141, 3.027376345333613106, -5.243569643749998122 ) ) ;
#2417 = CARTESIAN_POINT ( 'NONE',  ( 45.00000000000000000, 0.000000000000000000, 0.000000000000000000 ) ) ;
#2418 = CARTESIAN_POINT ( 'NONE',  ( 8.437500001229034652, 4.330127018922191873, 2.499999999999999556 ) ) ;
#2419 = CARTESIAN_POINT ( 'NONE',  ( 6.421875000614519102, 3.027376345333611329, 5.243569643749999010 ) ) ;
#2420 = CARTESIAN_POINT ( 'NONE',  ( 24.79687500061451999, 6.054752690667223547, 3.707466751127219781E-16 ) ) ;
#2421 = CARTESIAN_POINT ( 'NONE',  ( 45.00000000000000000, 6.123233995736764310E-16, -4.999999999999998224 ) ) ;
#2422 = CARTESIAN_POINT ( 'NONE',  ( 20.91562500061451502, -6.054752690667223547, -1.112240025338166033E-15 ) ) ;
#2423 = CARTESIAN_POINT ( 'NONE',  ( 25.69687500061451502, 6.054752690667223547, 3.707466751127219781E-16 ) ) ;
#2424 = CARTESIAN_POINT ( 'NONE',  ( 3.756430356250000102, 17.25312499938548072, 30.00000000000000000 ) ) ;
#2425 = CARTESIAN_POINT ( 'NONE',  ( 18.63749999999999929, 5.773502691896255534, 3.535250795749688401E-16 ) ) ;
#2426 = DIRECTION ( 'NONE',  ( -1.000000000000000000, -0.000000000000000000, -0.000000000000000000 ) ) ;
#2427 = CARTESIAN_POINT ( 'NONE',  ( 6.609375000614519102, -4.541064518000417216, -2.621784821875001281 ) ) ;
#2428 = CARTESIAN_POINT ( 'NONE',  ( 16.60312500061451857, 4.541064518000418104, -2.621784821874998173 ) ) ;
#2429 = ORIENTED_EDGE ( 'NONE', *, *, #69330, .T. ) ;
#2430 = CARTESIAN_POINT ( 'NONE',  ( 22.94999999999999929, -4.330127018922190985, -2.500000000000001332 ) ) ;
#2431 = CARTESIAN_POINT ( 'NONE',  ( 25.04062500061451502, -3.027376345333610441, -5.243569643749999898 ) ) ;
#2432 = CARTESIAN_POINT ( 'NONE',  ( 3.046875000614519990, -3.027376345333610441, -5.243569643749999898 ) ) ;
#2433 = CARTESIAN_POINT ( 'NONE',  ( 27.58125000122903359, 6.123233995736764310E-16, -4.999999999999998224 ) ) ;
#2434 = CYLINDRICAL_SURFACE ( 'NONE', #62037, 5.999999999999998224 ) ;
#2435 = CARTESIAN_POINT ( 'NONE',  ( 16.27499999999999858, 6.123233995736764310E-16, -4.999999999999998224 ) ) ;
#2436 = CARTESIAN_POINT ( 'NONE',  ( 20.05312500061451431, -4.541064518000417216, -2.621784821875001281 ) ) ;
#2437 = ORIENTED_EDGE ( 'NONE', *, *, #32834, .F. ) ;
#2438 = CARTESIAN_POINT ( 'NONE',  ( 25.12499999999999645, -4.330127018922194537, 2.499999999999995559 ) ) ;
#2439 = CARTESIAN_POINT ( 'NONE',  ( 25.09687500061451715, -3.027376345333610441, -5.243569643749999898 ) ) ;
#2440 = ORIENTED_EDGE ( 'NONE', *, *, #36141, .F. ) ;
#2441 = CARTESIAN_POINT ( 'NONE',  ( 25.94999999999999929, 0.000000000000000000, 4.999999999999998224 ) ) ;
#2442 = CARTESIAN_POINT ( 'NONE',  ( 14.01562500061451644, 3.027376345333611329, 5.243569643749999010 ) ) ;
#2443 = CARTESIAN_POINT ( 'NONE',  ( 6.590625000614518392, -3.027376345333610441, -5.243569643749999898 ) ) ;
#2444 = CARTESIAN_POINT ( 'NONE',  ( 16.09687500061451715, 4.119189519843966529, -2.378215178124998275 ) ) ;
#2445 = CARTESIAN_POINT ( 'NONE',  ( 28.52812500061451573, -4.541064518000419881, 2.621784821874995952 ) ) ;
#2446 = CARTESIAN_POINT ( 'NONE',  ( 14.55000000122903181, -2.886751345948125991, -5.000000000000000000 ) ) ;
#2447 = CARTESIAN_POINT ( 'NONE',  ( 19.08750000000000213, 5.773502691896255534, 3.535250795749688894E-16 ) ) ;
#2448 = CARTESIAN_POINT ( 'NONE',  ( 26.06250000000000000, -5.773502691896255534, -1.060575238724906372E-15 ) ) ;
#2449 = CARTESIAN_POINT ( 'NONE',  ( 2.896875000614518747, -3.027376345333614438, 5.243569643749998122 ) ) ;
#2450 = CARTESIAN_POINT ( 'NONE',  ( 8.521875000614516082, 3.027376345333613106, -5.243569643749998122 ) ) ;
#2451 = CARTESIAN_POINT ( 'NONE',  ( 19.09687500061451360, -3.027376345333614438, 5.243569643749998122 ) ) ;
#2452 = CYLINDRICAL_SURFACE ( 'NONE', #69010, 4.999999999999998224 ) ;
#2453 = EDGE_LOOP ( 'NONE', ( #8138, #56982, #51535, #7010, #49708, #2581 ) ) ;
#2454 = CARTESIAN_POINT ( 'NONE',  ( 29.61562500061451431, 3.027376345333613106, -5.243569643749998122 ) ) ;
#2455 = CARTESIAN_POINT ( 'NONE',  ( 29.85937500061451644, 0.000000000000000000, 5.243569643749999010 ) ) ;
#2456 = CARTESIAN_POINT ( 'NONE',  ( 5.334375000614517859, 6.421520780324663323E-16, -5.243569643749999010 ) ) ;
#2457 = CARTESIAN_POINT ( 'NONE',  ( 16.38749999999999929, 5.773502691896255534, 3.535250795749688894E-16 ) ) ;
#2458 = CARTESIAN_POINT ( 'NONE',  ( 14.54062500061451679, -3.027376345333614438, 5.243569643749998122 ) ) ;
#2459 = CARTESIAN_POINT ( 'NONE',  ( 9.356250001229033941, 0.000000000000000000, 4.999999999999998224 ) ) ;
#2460 = CARTESIAN_POINT ( 'NONE',  ( 14.13750000000000107, 5.773502691896255534, 3.535250795749688401E-16 ) ) ;
#2461 = CARTESIAN_POINT ( 'NONE',  ( 45.00000000000000000, 6.123233995736764310E-16, -4.999999999999998224 ) ) ;
#2462 = CARTESIAN_POINT ( 'NONE',  ( 18.22500000122903430, 2.886751345948129099, -4.999999999999998224 ) ) ;
#2463 = CARTESIAN_POINT ( 'NONE',  ( 27.35625000122903216, 0.000000000000000000, 4.999999999999998224 ) ) ;
#2464 = CARTESIAN_POINT ( 'NONE',  ( 17.78437500061451715, -4.119189519843968306, 2.378215178124996054 ) ) ;
#2465 = CARTESIAN_POINT ( 'NONE',  ( 8.353125000614518569, -4.541064518000417216, -2.621784821875001281 ) ) ;
#2466 = CARTESIAN_POINT ( 'NONE',  ( 23.82187500061451502, 3.027376345333613106, -5.243569643749998122 ) ) ;
#2467 = DIRECTION ( 'NONE',  ( -1.000000000000000000, -0.000000000000000000, -0.000000000000000000 ) ) ;
#2468 = CARTESIAN_POINT ( 'NONE',  ( 23.59687500061451715, -3.027376345333614438, 5.243569643749998122 ) ) ;
#2469 = CARTESIAN_POINT ( 'NONE',  ( 4.800000000000002487, 0.000000000000000000, 4.999999999999998224 ) ) ;
#2470 = CARTESIAN_POINT ( 'NONE',  ( 8.484601909799253346E-16, 9.875000001229032875, 34.61880215351700230 ) ) ;
#2471 = CARTESIAN_POINT ( 'NONE',  ( 13.56562500061451892, 3.027376345333611329, 5.243569643749999010 ) ) ;
#2472 = CARTESIAN_POINT ( 'NONE',  ( 5.700000001229033941, 5.773502691896255534, 3.535250795749688894E-16 ) ) ;
#2473 = EDGE_CURVE ( 'NONE', #22068, #71409, #47880, .T. ) ;
#2474 = CARTESIAN_POINT ( 'NONE',  ( 9.946875000614516793, 6.054752690667223547, 3.707466751127219781E-16 ) ) ;
#2475 = EDGE_LOOP ( 'NONE', ( #65961, #44078, #25078, #64122 ) ) ;
#2476 = CARTESIAN_POINT ( 'NONE',  ( 12.36562500061451608, -6.054752690667223547, -1.112240025338166033E-15 ) ) ;
#2477 = CARTESIAN_POINT ( 'NONE',  ( 13.95000000000000107, -4.330127018922190985, -2.500000000000001332 ) ) ;
#2478 = CARTESIAN_POINT ( 'NONE',  ( 23.66250000122903430, 4.330127018922192761, -2.499999999999997780 ) ) ;
#2479 = CARTESIAN_POINT ( 'NONE',  ( 11.10937500061451644, -4.541064518000417216, -2.621784821875001281 ) ) ;
#2480 = CARTESIAN_POINT ( 'NONE',  ( 15.77812500061451573, 4.541064518000418104, 2.621784821874999949 ) ) ;
#2481 = CARTESIAN_POINT ( 'NONE',  ( 27.61875000122903145, 2.886751345948129099, -4.999999999999998224 ) ) ;
#2482 = CARTESIAN_POINT ( 'NONE',  ( 23.07187500061451857, 3.027376345333611329, 5.243569643749999010 ) ) ;
#2483 = DIRECTION ( 'NONE',  ( -0.000000000000000000, -1.000000000000000000, -0.000000000000000000 ) ) ;
#2484 = CARTESIAN_POINT ( 'NONE',  ( 23.85000000000000142, -4.330127018922190985, -2.500000000000001332 ) ) ;
#2485 = CARTESIAN_POINT ( 'NONE',  ( -3.000416591977282496E-16, 15.69687500061451857, -34.90005215228797653 ) ) ;
#2486 = AXIS2_PLACEMENT_3D ( 'NONE', #65684, #36513, #25430 ) ;
#2487 = CARTESIAN_POINT ( 'NONE',  ( 15.75937500061451857, 4.541064518000418104, -2.621784821874998173 ) ) ;
#2488 = CARTESIAN_POINT ( 'NONE',  ( 17.36250000122903359, 4.330127018922192761, -2.499999999999997780 ) ) ;
#2489 =( BOUNDED_CURVE ( )  B_SPLINE_CURVE ( 2, ( #30575, #49036, #20939, #70093, #37570, #19840, #48300, #42754, #59728 ),
 .UNSPECIFIED., .F., .F. ) 
 B_SPLINE_CURVE_WITH_KNOTS ( ( 3, 2, 2, 2, 3 ),
 ( 0.2065217391304347838, 0.2101449275362318736, 0.2173913043478260809, 0.2246376811594202882, 0.2282608695652174058 ),
 .UNSPECIFIED. ) 
 CURVE ( )  GEOMETRIC_REPRESENTATION_ITEM ( )  RATIONAL_B_SPLINE_CURVE ( ( 0.9330127018922194093, 0.9330127018922194093, 1.000000000000000000, 0.8660254037844387076, 1.000000000000000000, 0.8660254037844387076, 1.000000000000000000, 0.9330127018922190762, 0.9330127018922194093 ) ) 
 REPRESENTATION_ITEM ( '' )  );
#2490 = CARTESIAN_POINT ( 'NONE',  ( 11.74687500061451573, 6.054752690667223547, 3.707466751127219781E-16 ) ) ;
#2491 = CARTESIAN_POINT ( 'NONE',  ( -2.121784821874999949, 17.47812500061451502, -33.67503911421598417 ) ) ;
#2492 = CARTESIAN_POINT ( 'NONE',  ( 20.70000000122903216, -2.886751345948129988, 4.999999999999997335 ) ) ;
#2493 = CARTESIAN_POINT ( 'NONE',  ( 12.77812500061451750, -4.541064518000419881, 2.621784821874995952 ) ) ;
#2494 = VERTEX_POINT ( 'NONE', #19046 ) ;
#2495 = ORIENTED_EDGE ( 'NONE', *, *, #9420, .F. ) ;
#2496 = CARTESIAN_POINT ( 'NONE',  ( 18.59999999999999787, 4.330127018922192761, -2.499999999999997780 ) ) ;
#2497 = CARTESIAN_POINT ( 'NONE',  ( 19.27500000122903145, 2.886751345948093572, 5.000000000000056843 ) ) ;
#2498 = CARTESIAN_POINT ( 'NONE',  ( 13.20937500061451786, 0.000000000000000000, 5.243569643749999010 ) ) ;
#2499 = CARTESIAN_POINT ( 'NONE',  ( 22.53750000000000142, -2.886751345948159742, -4.999999999999942268 ) ) ;
#2500 = PRODUCT_DEFINITION ( 'UNKNOWN', '', #41496, #8500 ) ;
#2501 = CARTESIAN_POINT ( 'NONE',  ( 12.90000000122903145, 5.773502691896255534, 3.535250795749688894E-16 ) ) ;
#2502 = CARTESIAN_POINT ( 'NONE',  ( 20.51250000122903216, 4.330127018922192761, -2.499999999999997780 ) ) ;
#2503 = CARTESIAN_POINT ( 'NONE',  ( 18.51562500061451289, 3.027376345333611329, 5.243569643749999010 ) ) ;
#2504 = CARTESIAN_POINT ( 'NONE',  ( 20.72812500061451502, 4.541064518000418104, 2.621784821874999949 ) ) ;
#2505 = CARTESIAN_POINT ( 'NONE',  ( 28.83750000122903145, -4.330127018922194537, 2.499999999999995559 ) ) ;
#2506 = CARTESIAN_POINT ( 'NONE',  ( 28.42499999999999716, 6.123233995736764310E-16, -4.999999999999998224 ) ) ;
#2507 = CYLINDRICAL_SURFACE ( 'NONE', #47800, 3.999999999999996447 ) ;
#2508 = CARTESIAN_POINT ( 'NONE',  ( 7.959375000614516971, -4.119189519843965641, -2.378215178125001383 ) ) ;
#2509 = CARTESIAN_POINT ( 'NONE',  ( 27.04687500061451644, 6.054752690667223547, 3.707466751127219781E-16 ) ) ;
#2510 = CARTESIAN_POINT ( 'NONE',  ( 1.626862140677534273E-15, 14.26250000000000107, -26.00000000000000355 ) ) ;
#2511 = AXIS2_PLACEMENT_3D ( 'NONE', #7, #11071, #28074 ) ;
#2512 = CARTESIAN_POINT ( 'NONE',  ( 4.243569643749999898, 16.03437500061451715, -30.00000000000000000 ) ) ;
#2513 = CARTESIAN_POINT ( 'NONE',  ( 30.00000000000000000, 0.000000000000000000, 4.999999999999998224 ) ) ;
#2514 = CARTESIAN_POINT ( 'NONE',  ( 5.549999999999998934, 4.330127018922192761, -2.499999999999997780 ) ) ;
#2515 = EDGE_CURVE ( 'NONE', #24010, #53411, #49114, .T. ) ;
#2516 = CARTESIAN_POINT ( 'NONE',  ( 16.46249999999999858, 2.886751345948126879, 4.999999999999998224 ) ) ;
#2517 = CARTESIAN_POINT ( 'NONE',  ( 9.196875000614518569, -3.027376345333614438, 5.243569643749998122 ) ) ;
#2518 = CARTESIAN_POINT ( 'NONE',  ( 29.42812500061451431, -4.541064518000419881, 2.621784821874995952 ) ) ;
#2520 = EDGE_CURVE ( 'NONE', #7627, #10804, #55613, .T. ) ;
#2519 = CYLINDRICAL_SURFACE ( 'NONE', #71610, 4.999999999999998224 ) ;
#2521 = CARTESIAN_POINT ( 'NONE',  ( -2.699902572705014769, 9.635935948006318696, -24.62716651635609466 ) ) ;
#2522 = CARTESIAN_POINT ( 'NONE',  ( 30.00000000000000000, 0.000000000000000000, 0.000000000000000000 ) ) ;
#2523 = CARTESIAN_POINT ( 'NONE',  ( 6.721875000614518925, 3.027376345333613106, -5.243569643749998122 ) ) ;
#2524 = CARTESIAN_POINT ( 'NONE',  ( 11.52187500061451608, -6.054752690667223547, -1.112240025338166033E-15 ) ) ;
#2525 = CARTESIAN_POINT ( 'NONE',  ( 4.349999999999999645, 0.000000000000000000, 4.999999999999998224 ) ) ;
#2526 = CARTESIAN_POINT ( 'NONE',  ( 9.001249775931846008E-16, 15.41562500061459495, 34.90005215228797653 ) ) ;
#2528 = EDGE_CURVE ( 'NONE', #43803, #16272, #67039, .T. ) ;
#2527 = CARTESIAN_POINT ( 'NONE',  ( 1.039375613666550624, 25.50811497328423982, 26.12855575835990152 ) ) ;
#2529 = CARTESIAN_POINT ( 'NONE',  ( 7.237500000000000711, -2.886751345948125991, -5.000000000000000000 ) ) ;
#2530 = CARTESIAN_POINT ( 'NONE',  ( 14.10937500061451644, -5.492252693125287522, -1.008910452111647106E-15 ) ) ;
#2531 = CARTESIAN_POINT ( 'NONE',  ( 20.24062500061451431, 6.054752690667223547, 3.707466751127219781E-16 ) ) ;
#2532 = CARTESIAN_POINT ( 'NONE',  ( 13.07812500061451821, 4.541064518000418104, 2.621784821874999949 ) ) ;
#2533 = CARTESIAN_POINT ( 'NONE',  ( 23.93437500061451573, -2.746126346562646425, 4.756430356249996549 ) ) ;
#2534 = CARTESIAN_POINT ( 'NONE',  ( 9.534375000614517148, 4.541064518000418104, 2.621784821874999949 ) ) ;
#2535 = CARTESIAN_POINT ( 'NONE',  ( 25.94999999999999929, 0.000000000000000000, 4.999999999999998224 ) ) ;
#2536 = CARTESIAN_POINT ( 'NONE',  ( 21.86250000122903003, 4.330127018922192761, -2.499999999999997780 ) ) ;
#2537 = CARTESIAN_POINT ( 'NONE',  ( 1.071796769724491893, 10.79509619066136850, 33.99999999999999289 ) ) ;
#2538 = CARTESIAN_POINT ( 'NONE',  ( 8.596875000614518925, 6.054752690667223547, 3.707466751127219781E-16 ) ) ;
#2539 = CARTESIAN_POINT ( 'NONE',  ( 27.42187500061451644, 3.027376345333613106, -5.243569643749998122 ) ) ;
#2540 = EDGE_CURVE ( 'NONE', #17100, #25696, #24047, .T. ) ;
#2541 = CARTESIAN_POINT ( 'NONE',  ( 23.43750000000000000, -2.886751345948153968, -4.999999999999952038 ) ) ;
#2542 = CARTESIAN_POINT ( 'NONE',  ( 45.00000000000000000, 0.000000000000000000, 0.000000000000000000 ) ) ;
#2543 = CARTESIAN_POINT ( 'NONE',  ( 19.20937500061451786, -4.541064518000417216, -2.621784821875001281 ) ) ;
#2544 = CARTESIAN_POINT ( 'NONE',  ( 10.84687500061451892, 6.054752690667223547, 3.707466751127219781E-16 ) ) ;
#2545 = CARTESIAN_POINT ( 'NONE',  ( -7.967954043666661671E-16, 12.97812499938548392, 34.33755215474603517 ) ) ;
#2546 = CARTESIAN_POINT ( 'NONE',  ( 22.27499999999999858, 4.330127018922191873, 2.499999999999999556 ) ) ;
#2547 = CARTESIAN_POINT ( 'NONE',  ( -7.967954043666661671E-16, 19.72812499938548214, 34.33755215474603517 ) ) ;
#2548 = CARTESIAN_POINT ( 'NONE',  ( -4.243569643749999898, 13.10937500061451821, -30.00000000000000000 ) ) ;
#2549 = CARTESIAN_POINT ( 'NONE',  ( 23.74687500061451573, -2.746126346562642428, -4.756430356249999214 ) ) ;
#2550 = CARTESIAN_POINT ( 'NONE',  ( 15.89062500061451289, -3.027376345333614438, 5.243569643749998122 ) ) ;
#2551 = CARTESIAN_POINT ( 'NONE',  ( 5.175000000000002487, 4.330127018922191873, 2.499999999999999556 ) ) ;
#2552 = CARTESIAN_POINT ( 'NONE',  ( 12.30000000122903359, -2.886751345948193048, -4.999999999999883649 ) ) ;
#2553 = CARTESIAN_POINT ( 'NONE',  ( 50.00000000000000000, -5.218601775200058412, 7.332543590861138938 ) ) ;
#2554 = CARTESIAN_POINT ( 'NONE',  ( 13.57500000000000107, 6.123233995736764310E-16, -4.999999999999998224 ) ) ;
#2555 = CARTESIAN_POINT ( 'NONE',  ( 2.121784821874999061, 11.10312500061451679, 26.32496088578401583 ) ) ;
#2556 = CARTESIAN_POINT ( 'NONE',  ( 14.06250000122903288, -4.330127018922190985, -2.500000000000001332 ) ) ;
#2557 = CARTESIAN_POINT ( 'NONE',  ( 24.83437500061451431, 4.541064518000418104, 2.621784821874999949 ) ) ;
#2558 = VERTEX_POINT ( 'NONE', #72607 ) ;
#2559 = CARTESIAN_POINT ( 'NONE',  ( 19.52812500061451573, -4.541064518000419881, 2.621784821874995952 ) ) ;
#2560 = CARTESIAN_POINT ( 'NONE',  ( 4.753125000614515372, -4.541064518000417216, -2.621784821875001281 ) ) ;
#2561 = CARTESIAN_POINT ( 'NONE',  ( 20.82187500061451857, 3.027376345333611329, 5.243569643749999010 ) ) ;
#2562 = CARTESIAN_POINT ( 'NONE',  ( 27.90937500061451715, 4.541064518000418104, -2.621784821874998173 ) ) ;
#2563 = CARTESIAN_POINT ( 'NONE',  ( 5.240625000614516971, -3.027376345333610441, -5.243569643749999898 ) ) ;
#2564 = CARTESIAN_POINT ( 'NONE',  ( 22.60312500061451857, 0.000000000000000000, 5.243569643749999010 ) ) ;
#2565 = CARTESIAN_POINT ( 'NONE',  ( 2.121784821874999061, 15.60312500061451857, 26.32496088578401583 ) ) ;
#2566 = CARTESIAN_POINT ( 'NONE',  ( 15.71250000122903501, 0.000000000000000000, 4.999999999999998224 ) ) ;
#2567 = CARTESIAN_POINT ( 'NONE',  ( 13.09687500061451537, 5.492252693125287522, 3.363034840372157021E-16 ) ) ;
#2568 = CARTESIAN_POINT ( 'NONE',  ( 7.603125000614517681, 4.541064518000418104, -2.621784821874998173 ) ) ;
#2569 = CARTESIAN_POINT ( 'NONE',  ( 13.61250000000000071, 2.886751345948129099, -4.999999999999997335 ) ) ;
#2570 = CARTESIAN_POINT ( 'NONE',  ( 29.01562500061451644, -6.054752690667223547, -1.112240025338166033E-15 ) ) ;
#2571 = CARTESIAN_POINT ( 'NONE',  ( 24.00937500061451502, 0.000000000000000000, 5.243569643749999010 ) ) ;
#2572 = CARTESIAN_POINT ( 'NONE',  ( 14.95312500061451644, 0.000000000000000000, 5.243569643749999010 ) ) ;
#2573 = ADVANCED_FACE ( 'NONE', ( #55978 ), #38994, .F. ) ;
#2574 = CARTESIAN_POINT ( 'NONE',  ( 25.65000000122903145, -2.886751345948129988, 4.999999999999997335 ) ) ;
#2575 = CARTESIAN_POINT ( 'NONE',  ( 24.66562500061451502, 3.027376345333613106, -5.243569643749998122 ) ) ;
#2576 = CARTESIAN_POINT ( 'NONE',  ( 20.33437500061451786, 4.541064518000418104, 2.621784821874999949 ) ) ;
#2577 = CARTESIAN_POINT ( 'NONE',  ( 14.50312500061451537, 0.000000000000000000, 5.243569643749999010 ) ) ;
#2578 = CARTESIAN_POINT ( 'NONE',  ( 9.001249775931846008E-16, 15.92187500061451821, 34.90005215228797653 ) ) ;
#2579 = CARTESIAN_POINT ( 'NONE',  ( 19.15312500061451573, -4.541064518000417216, -2.621784821875001281 ) ) ;
#2580 = CARTESIAN_POINT ( 'NONE',  ( -2.000000000000001776, 17.75000000000000355, 33.46410161513775705 ) ) ;
#2581 = ORIENTED_EDGE ( 'NONE', *, *, #44171, .F. ) ;
#2582 = CARTESIAN_POINT ( 'NONE',  ( 25.01249999999999929, 2.886751345948126879, 4.999999999999999112 ) ) ;
#2583 = CARTESIAN_POINT ( 'NONE',  ( 8.484601909799253346E-16, 11.56250000000000000, -25.38119784648299770 ) ) ;
#2584 = CARTESIAN_POINT ( 'NONE',  ( -3.756430356250000102, 19.72812499938548214, 30.00000000000000000 ) ) ;
#2585 = CARTESIAN_POINT ( 'NONE',  ( 26.80312500061451431, -4.541064518000417216, -2.621784821875001281 ) ) ;
#2586 = CARTESIAN_POINT ( 'NONE',  ( 7.040625000614517681, -3.027376345333610441, -5.243569643749999898 ) ) ;
#2587 = CARTESIAN_POINT ( 'NONE',  ( 20.51250000122903216, 4.330127018922192761, -2.499999999999997780 ) ) ;
#2588 = CARTESIAN_POINT ( 'NONE',  ( 25.11562500061451431, 3.027376345333613106, -5.243569643749998122 ) ) ;
#2589 = CARTESIAN_POINT ( 'NONE',  ( 25.87500000000000000, 4.330127018922191873, 2.499999999999999556 ) ) ;
#2590 = CARTESIAN_POINT ( 'NONE',  ( 3.999999999999998668, 16.32500000122903216, -32.30940107675850470 ) ) ;
#2591 = CARTESIAN_POINT ( 'NONE',  ( 26.80312500061451431, -4.541064518000417216, -2.621784821875001281 ) ) ;
#2592 = CARTESIAN_POINT ( 'NONE',  ( 8.390625000614518214, -3.027376345333610441, -5.243569643749999898 ) ) ;
#2593 = ORIENTED_EDGE ( 'NONE', *, *, #5826, .T. ) ;
#2594 = CARTESIAN_POINT ( 'NONE',  ( 24.55312500061451786, -4.541064518000417216, -2.621784821875001281 ) ) ;
#2595 = CARTESIAN_POINT ( 'NONE',  ( 4.565625000614516260, 3.027376345333611329, 5.243569643749999010 ) ) ;
#2596 = CARTESIAN_POINT ( 'NONE',  ( 13.80937500061451750, -4.119189519843965641, -2.378215178125001383 ) ) ;
#2597 = DIRECTION ( 'NONE',  ( -1.000000000000000000, -0.000000000000000000, -0.000000000000000000 ) ) ;
#2598 = CARTESIAN_POINT ( 'NONE',  ( 12.03749999999999964, -2.886751345948129988, 4.999999999999997335 ) ) ;
#2599 = CARTESIAN_POINT ( 'NONE',  ( 13.05937500061451750, 4.541064518000418104, -2.621784821874998173 ) ) ;
#2600 = CARTESIAN_POINT ( 'NONE',  ( 10.05000000122903181, -2.886751345948125991, -5.000000000000000000 ) ) ;
#2601 = CARTESIAN_POINT ( 'NONE',  ( 17.18437500061451573, 4.541064518000418104, 2.621784821874999949 ) ) ;
#2602 = CARTESIAN_POINT ( 'NONE',  ( 15.56250000000000000, 2.886751345948126879, 4.999999999999999112 ) ) ;
#2603 = CARTESIAN_POINT ( 'NONE',  ( 7.996875000614519280, -3.027376345333610441, -5.243569643749999898 ) ) ;
#2604 = CARTESIAN_POINT ( 'NONE',  ( -2.121784821874996840, 12.22812500061451857, -26.32496088578401583 ) ) ;
#2605 = CARTESIAN_POINT ( 'NONE',  ( -2.000000000000000000, 11.82500000000000107, -33.46410161513775705 ) ) ;
#2606 = CARTESIAN_POINT ( 'NONE',  ( 24.30937500061451573, 2.746126346562643317, 4.756430356249998326 ) ) ;
#2607 = CARTESIAN_POINT ( 'NONE',  ( 15.67500000000000071, -4.330127018922194537, 2.499999999999995559 ) ) ;
#2608 = CARTESIAN_POINT ( 'NONE',  ( 23.27812500061451573, 6.421520780324663323E-16, -5.243569643749999010 ) ) ;
#2609 = CARTESIAN_POINT ( 'NONE',  ( -2.121784821874999949, 10.33437500061451786, 26.32496088578401938 ) ) ;
#2610 = FACE_OUTER_BOUND ( 'NONE', #2282, .T. ) ;
#2611 = CARTESIAN_POINT ( 'NONE',  ( 25.02187500061451431, -6.054752690667223547, -1.112240025338166033E-15 ) ) ;
#2612 = EDGE_CURVE ( 'NONE', #22784, #32666, #1863, .T. ) ;
#2613 = CARTESIAN_POINT ( 'NONE',  ( 28.13437500061451502, -4.541064518000419881, 2.621784821874995952 ) ) ;
#2614 = CARTESIAN_POINT ( 'NONE',  ( 4.715625000614516615, -6.054752690667223547, -1.112240025338166033E-15 ) ) ;
#2615 = CARTESIAN_POINT ( 'NONE',  ( 21.42187500061451644, 5.824947211148865298E-16, -4.756430356249998326 ) ) ;
#2616 = CARTESIAN_POINT ( 'NONE',  ( 17.78437500061451715, -4.541064518000419881, 2.621784821874995952 ) ) ;
#2617 = CARTESIAN_POINT ( 'NONE',  ( 7.734375000614519102, -2.746126346562646425, 4.756430356249996549 ) ) ;
#2618 = CARTESIAN_POINT ( 'NONE',  ( 3.403125000614518836, -4.541064518000417216, -2.621784821875001281 ) ) ;
#2619 = CARTESIAN_POINT ( 'NONE',  ( 7.359375000614516438, 0.000000000000000000, 5.243569643749999010 ) ) ;
#2620 = CARTESIAN_POINT ( 'NONE',  ( 19.47187500061451360, 3.027376345333611329, 5.243569643749999010 ) ) ;
#2621 = CARTESIAN_POINT ( 'NONE',  ( 13.68750000122903288, 6.123233995736764310E-16, -4.999999999999998224 ) ) ;
#2622 = CARTESIAN_POINT ( 'NONE',  ( 25.76249999999999929, 2.886751345948129099, -4.999999999999998224 ) ) ;
#2623 = CARTESIAN_POINT ( 'NONE',  ( 26.82187500061451857, -6.054752690667223547, -1.112240025338166033E-15 ) ) ;
#2624 = CARTESIAN_POINT ( 'NONE',  ( -1.878215178124999163, 13.80312499938548321, 26.74683588394047007 ) ) ;
#2625 = CARTESIAN_POINT ( 'NONE',  ( 8.756250001229034297, 4.330127018922192761, -2.499999999999997780 ) ) ;
#2626 = ORIENTED_EDGE ( 'NONE', *, *, #70842, .F. ) ;
#2627 = CARTESIAN_POINT ( 'NONE',  ( 7.162500000000001421, -5.773502691896255534, -1.060575238724906372E-15 ) ) ;
#2628 = CARTESIAN_POINT ( 'NONE',  ( 9.834375000614514306, 5.492252693125287522, 3.363034840372157021E-16 ) ) ;
#2629 = CARTESIAN_POINT ( 'NONE',  ( 20.95312500061451999, -4.541064518000417216, -2.621784821875001281 ) ) ;
#2630 = CARTESIAN_POINT ( 'NONE',  ( 12.15000000000000036, -4.330127018922190985, -2.500000000000001332 ) ) ;
#2631 =( BOUNDED_CURVE ( )  B_SPLINE_CURVE ( 3, ( #61263, #54627, #16909, #26558 ),
 .UNSPECIFIED., .F., .F. ) 
 B_SPLINE_CURVE_WITH_KNOTS ( ( 4, 4 ),
 ( 3.141592653589793116, 4.712388980384689674 ),
 .UNSPECIFIED. ) 
 CURVE ( )  GEOMETRIC_REPRESENTATION_ITEM ( )  RATIONAL_B_SPLINE_CURVE ( ( 1.000000000000000000, 0.8047378541243649375, 0.8047378541243649375, 1.000000000000000000 ) ) 
 REPRESENTATION_ITEM ( '' )  );
#2632 = CARTESIAN_POINT ( 'NONE',  ( 9.337500001229033231, 4.330127018922191873, 2.499999999999999556 ) ) ;
#2633 = CARTESIAN_POINT ( 'NONE',  ( 5.540625000614515905, -3.027376345333614438, 5.243569643749998122 ) ) ;
#2634 = CARTESIAN_POINT ( 'NONE',  ( 21.11249999999999716, -5.773502691896255534, -1.060575238724906372E-15 ) ) ;
#2635 = CARTESIAN_POINT ( 'NONE',  ( 17.46562500061451217, 3.027376345333613106, -5.243569643749998122 ) ) ;
#2636 = CARTESIAN_POINT ( 'NONE',  ( 12.00000000000000000, 0.000000000000000000, 4.999999999999998224 ) ) ;
#2637 = AXIS2_PLACEMENT_3D ( 'NONE', #49337, #31609, #32707 ) ;
#2638 = CARTESIAN_POINT ( 'NONE',  ( 25.38750000122903216, 6.123233995736764310E-16, -4.999999999999998224 ) ) ;
#2639 = CARTESIAN_POINT ( 'NONE',  ( 3.756430356250000546, 18.52812499938548285, 27.83122392262697886 ) ) ;
#2640 = CARTESIAN_POINT ( 'NONE',  ( 6.225000000000001421, -4.330127018922194537, 2.499999999999995559 ) ) ;
#2641 = VERTEX_POINT ( 'NONE', #50445 ) ;
#2642 = CARTESIAN_POINT ( 'NONE',  ( 19.79062500061451502, 6.054752690667223547, 3.707466751127219781E-16 ) ) ;
#2643 = CARTESIAN_POINT ( 'NONE',  ( 25.94062500061451715, -3.027376345333610441, -5.243569643749999898 ) ) ;
#2644 = CARTESIAN_POINT ( 'NONE',  ( 27.68437500061451573, -4.541064518000419881, 2.621784821874995952 ) ) ;
#2645 = CARTESIAN_POINT ( 'NONE',  ( 8.099999999999999645, -4.330127018922190985, -2.500000000000001332 ) ) ;
#2646 = CARTESIAN_POINT ( 'NONE',  ( 13.60312500061451679, 0.000000000000000000, 5.243569643749999010 ) ) ;
#2647 = CARTESIAN_POINT ( 'NONE',  ( 29.65312500061451573, 4.541064518000418104, -2.621784821874998173 ) ) ;
#2648 = CARTESIAN_POINT ( 'NONE',  ( 9.440625000614517148, 6.054752690667223547, 3.707466751127219781E-16 ) ) ;
#2649 = CARTESIAN_POINT ( 'NONE',  ( 7.012500001229035718, 4.330127018922192761, -2.499999999999997780 ) ) ;
#2650 = CARTESIAN_POINT ( 'NONE',  ( 4.243569643749999898, 11.94687500061451857, 32.45002607614398471 ) ) ;
#2651 = EDGE_CURVE ( 'NONE', #53197, #48464, #51910, .T. ) ;
#2652 = CARTESIAN_POINT ( 'NONE',  ( 27.07500000122903216, -5.773502691896255534, -1.060575238724906372E-15 ) ) ;
#2653 = CARTESIAN_POINT ( 'NONE',  ( 20.18437500061451573, 5.824947211148865298E-16, -4.756430356249998326 ) ) ;
#2654 = CARTESIAN_POINT ( 'NONE',  ( 16.97812500061451502, 6.421520780324663323E-16, -5.243569643749999010 ) ) ;
#2655 = CARTESIAN_POINT ( 'NONE',  ( -1.071796769724496334, 15.33259618943233527, 26.00000000000000355 ) ) ;
#2656 = CARTESIAN_POINT ( 'NONE',  ( 10.65937500061451715, -4.541064518000417216, -2.621784821875001281 ) ) ;
#2657 = CARTESIAN_POINT ( 'NONE',  ( 10.32187500061451679, 3.027376345333613106, -5.243569643749998122 ) ) ;
#2658 = CARTESIAN_POINT ( 'NONE',  ( 17.29687500061451999, -3.027376345333614438, 5.243569643749998122 ) ) ;
#2659 = EDGE_LOOP ( 'NONE', ( #4142, #55837, #64847, #1422 ) ) ;
#2660 = CARTESIAN_POINT ( 'NONE',  ( 4.000000000000000000, 13.43750000000000000, 32.30940107675849760 ) ) ;
#2661 = CARTESIAN_POINT ( 'NONE',  ( 20.91562500061451502, -6.054752690667223547, -1.112240025338166033E-15 ) ) ;
#2662 = CARTESIAN_POINT ( 'NONE',  ( 16.62187500061451573, 3.027376345333613106, -5.243569643749998122 ) ) ;
#2663 = CARTESIAN_POINT ( 'NONE',  ( 21.32812500061451644, -4.541064518000419881, 2.621784821874995952 ) ) ;
#2664 = CARTESIAN_POINT ( 'NONE',  ( 2.000000000000001332, 15.20000000000000107, 33.46410161513774995 ) ) ;
#2665 = CARTESIAN_POINT ( 'NONE',  ( 27.40312500061451573, 4.541064518000418104, -2.621784821874998173 ) ) ;
#2666 = CARTESIAN_POINT ( 'NONE',  ( 8.212500001229035007, -4.330127018922190985, -2.500000000000001332 ) ) ;
#2667 = VERTEX_POINT ( 'NONE', #37882 ) ;
#2668 = CARTESIAN_POINT ( 'NONE',  ( 3.825000001229032609, 2.886751345948129099, -4.999999999999998224 ) ) ;
#2669 = CARTESIAN_POINT ( 'NONE',  ( -2.828200636599751609E-16, 18.08750000000000213, -34.61880215351700230 ) ) ;
#2670 = CARTESIAN_POINT ( 'NONE',  ( 25.72500000122903074, -5.773502691896255534, -1.060575238724906372E-15 ) ) ;
#2671 = CARTESIAN_POINT ( 'NONE',  ( -1.999999999999999112, 19.79374999877096286, 26.53589838486224650 ) ) ;
#2672 = CARTESIAN_POINT ( 'NONE',  ( 6.009375000614519458, 0.000000000000000000, 5.243569643749999010 ) ) ;
#2673 = CARTESIAN_POINT ( 'NONE',  ( 4.337544802671691180, 2.487292970951878956, -4.464402052312094860 ) ) ;
#2674 = EDGE_CURVE ( 'NONE', #33629, #44223, #22352, .T. ) ;
#2675 = CARTESIAN_POINT ( 'NONE',  ( 16.19062500061451715, 6.054752690667223547, 3.707466751127219781E-16 ) ) ;
#2676 = CARTESIAN_POINT ( 'NONE',  ( 8.484375000614518214, 6.421520780324663323E-16, -5.243569643749999010 ) ) ;
#2677 = CARTESIAN_POINT ( 'NONE',  ( 28.05000000122903359, -2.886751345948125991, -5.000000000000000000 ) ) ;
#2678 = CARTESIAN_POINT ( 'NONE',  ( 16.39687500061451786, -3.027376345333614438, 5.243569643749998122 ) ) ;
#2679 = CARTESIAN_POINT ( 'NONE',  ( 4.434375000614519280, 6.421520780324663323E-16, -5.243569643749999010 ) ) ;
#2680 = CARTESIAN_POINT ( 'NONE',  ( 3.999999999999999112, 16.28750000122903430, 30.00000000000000000 ) ) ;
#2681 = CARTESIAN_POINT ( 'NONE',  ( 6.253125000614517148, 4.541064518000418104, -2.621784821874998173 ) ) ;
#2682 = CARTESIAN_POINT ( 'NONE',  ( 17.01562500061451644, 3.027376345333613106, -5.243569643749998122 ) ) ;
#2683 = ORIENTED_EDGE ( 'NONE', *, *, #44097, .T. ) ;
#2684 = CARTESIAN_POINT ( 'NONE',  ( 13.64062500061451644, -3.027376345333614438, 5.243569643749998122 ) ) ;
#2685 = CARTESIAN_POINT ( 'NONE',  ( 6.375000001229031987, -5.773502691896255534, -1.060575238724906372E-15 ) ) ;
#2686 = CARTESIAN_POINT ( 'NONE',  ( 11.65312500061451573, 4.541064518000418104, -2.621784821874998173 ) ) ;
#2687 = CARTESIAN_POINT ( 'NONE',  ( 21.94687500061451857, -2.746126346562642428, -4.756430356249999214 ) ) ;
#2688 = CARTESIAN_POINT ( 'NONE',  ( 11.92500000000000071, 4.330127018922191873, 2.499999999999999556 ) ) ;
#2689 = CARTESIAN_POINT ( 'NONE',  ( 7.575000001229033053, 2.886751345948126879, 4.999999999999999112 ) ) ;
#2690 = EDGE_CURVE ( 'NONE', #33907, #58199, #16803, .T. ) ;
#2691 = CARTESIAN_POINT ( 'NONE',  ( 20.47500000000000142, 4.330127018922191873, 2.499999999999999556 ) ) ;
#2692 =( BOUNDED_CURVE ( )  B_SPLINE_CURVE ( 2, ( #60582, #27352, #3727, #72408, #21790, #4095, #55062 ),
 .UNSPECIFIED., .F., .F. ) 
 B_SPLINE_CURVE_WITH_KNOTS ( ( 3, 2, 2, 3 ),
 ( 0.8250000000000000666, 0.8277777777777778345, 0.8305555555555557135, 0.8333333333333334814 ),
 .UNSPECIFIED. ) 
 CURVE ( )  GEOMETRIC_REPRESENTATION_ITEM ( )  RATIONAL_B_SPLINE_CURVE ( ( 0.9999999999999946709, 0.8660254037844440367, 1.000000000000000000, 0.8660254037844387076, 1.000000000000000000, 0.8660254037844333785, 1.000000000000005329 ) ) 
 REPRESENTATION_ITEM ( '' )  );
#2693 = CARTESIAN_POINT ( 'NONE',  ( 15.49687500061451750, -3.027376345333614438, 5.243569643749998122 ) ) ;
#2694 = CARTESIAN_POINT ( 'NONE',  ( 14.92500000122903181, -5.773502691896255534, -1.060575238724906372E-15 ) ) ;
#2695 = CARTESIAN_POINT ( 'NONE',  ( 23.43750000000000000, -2.886751345948125991, -5.000000000000000000 ) ) ;
#2696 = CARTESIAN_POINT ( 'NONE',  ( -4.243569643749999898, 19.80312500061451786, -30.00000000000000000 ) ) ;
#2697 = CARTESIAN_POINT ( 'NONE',  ( 2.000000000000000444, 20.22500000000000142, 26.53589838486224650 ) ) ;
#2698 = CARTESIAN_POINT ( 'NONE',  ( 1.071796769724497445, 15.02990381179670010, -33.99999999999998579 ) ) ;
#2699 = CARTESIAN_POINT ( 'NONE',  ( 4.247151432104769420, -2.638504256727666863, 4.531370421416291983 ) ) ;
#2700 = DIRECTION ( 'NONE',  ( -0.000000000000000000, -1.000000000000000000, -0.000000000000000000 ) ) ;
#2701 = CARTESIAN_POINT ( 'NONE',  ( 18.73125000122903216, 4.330127018922191873, 2.499999999999999556 ) ) ;
#2702 = CARTESIAN_POINT ( 'NONE',  ( 16.84687500061451715, -3.027376345333614438, 5.243569643749998122 ) ) ;
#2703 = CARTESIAN_POINT ( 'NONE',  ( 29.51249999999999929, 2.886751345948126879, 4.999999999999999112 ) ) ;
#2704 = CARTESIAN_POINT ( 'NONE',  ( 12.36562500061451608, -6.054752690667223547, -1.112240025338166033E-15 ) ) ;
#2705 = CARTESIAN_POINT ( 'NONE',  ( 28.65937500061451715, 2.746126346562645981, -4.756430356249997438 ) ) ;
#2706 = CARTESIAN_POINT ( 'NONE',  ( 23.07187500061451857, 3.027376345333611329, 5.243569643749999010 ) ) ;
#2707 = CARTESIAN_POINT ( 'NONE',  ( 15.04687500061451466, -4.119189519843965641, -2.378215178125001383 ) ) ;
#2708 = CARTESIAN_POINT ( 'NONE',  ( 10.97812500061451679, -4.541064518000419881, 2.621784821874995952 ) ) ;
#2709 = CARTESIAN_POINT ( 'NONE',  ( 15.72187500061451892, 3.027376345333613106, -5.243569643749998122 ) ) ;
#2710 = ORIENTED_EDGE ( 'NONE', *, *, #35681, .F. ) ;
#2711 = CARTESIAN_POINT ( 'NONE',  ( 26.89687500061451431, -3.027376345333610441, -5.243569643749999898 ) ) ;
#2712 = CARTESIAN_POINT ( 'NONE',  ( 27.44062500061451715, 6.054752690667223547, 3.707466751127219781E-16 ) ) ;
#2713 = CARTESIAN_POINT ( 'NONE',  ( 18.74062500061451431, -3.027376345333610441, -5.243569643749999898 ) ) ;
#2714 = CARTESIAN_POINT ( 'NONE',  ( 27.66562500061451146, -6.054752690667223547, -1.112240025338166033E-15 ) ) ;
#2715 = LINE ( 'NONE', #59209, #27824 ) ;
#2716 = CARTESIAN_POINT ( 'NONE',  ( 7.800000000000001599, 4.330127018922192761, -2.499999999999997780 ) ) ;
#2717 = CARTESIAN_POINT ( 'NONE',  ( 18.56250000122903288, -4.330127018922190985, -2.500000000000001332 ) ) ;
#2718 = CARTESIAN_POINT ( 'NONE',  ( -1.999999999999997113, 18.83750000122903501, -26.53589838486224295 ) ) ;
#2719 = CARTESIAN_POINT ( 'NONE',  ( 7.546875000614516438, 4.119189519843966529, -2.378215178124998275 ) ) ;
#2720 = ORIENTED_EDGE ( 'NONE', *, *, #63166, .T. ) ;
#2721 = CARTESIAN_POINT ( 'NONE',  ( 15.37500000000000000, 6.123233995736764310E-16, -4.999999999999998224 ) ) ;
#2722 = CARTESIAN_POINT ( 'NONE',  ( 19.94999999999999929, 4.330127018922192761, -2.499999999999997780 ) ) ;
#2723 = CARTESIAN_POINT ( 'NONE',  ( 15.79687500061451821, 6.054752690667223547, 3.707466751127219781E-16 ) ) ;
#2724 = CARTESIAN_POINT ( 'NONE',  ( 14.16562500061451679, -6.054752690667223547, -1.112240025338166033E-15 ) ) ;
#2725 = ORIENTED_EDGE ( 'NONE', *, *, #54850, .T. ) ;
#2726 = LINE ( 'NONE', #20428, #1814 ) ;
#2727 = CARTESIAN_POINT ( 'NONE',  ( 4.243569643749999010, 16.07187500061451857, -32.45002607614398471 ) ) ;
#2728 = CARTESIAN_POINT ( 'NONE',  ( 5.765625000614519102, 3.027376345333613106, -5.243569643749998122 ) ) ;
#2729 = CARTESIAN_POINT ( 'NONE',  ( 3.756430356250000546, 12.67812499938548143, 27.83122392262697886 ) ) ;
#2730 = CARTESIAN_POINT ( 'NONE',  ( 12.15000000000000036, -4.330127018922190985, -2.500000000000001332 ) ) ;
#2731 = CARTESIAN_POINT ( 'NONE',  ( 29.48437500061451644, -2.746126346562642428, -4.756430356249999214 ) ) ;
#2732 = CARTESIAN_POINT ( 'NONE',  ( 4.243569643749999010, 14.21562500061451928, 27.54997392385601174 ) ) ;
#2733 = CARTESIAN_POINT ( 'NONE',  ( 26.05312500061451431, 4.541064518000418104, -2.621784821874998173 ) ) ;
#2734 = CARTESIAN_POINT ( 'NONE',  ( 9.112500000000000711, 2.886751345948129099, -4.999999999999998224 ) ) ;
#2735 = CARTESIAN_POINT ( 'NONE',  ( 3.756430356250000102, 16.69062499938548427, 30.00000000000000000 ) ) ;
#2736 = CARTESIAN_POINT ( 'NONE',  ( 24.08437500061451786, -4.541064518000419881, 2.621784821874995952 ) ) ;
#2737 = CARTESIAN_POINT ( 'NONE',  ( 20.57812500061451644, 6.421520780324663323E-16, -5.243569643749999010 ) ) ;
#2738 = CARTESIAN_POINT ( 'NONE',  ( -2.121784821874999949, 17.47812500061459318, -33.67503911421598417 ) ) ;
#2739 = CARTESIAN_POINT ( 'NONE',  ( 24.41250000122903430, -4.330127018922190985, -2.500000000000001332 ) ) ;
#2740 = CARTESIAN_POINT ( 'NONE',  ( 7.640625000614517326, 6.054752690667223547, 3.707466751127219781E-16 ) ) ;
#2741 = CARTESIAN_POINT ( 'NONE',  ( 26.93437500061451573, 5.824947211148865298E-16, -4.756430356249998326 ) ) ;
#2742 = CARTESIAN_POINT ( 'NONE',  ( 23.42812500061451786, 4.541064518000418104, 2.621784821874999949 ) ) ;
#2743 = CARTESIAN_POINT ( 'NONE',  ( 9.309375000614517504, -4.119189519843965641, -2.378215178125001383 ) ) ;
#2744 = CARTESIAN_POINT ( 'NONE',  ( -3.756430356250000102, 15.11562499938548321, 30.00000000000000000 ) ) ;
#2745 = CARTESIAN_POINT ( 'NONE',  ( 17.48437500061451999, 6.421520780324663323E-16, -5.243569643749999010 ) ) ;
#2746 = CARTESIAN_POINT ( 'NONE',  ( 24.15937500061451715, -4.541064518000417216, -2.621784821875001281 ) ) ;
#2747 = CARTESIAN_POINT ( 'NONE',  ( 2.121784821875001281, 13.70937500061451786, 33.67503911421598417 ) ) ;
#2748 = CARTESIAN_POINT ( 'NONE',  ( 4.790625000614518569, -3.027376345333610441, -5.243569643749999898 ) ) ;
#2749 = CARTESIAN_POINT ( 'NONE',  ( 29.72812500061451502, 4.541064518000418104, 2.621784821874999949 ) ) ;
#2750 = CARTESIAN_POINT ( 'NONE',  ( 29.50312500061451360, -4.541064518000417216, -2.621784821875001281 ) ) ;
#2751 = CARTESIAN_POINT ( 'NONE',  ( 1.138803498474273873E-14, 15.08749999999999858, 34.00000000000000000 ) ) ;
#2752 = DIRECTION ( 'NONE',  ( -1.000000000000000000, -0.000000000000000000, -0.000000000000000000 ) ) ;
#2753 = CARTESIAN_POINT ( 'NONE',  ( 29.55000000122903003, 5.773502691896255534, 3.535250795749688894E-16 ) ) ;
#2754 = CARTESIAN_POINT ( 'NONE',  ( 7.734375000614517326, 4.541064518000418104, 2.621784821874999949 ) ) ;
#2755 = CARTESIAN_POINT ( 'NONE',  ( 17.66250000122903430, -4.330127018922190985, -2.500000000000001332 ) ) ;
#2756 = CARTESIAN_POINT ( 'NONE',  ( 4.284375000614518925, -4.541064518000419881, 2.621784821874995952 ) ) ;
#2757 = CARTESIAN_POINT ( 'NONE',  ( 4.340625000614515727, -3.027376345333610441, -5.243569643749999898 ) ) ;
#2758 = CARTESIAN_POINT ( 'NONE',  ( -4.000000000000000888, 14.50624999877096677, 32.30940107675850470 ) ) ;
#2759 = CARTESIAN_POINT ( 'NONE',  ( 20.49375000122903501, 5.773502691896255534, 3.535250795749688894E-16 ) ) ;
#2760 = CARTESIAN_POINT ( 'NONE',  ( 15.19687500061451857, -3.027376345333610441, -5.243569643749999898 ) ) ;
#2761 = CARTESIAN_POINT ( 'NONE',  ( 20.99999999999999645, 0.000000000000000000, 4.999999999999998224 ) ) ;
#2762 = EDGE_LOOP ( 'NONE', ( #12032, #12705, #25248, #7136 ) ) ;
#2763 = CARTESIAN_POINT ( 'NONE',  ( 22.41562500061451502, 3.027376345333613106, -5.243569643749998122 ) ) ;
#2764 = CARTESIAN_POINT ( 'NONE',  ( 6.140625000614516438, -3.027376345333610441, -5.243569643749999898 ) ) ;
#2765 = CARTESIAN_POINT ( 'NONE',  ( 25.73437500061451644, 4.541064518000418104, 2.621784821874999949 ) ) ;
#2766 = CARTESIAN_POINT ( 'NONE',  ( 7.490625000614516082, -3.027376345333610441, -5.243569643749999898 ) ) ;
#2767 = CARTESIAN_POINT ( 'NONE',  ( 7.856250001229033053, 4.330127018922192761, -2.499999999999997780 ) ) ;
#2768 = CARTESIAN_POINT ( 'NONE',  ( 9.862500001229033586, 0.000000000000000000, 4.999999999999998224 ) ) ;
#2769 = CARTESIAN_POINT ( 'NONE',  ( 24.55312500061451786, -4.541064518000417216, -2.621784821875001281 ) ) ;
#2770 = CARTESIAN_POINT ( 'NONE',  ( 3.999999999999999112, 19.43750000122903288, -30.00000000000000000 ) ) ;
#2771 = CARTESIAN_POINT ( 'NONE',  ( 10.08750000122903323, 6.123233995736764310E-16, -4.999999999999998224 ) ) ;
#2772 = CARTESIAN_POINT ( 'NONE',  ( 19.41562500061451146, 3.027376345333611329, 5.243569643749999010 ) ) ;
#2773 = CARTESIAN_POINT ( 'NONE',  ( 16.94062500061451715, -3.027376345333610441, -5.243569643749999898 ) ) ;
#2774 = CARTESIAN_POINT ( 'NONE',  ( 27.75937500061451502, -4.119189519843965641, -2.378215178125001383 ) ) ;
#2775 = CARTESIAN_POINT ( 'NONE',  ( 18.89999999999999858, -4.330127018922190985, -2.500000000000001332 ) ) ;
#2776 = CARTESIAN_POINT ( 'NONE',  ( 14.58750000122903323, 6.123233995736764310E-16, -4.999999999999998224 ) ) ;
#2777 = CARTESIAN_POINT ( 'NONE',  ( 10.15312500061451750, -4.541064518000417216, -2.621784821875001281 ) ) ;
#2778 = CARTESIAN_POINT ( 'NONE',  ( 14.31562500061451537, 3.027376345333613106, -5.243569643749998122 ) ) ;
#2779 = CARTESIAN_POINT ( 'NONE',  ( 22.68750000122903288, 6.123233995736764310E-16, -4.999999999999998224 ) ) ;
#2780 = CARTESIAN_POINT ( 'NONE',  ( 21.90937500061451715, -4.541064518000417216, -2.621784821875001281 ) ) ;
#2781 = CARTESIAN_POINT ( 'NONE',  ( 20.55937500061451573, -4.541064518000417216, -2.621784821875001281 ) ) ;
#2782 = CARTESIAN_POINT ( 'NONE',  ( 24.82499999999999929, 6.123233995736764310E-16, -4.999999999999998224 ) ) ;
#2783 = EDGE_CURVE ( 'NONE', #4916, #19922, #26439, .T. ) ;
#2784 = CARTESIAN_POINT ( 'NONE',  ( 8.700000001229032165, -2.886751345948125991, -5.000000000000000000 ) ) ;
#2785 = CARTESIAN_POINT ( 'NONE',  ( 5.559375000614517504, 0.000000000000000000, 5.243569643749999010 ) ) ;
#2786 = CARTESIAN_POINT ( 'NONE',  ( 24.12187500061451217, -6.054752690667223547, -1.112240025338166033E-15 ) ) ;
#2787 = EDGE_CURVE ( 'NONE', #53615, #51815, #29242, .T. ) ;
#2788 = CARTESIAN_POINT ( 'NONE',  ( 21.85312500061451502, -4.541064518000417216, -2.621784821875001281 ) ) ;
#2789 = CARTESIAN_POINT ( 'NONE',  ( 24.49687500061451573, -3.027376345333614438, 5.243569643749998122 ) ) ;
#2790 = CARTESIAN_POINT ( 'NONE',  ( -3.756430356250000990, 19.31562499938548427, 32.16877607737301048 ) ) ;
#2791 = DIRECTION ( 'NONE',  ( 0.000000000000000000, 0.000000000000000000, 1.000000000000000000 ) ) ;
#2792 = CARTESIAN_POINT ( 'NONE',  ( 5.859375000614519102, 4.541064518000418104, -2.621784821874998173 ) ) ;
#2793 = CARTESIAN_POINT ( 'NONE',  ( 17.99062500061451786, 6.054752690667223547, 3.707466751127219781E-16 ) ) ;
#2794 = ORIENTED_EDGE ( 'NONE', *, *, #42990, .T. ) ;
#2795 = CYLINDRICAL_SURFACE ( 'NONE', #7670, 4.999999999999998224 ) ;
#2796 = CARTESIAN_POINT ( 'NONE',  ( 24.89062500061451644, -3.027376345333614438, 5.243569643749998122 ) ) ;
#2797 = CARTESIAN_POINT ( 'NONE',  ( 4.471875000614518925, 3.027376345333613106, -5.243569643749998122 ) ) ;
#2798 = CARTESIAN_POINT ( 'NONE',  ( 4.779258346327469376, 1.469247991000700582, 4.779258346327429408 ) ) ;
#2799 = CARTESIAN_POINT ( 'NONE',  ( 1.841668243974592611, 4.655663185590168673, -33.56086590413347892 ) ) ;
#2800 = CARTESIAN_POINT ( 'NONE',  ( 13.72500000000000142, 4.330127018922191873, 2.499999999999999556 ) ) ;
#2801 = CARTESIAN_POINT ( 'NONE',  ( 25.57500000122903216, 2.886751345948126879, 4.999999999999999112 ) ) ;
#2802 = CARTESIAN_POINT ( 'NONE',  ( 21.96562500061451573, 3.027376345333613106, -5.243569643749998122 ) ) ;
#2803 = ORIENTED_EDGE ( 'NONE', *, *, #45125, .F. ) ;
#2804 = CARTESIAN_POINT ( 'NONE',  ( 24.07499999999999929, 4.330127018922191873, 2.499999999999999556 ) ) ;
#2805 = CARTESIAN_POINT ( 'NONE',  ( 27.27187500061451431, -6.054752690667223547, -1.112240025338166033E-15 ) ) ;
#2806 = ORIENTED_EDGE ( 'NONE', *, *, #19846, .T. ) ;
#2807 = CARTESIAN_POINT ( 'NONE',  ( 13.35000000122903430, 5.773502691896255534, 3.535250795749688401E-16 ) ) ;
#2808 = CARTESIAN_POINT ( 'NONE',  ( 11.95312500061451644, -4.541064518000417216, -2.621784821875001281 ) ) ;
#2809 = CARTESIAN_POINT ( 'NONE',  ( 24.93750000122903288, 6.123233995736764310E-16, -4.999999999999998224 ) ) ;
#2810 = CARTESIAN_POINT ( 'NONE',  ( 16.84687500061451715, -4.119189519843965641, -2.378215178125001383 ) ) ;
#2811 = CARTESIAN_POINT ( 'NONE',  ( 29.39062500061451289, -3.027376345333614438, 5.243569643749998122 ) ) ;
#2812 = CARTESIAN_POINT ( 'NONE',  ( 12.37500000122903465, 2.886751345948129099, -4.999999999999998224 ) ) ;
#2813 = CARTESIAN_POINT ( 'NONE',  ( 20.21250000000000213, -5.773502691896255534, -1.060575238724906372E-15 ) ) ;
#2814 = CARTESIAN_POINT ( 'NONE',  ( 25.98750000000000071, -2.886751345948129988, 4.999999999999997335 ) ) ;
#2815 = CARTESIAN_POINT ( 'NONE',  ( 3.242103837493086330E-14, 12.80000000122903359, 26.00000000000000711 ) ) ;
#2816 = CARTESIAN_POINT ( 'NONE',  ( 7.171875000614517326, 3.027376345333613106, -5.243569643749998122 ) ) ;
#2817 = CARTESIAN_POINT ( 'NONE',  ( 19.95937500061451786, 0.000000000000000000, 5.243569643749999010 ) ) ;
#2818 = CARTESIAN_POINT ( 'NONE',  ( 19.80000000122903359, -2.886751345948130876, 4.999999999999996447 ) ) ;
#2819 = ORIENTED_EDGE ( 'NONE', *, *, #57401, .F. ) ;
#2820 = CARTESIAN_POINT ( 'NONE',  ( 27.70312500061451289, -4.541064518000417216, -2.621784821875001281 ) ) ;
#2821 = CARTESIAN_POINT ( 'NONE',  ( 4.200000000000001954, 4.330127018922192761, -2.499999999999997780 ) ) ;
#2822 = CARTESIAN_POINT ( 'NONE',  ( 5.446875000614518569, 6.054752690667223547, 3.707466751127219781E-16 ) ) ;
#2823 = CARTESIAN_POINT ( 'NONE',  ( 15.56250000000000000, 2.886751345948126879, 4.999999999999999112 ) ) ;
#2824 = CARTESIAN_POINT ( 'NONE',  ( 14.20312500061451644, -4.541064518000417216, -2.621784821875001281 ) ) ;
#2825 = CARTESIAN_POINT ( 'NONE',  ( 5.810221930991193690E-16, 19.36250000000000071, 26.00000000000000000 ) ) ;
#2826 = CARTESIAN_POINT ( 'NONE',  ( 1.592000809091587073E-14, 15.38750000000000284, -34.00000000000000000 ) ) ;
#2827 = CARTESIAN_POINT ( 'NONE',  ( 3.962290188940274405, -3.840926163143314920, 3.347320737315190531 ) ) ;
#2828 = CARTESIAN_POINT ( 'NONE',  ( 17.47500000122903430, 2.886751345948126879, 4.999999999999999112 ) ) ;
#2829 = CARTESIAN_POINT ( 'NONE',  ( 3.778125000614519280, -4.541064518000419881, 2.621784821874995952 ) ) ;
#2830 = CARTESIAN_POINT ( 'NONE',  ( 18.68437500061451928, -4.119189519843968306, 2.378215178124996054 ) ) ;
#2831 = CARTESIAN_POINT ( 'NONE',  ( 8.428125000614517859, 6.421520780324663323E-16, -5.243569643749999010 ) ) ;
#2832 = CARTESIAN_POINT ( 'NONE',  ( 24.19687500061451857, -3.027376345333610441, -5.243569643749999898 ) ) ;
#2833 = CARTESIAN_POINT ( 'NONE',  ( -3.000416591977282496E-16, 17.94687500061451502, 25.09994784771203058 ) ) ;
#2834 = CARTESIAN_POINT ( 'NONE',  ( 24.45937500061451786, 0.000000000000000000, 5.243569643749999010 ) ) ;
#2835 = CARTESIAN_POINT ( 'NONE',  ( 6.000000000000001776, 4.330127018922192761, -2.499999999999997780 ) ) ;
#2836 = CARTESIAN_POINT ( 'NONE',  ( -2.000000000000000000, 11.93750000122903465, 26.53589838486224650 ) ) ;
#2837 = CARTESIAN_POINT ( 'NONE',  ( 12.44062500061451537, -3.027376345333610441, -5.243569643749999898 ) ) ;
#2838 = CARTESIAN_POINT ( 'NONE',  ( 3.712500001229034563, -4.330127018922190985, -2.500000000000001332 ) ) ;
#2839 = CARTESIAN_POINT ( 'NONE',  ( 8.971875000614515372, 3.027376345333613106, -5.243569643749998122 ) ) ;
#2840 = CARTESIAN_POINT ( 'NONE',  ( 4.907911205059083602E-16, 5.000000000000000000, -26.00000000000000000 ) ) ;
#2841 = ORIENTED_EDGE ( 'NONE', *, *, #8791, .T. ) ;
#2842 = CARTESIAN_POINT ( 'NONE',  ( 11.80312500061451608, 0.000000000000000000, 5.243569643749999010 ) ) ;
#2843 = CARTESIAN_POINT ( 'NONE',  ( 45.00000000000000000, 6.123233995736764310E-16, -4.999999999999998224 ) ) ;
#2844 = CARTESIAN_POINT ( 'NONE',  ( 25.01250000122903216, 4.330127018922192761, -2.499999999999997780 ) ) ;
#2845 = CARTESIAN_POINT ( 'NONE',  ( 10.05937500061451750, 0.000000000000000000, 5.243569643749999010 ) ) ;
#2846 = CARTESIAN_POINT ( 'NONE',  ( 12.66562500061451502, 3.027376345333611329, 5.243569643749999010 ) ) ;
#2847 = CARTESIAN_POINT ( 'NONE',  ( 27.09375000122903288, -2.886751345948125991, -5.000000000000000000 ) ) ;
#2848 = CARTESIAN_POINT ( 'NONE',  ( 21.98437500061451644, 6.421520780324663323E-16, -5.243569643749999010 ) ) ;
#2849 = CARTESIAN_POINT ( 'NONE',  ( 0.000000000000000000, 20.00000000000000000, 30.00000000000000000 ) ) ;
#2850 = CARTESIAN_POINT ( 'NONE',  ( 4.276577733362700862, 2.590537181842085257, -4.276577733362700862 ) ) ;
#2851 = CARTESIAN_POINT ( 'NONE',  ( 30.00000000000000000, 0.000000000000000000, 4.999999999999998224 ) ) ;
#2852 = CARTESIAN_POINT ( 'NONE',  ( 9.001249775931846008E-16, 15.47187500061451892, -25.09994784771203058 ) ) ;
#2853 =( BOUNDED_CURVE ( )  B_SPLINE_CURVE ( 2, ( #29001, #50087, #45271, #72618, #72980, #56355, #213, #67089, #22362, #16448, #22718, #5745, #6103, #576, #22001, #44558, #67804, #27920, #61520, #23081, #5021, #17178, #38639, #55989, #61163, #28279, #44914, #23446, #5382, #34529, #27555, #39737, #34166, #45639, #50454, #62254, #55625, #11651, #28634, #51172, #67451, #40096, #45992, #68171, #61886, #16813, #68529, #39369, #51538, #11291, #33812, #50811, #17534, #62610, #12006, #57059, #6466, #939, #10558, #33086, #58140, #47804, #2738, #34896, #7546, #18617, #17890, #35259, #57425, #46720, #30807, #6829, #40450, #62966, #12723, #19340, #29718, #13814, #1294, #41895, #57781, #23804, #24893, #29364, #52256, #58503, #7190, #35984, #69970, #12362, #7913, #41536, #24535, #64422, #18975, #47438, #51896, #68889, #69255, #2024, #18246, #46355, #13434, #69614, #40819, #63335, #1659, #24168, #47079, #25256, #41182, #30080, #63691, #64054, #30450, #36354, #13082, #35620, #52979, #2375, #52618, #58867, #8277, #53340, #4212, #3104, #26741, #70333, #32639, #71437, #55180, #10109, #59969, #65522, #14176, #26000, #4575, #59232, #19710, #42262, #65150, #65891, #32273, #31910, #64785, #60696, #66253, #53712, #49274, #36710, #31544, #37810, #14540, #15271, #71807, #8640, #60330, #20812, #3845, #21177, #43367, #42991, #27105, #42626, #9739, #43729, #15631, #31169, #54806, #48905, #25633, #48171, #37076, #70695, #26366, #20070, #59600, #9377, #9013, #38172, #54084, #3482, #48539, #71066, #14908, #20441, #37450, #54446, #6376, #34081, #66625, #11919, #39650, #10830, #28551, #50727, #51086, #39283, #44830, #45185, #27470, #68082, #4936, #67717, #33001, #62169, #33366, #50371, #22635, #55540, #34444, #11200, #56273, #49638, #50002, #72164, #67365, #55902, #56972, #72527, #45552, #38918, #482, #61796, #72896, #11566, #5294, #17089, #21544, #21915, #56621, #44471, #22991, #44099, #6016, #22278, #16363, #16002, #67001, #62522, #38551, #61437, #61074, #17450, #10472, #27840, #40008, #16728, #33727, #5662, #28198, #130, #58781, #13725, #45906, #69169, #29631, #28908, #46264, #51446, #68804, #1209, #12995, #69527, #34806, #35531, #58414, #12638, #24442 ),
 .UNSPECIFIED., .F., .F. ) 
 B_SPLINE_CURVE_WITH_KNOTS ( ( 3, 2, 2, 2, 2, 2, 2, 2, 2, 2, 2, 2, 2, 2, 2, 2, 2, 2, 2, 2, 2, 2, 2, 2, 2, 2, 2, 2, 2, 2, 2, 2, 2, 2, 2, 2, 2, 2, 2, 2, 2, 2, 2, 2, 2, 2, 2, 2, 2, 2, 2, 2, 2, 2, 2, 2, 2, 2, 2, 2, 2, 2, 2, 2, 2, 2, 2, 2, 2, 2, 2, 2, 2, 2, 2, 2, 2, 2, 2, 2, 2, 2, 2, 2, 2, 2, 2, 2, 2, 2, 2, 2, 2, 2, 2, 2, 2, 2, 2, 2, 2, 2, 2, 2, 2, 2, 2, 2, 2, 2, 2, 2, 2, 2, 2, 2, 2, 2, 2, 2, 2, 2, 2, 2, 2, 2, 2, 2, 2, 2, 2, 2, 2, 2, 3 ),
 ( 0.000000000000000000, 0.007499808158871945282, 0.01499961631774389056, 0.02249942447661583411, 0.02999923263548778113, 0.03749904079435972815, 0.04499884895323166822, 0.05249865711210361524, 0.05999846527097556226, 0.06749827342984750234, 0.07499808158871945629, 0.08249788974759138249, 0.08999769790646333645, 0.09749750606533529040, 0.1049973142242072305, 0.1124971223830791706, 0.1199969305419511245, 0.1274967387008230646, 0.1349965468596950047, 0.1424963550185669448, 0.1499961631774389126, 0.1574959713363108527, 0.1649957794951827650, 0.1724955876540547328, 0.1799953958129266729, 0.1874952039717986130, 0.1949950121306705808, 0.2024948202895425209, 0.2099946284484144610, 0.2174944366072864010, 0.2249942447661583411, 0.2324940529250302812, 0.2399938610839022490, 0.2474936692427741891, 0.2549934774016461292, 0.2624932855605180970, 0.2699930937193900093, 0.2774929018782619772, 0.2849927100371338895, 0.2924925181960058573, 0.2999923263548778252, 0.3074921345137497375, 0.3149919426726217053, 0.3224917508314936176, 0.3299915589903655300, 0.3374913671492375533, 0.3449911753081094656, 0.3524909834669814335, 0.3599907916258533458, 0.3674905997847253136, 0.3749904079435972259, 0.3824902161024691938, 0.3899900242613411616, 0.3974898324202130739, 0.4049896405790850418, 0.4124894487379569541, 0.4199892568968289219, 0.4274890650557008898, 0.4349888732145728021, 0.4424886813734447699, 0.4499884895323166822, 0.4574882976911886501, 0.4649881058500605624, 0.4724879140089325302, 0.4799877221678044981, 0.4874875303266764104, 0.4949873384855483782, 0.5024871466444202905, 0.5099869548032922584, 0.5174867629621642262, 0.5249865711210361940, 0.5324863792799080509, 0.5399861874387800187, 0.5474859955976519865, 0.5549858037565239544, 0.5624856119153958112, 0.5699854200742677790, 0.5774852282331397468, 0.5849850363920117147, 0.5924848445508836825, 0.5999846527097556503, 0.6074844608686276182, 0.6149842690274994750, 0.6224840771863714428, 0.6299838853452434106, 0.6374836935041152675, 0.6449835016629872353, 0.6524833098218592031, 0.6599831179807310599, 0.6674829261396030278, 0.6749827342984751066, 0.6824825424573470745, 0.6899823506162189313, 0.6974821587750908991, 0.7049819669339628669, 0.7124817750928347238, 0.7199815832517066916, 0.7274813914105786594, 0.7349811995694506273, 0.7424810077283224841, 0.7499808158871944519, 0.7574806240460665308, 0.7649804322049383876, 0.7724802403638103554, 0.7799800485226823232, 0.7874798566815542911, 0.7949796648404261479, 0.8024794729992981157, 0.8099792811581700835, 0.8174790893170419404, 0.8249788974759139082, 0.8324787056347858760, 0.8399785137936578439, 0.8474783219525298117, 0.8549781301114017795, 0.8624779382702737474, 0.8699777464291456042, 0.8774775545880175720, 0.8849773627468895398, 0.8924771709057615077, 0.8999769790646333645, 0.9074767872235053323, 0.9149765953823773001, 0.9224764035412491570, 0.9299762117001211248, 0.9374760198589932036, 0.9449758280178650605, 0.9524756361767370283, 0.9599754443356089961, 0.9674752524944809640, 0.9749750606533528208, 0.9824748688122247886, 0.9899746769710967564, 0.9974744851299686133, 1.000000000000000000 ),
 .UNSPECIFIED. ) 
 CURVE ( )  GEOMETRIC_REPRESENTATION_ITEM ( )  RATIONAL_B_SPLINE_CURVE ( ( 1.000000000000000000, 0.8660254037844387076, 1.000000000000000000, 0.8660254037844387076, 1.000000000000000000, 0.8660254037844387076, 1.000000000000000000, 0.8660254037844387076, 1.000000000000000000, 0.8660254037844387076, 1.000000000000000000, 0.8660254037844387076, 1.000000000000000000, 0.8660254037844387076, 1.000000000000000000, 0.8660254037844387076, 1.000000000000000000, 0.8660254037844387076, 1.000000000000000000, 0.8660254037844387076, 1.000000000000000000, 0.8660254037844387076, 1.000000000000000000, 0.8660254037844387076, 1.000000000000000000, 0.8660254037844387076, 1.000000000000000000, 0.8660254037844387076, 1.000000000000000000, 0.8660254037844387076, 1.000000000000000000, 0.8660254037844387076, 1.000000000000000000, 0.8660254037844387076, 1.000000000000000000, 0.8660254037844387076, 1.000000000000000000, 0.8660254037844387076, 1.000000000000000000, 0.8660254037844387076, 1.000000000000000000, 0.8660254037844387076, 1.000000000000000000, 0.8660254037844387076, 1.000000000000000000, 0.8660254037844387076, 1.000000000000000000, 0.8660254037844387076, 1.000000000000000000, 0.8660254037844387076, 1.000000000000000000, 0.8660254037844387076, 1.000000000000000000, 0.8660254037844387076, 1.000000000000000000, 0.8660254037844387076, 1.000000000000000000, 0.8660254037844387076, 1.000000000000000000, 0.8660254037844387076, 1.000000000000000000, 0.8660254037844387076, 1.000000000000000000, 0.8660254037844387076, 1.000000000000000000, 0.8660254037844387076, 1.000000000000000000, 0.8660254037844387076, 1.000000000000000000, 0.8660254037844387076, 1.000000000000000000, 0.8660254037844387076, 1.000000000000000000, 0.8660254037844387076, 1.000000000000000000, 0.8660254037844387076, 1.000000000000000000, 0.8660254037844387076, 1.000000000000000000, 0.8660254037844387076, 1.000000000000000000, 0.8660254037844387076, 1.000000000000000000, 0.8660254037844387076, 1.000000000000000000, 0.8660254037844387076, 1.000000000000000000, 0.8660254037844387076, 1.000000000000000000, 0.8660254037844387076, 1.000000000000000000, 0.8660254037844387076, 1.000000000000000000, 0.8660254037844387076, 1.000000000000000000, 0.8660254037844387076, 1.000000000000000000, 0.8660254037844387076, 1.000000000000000000, 0.8660254037844387076, 1.000000000000000000, 0.8660254037844387076, 1.000000000000000000, 0.8660254037844387076, 1.000000000000000000, 0.8660254037844387076, 1.000000000000000000, 0.8660254037844387076, 1.000000000000000000, 0.8660254037844387076, 1.000000000000000000, 0.8660254037844387076, 1.000000000000000000, 0.8660254037844387076, 1.000000000000000000, 0.8660254037844387076, 1.000000000000000000, 0.8660254037844387076, 1.000000000000000000, 0.8660254037844387076, 1.000000000000000000, 0.8660254037844387076, 1.000000000000000000, 0.8660254037844387076, 1.000000000000000000, 0.8660254037844387076, 1.000000000000000000, 0.8660254037844387076, 1.000000000000000000, 0.8660254037844387076, 1.000000000000000000, 0.8660254037844387076, 1.000000000000000000, 0.8660254037844387076, 1.000000000000000000, 0.8660254037844387076, 1.000000000000000000, 0.8660254037844387076, 1.000000000000000000, 0.8660254037844387076, 1.000000000000000000, 0.8660254037844387076, 1.000000000000000000, 0.8660254037844387076, 1.000000000000000000, 0.8660254037844387076, 1.000000000000000000, 0.8660254037844387076, 1.000000000000000000, 0.8660254037844387076, 1.000000000000000000, 0.8660254037844387076, 1.000000000000000000, 0.8660254037844387076, 1.000000000000000000, 0.8660254037844387076, 1.000000000000000000, 0.8660254037844387076, 1.000000000000000000, 0.8660254037844387076, 1.000000000000000000, 0.8660254037844387076, 1.000000000000000000, 0.8660254037844387076, 1.000000000000000000, 0.8660254037844387076, 1.000000000000000000, 0.8660254037844387076, 1.000000000000000000, 0.8660254037844387076, 1.000000000000000000, 0.8660254037844387076, 1.000000000000000000, 0.8660254037844387076, 1.000000000000000000, 0.8660254037844387076, 1.000000000000000000, 0.8660254037844387076, 1.000000000000000000, 0.8660254037844387076, 1.000000000000000000, 0.8660254037844387076, 1.000000000000000000, 0.8660254037844387076, 1.000000000000000000, 0.8660254037844387076, 1.000000000000000000, 0.8660254037844387076, 1.000000000000000000, 0.8660254037844387076, 1.000000000000000000, 0.8660254037844387076, 1.000000000000000000, 0.8660254037844387076, 1.000000000000000000, 0.8660254037844387076, 1.000000000000000000, 0.8660254037844387076, 1.000000000000000000, 0.8660254037844387076, 1.000000000000000000, 0.8660254037844387076, 1.000000000000000000, 0.8660254037844387076, 1.000000000000000000, 0.8660254037844387076, 1.000000000000000000, 0.8660254037844387076, 1.000000000000000000, 0.8660254037844387076, 1.000000000000000000, 0.8660254037844387076, 1.000000000000000000, 0.8660254037844387076, 1.000000000000000000, 0.8660254037844387076, 1.000000000000000000, 0.8660254037844387076, 1.000000000000000000, 0.8660254037844387076, 1.000000000000000000, 0.8660254037844387076, 1.000000000000000000, 0.8660254037844387076, 1.000000000000000000, 0.8660254037844387076, 1.000000000000000000, 0.8660254037844387076, 1.000000000000000000, 0.8660254037844387076, 1.000000000000000000, 0.8660254037844387076, 1.000000000000000000, 0.8660254037844387076, 1.000000000000000000, 0.8660254037844387076, 1.000000000000000000, 0.8660254037844387076, 1.000000000000000000, 0.8660254037844387076, 1.000000000000000000, 0.8660254037844387076, 1.000000000000000000, 0.8660254037844387076, 1.000000000000000000, 0.8660254037844387076, 1.000000000000000000, 0.8660254037844387076, 1.000000000000000000, 0.8660254037844387076, 1.000000000000000000, 0.8660254037844387076, 1.000000000000000000, 0.8660254037844387076, 1.000000000000000000, 0.8660254037844387076, 1.000000000000000000, 0.8660254037844387076, 1.000000000000000000, 0.8660254037844387076, 1.000000000000000000, 0.8660254037844387076, 1.000000000000000000, 0.8660254037844387076, 1.000000000000000000, 0.8660254037844387076, 1.000000000000000000, 0.9548848677736607726, 0.9401542295229587953 ) ) 
 REPRESENTATION_ITEM ( '' )  );
#2854 = CARTESIAN_POINT ( 'NONE',  ( 15.60937500061451644, -4.541064518000417216, -2.621784821875001281 ) ) ;
#2855 = CARTESIAN_POINT ( 'NONE',  ( 18.07500000122903216, -5.773502691896255534, -1.060575238724906372E-15 ) ) ;
#2856 = CARTESIAN_POINT ( 'NONE',  ( 12.87187500061451750, -6.054752690667223547, -1.112240025338166033E-15 ) ) ;
#2857 = CARTESIAN_POINT ( 'NONE',  ( -2.121784821874996840, 18.07812500061451644, -26.32496088578401583 ) ) ;
#2858 = CARTESIAN_POINT ( 'NONE',  ( 18.22500000122903430, 2.886751345948129099, -4.999999999999998224 ) ) ;
#2859 = CARTESIAN_POINT ( 'NONE',  ( 13.00312500061451537, 4.541064518000418104, -2.621784821874998173 ) ) ;
#2860 = VECTOR ( 'NONE', #1404, 1000.000000000000000 ) ;
#2861 = VERTEX_POINT ( 'NONE', #40437 ) ;
#2862 = CARTESIAN_POINT ( 'NONE',  ( 15.75000000000000000, -4.330127018922190985, -2.500000000000001332 ) ) ;
#2863 = CARTESIAN_POINT ( 'NONE',  ( 19.16250000122903430, 4.330127018922192761, -2.499999999999997780 ) ) ;
#2864 = CARTESIAN_POINT ( 'NONE',  ( 12.90937500061451537, -4.541064518000417216, -2.621784821875001281 ) ) ;
#2865 = CARTESIAN_POINT ( 'NONE',  ( 3.027206758929961161, 3.985217399322935172, 27.37339809994529105 ) ) ;
#2866 = CARTESIAN_POINT ( 'NONE',  ( 11.81250000122903465, -4.330127018922190985, -2.500000000000001332 ) ) ;
#2867 = CARTESIAN_POINT ( 'NONE',  ( 20.73750000122903359, -4.330127018922194537, 2.499999999999995559 ) ) ;
#2868 = CARTESIAN_POINT ( 'NONE',  ( 18.25312500061451715, -4.541064518000417216, -2.621784821875001281 ) ) ;
#2869 = CARTESIAN_POINT ( 'NONE',  ( 20.54062500061451502, -3.027376345333610441, -5.243569643749999898 ) ) ;
#2870 = CARTESIAN_POINT ( 'NONE',  ( 27.67500000122903359, 2.886751345948129099, -4.999999999999998224 ) ) ;
#2871 = CARTESIAN_POINT ( 'NONE',  ( 25.12499999999999645, -4.330127018922194537, 2.499999999999995559 ) ) ;
#2872 = CARTESIAN_POINT ( 'NONE',  ( 45.00000000000000000, 2.500000000000000000, -3.500000000000000000 ) ) ;
#2873 = CARTESIAN_POINT ( 'NONE',  ( 28.94999999999999929, 4.330127018922192761, -2.499999999999997780 ) ) ;
#2874 = CARTESIAN_POINT ( 'NONE',  ( 27.12187500061451573, 3.027376345333611329, 5.243569643749999010 ) ) ;
#2875 = CARTESIAN_POINT ( 'NONE',  ( -1.389182545231912203, 9.676047173952133207, -33.81675723707382275 ) ) ;
#2876 = CARTESIAN_POINT ( 'NONE',  ( -4.243569643749997233, 14.49687500061451928, -27.54997392385601174 ) ) ;
#2877 = CARTESIAN_POINT ( 'NONE',  ( 4.350000001229033408, 5.773502691896255534, 3.535250795749688894E-16 ) ) ;
#2878 = CARTESIAN_POINT ( 'NONE',  ( 3.900000000000000799, 0.000000000000000000, 4.999999999999998224 ) ) ;
#2879 = EDGE_CURVE ( 'NONE', #12976, #35743, #16076, .T. ) ;
#2880 = CARTESIAN_POINT ( 'NONE',  ( 7.096875000614517148, -3.027376345333610441, -5.243569643749999898 ) ) ;
#2881 = CARTESIAN_POINT ( 'NONE',  ( 27.66562500061451146, -6.054752690667223547, -1.112240025338166033E-15 ) ) ;
#2882 = CARTESIAN_POINT ( 'NONE',  ( -1.878215178124999163, 13.35312499938548392, 26.74683588394047007 ) ) ;
#2883 = CARTESIAN_POINT ( 'NONE',  ( 7.285825834671762338E-16, 10.00000000000000000, -24.00000000000000000 ) ) ;
#2884 = CARTESIAN_POINT ( 'NONE',  ( 8.250000000000000000, 4.330127018922192761, -2.499999999999997780 ) ) ;
#2885 = CARTESIAN_POINT ( 'NONE',  ( 5.259375000614518569, -4.541064518000417216, -2.621784821875001281 ) ) ;
#2886 = CARTESIAN_POINT ( 'NONE',  ( 12.27187500061451786, 3.027376345333611329, 5.243569643749999010 ) ) ;
#2887 = CARTESIAN_POINT ( 'NONE',  ( 4.800000000000002487, 0.000000000000000000, 4.999999999999998224 ) ) ;
#2888 =( BOUNDED_CURVE ( )  B_SPLINE_CURVE ( 2, ( #41429, #24059, #40705, #58757, #57676, #7081, #827 ),
 .UNSPECIFIED., .F., .F. ) 
 B_SPLINE_CURVE_WITH_KNOTS ( ( 3, 2, 2, 3 ),
 ( 0.009999999999999979391, 0.01333333333333330643, 0.01666666666666663174, 0.01999999999999995878 ),
 .UNSPECIFIED. ) 
 CURVE ( )  GEOMETRIC_REPRESENTATION_ITEM ( )  RATIONAL_B_SPLINE_CURVE ( ( 1.000000000000000888, 0.8660254037844378194, 1.000000000000000000, 0.8660254037844387076, 1.000000000000000000, 0.8660254037844403729, 0.9999999999999983347 ) ) 
 REPRESENTATION_ITEM ( '' )  );
#2889 = CARTESIAN_POINT ( 'NONE',  ( -3.000416591977282496E-16, 14.29062500061459495, 25.09994784771203058 ) ) ;
#2890 = CARTESIAN_POINT ( 'NONE',  ( 6.150000000000003020, 0.000000000000000000, 4.999999999999998224 ) ) ;
#2891 = CARTESIAN_POINT ( 'NONE',  ( 16.39687500061451431, -4.119189519843965641, -2.378215178125001383 ) ) ;
#2892 = CARTESIAN_POINT ( 'NONE',  ( 21.06562500061451715, 3.027376345333613106, -5.243569643749998122 ) ) ;
#2893 = CARTESIAN_POINT ( 'NONE',  ( 9.965625000614517504, 3.027376345333611329, 5.243569643749999010 ) ) ;
#2894 = CARTESIAN_POINT ( 'NONE',  ( 24.27187500061451431, 4.119189519843966529, 2.378215178124999607 ) ) ;
#2895 = CARTESIAN_POINT ( 'NONE',  ( 8.521875000614516082, 3.027376345333613106, -5.243569643749998122 ) ) ;
#2896 = CARTESIAN_POINT ( 'NONE',  ( 26.81250000000000000, 2.886751345948126879, 4.999999999999999112 ) ) ;
#2897 = CARTESIAN_POINT ( 'NONE',  ( 19.23750000122903714, 4.330127018922191873, 2.499999999999999556 ) ) ;
#2899 = CARTESIAN_POINT ( 'NONE',  ( 26.65312500061451573, 0.000000000000000000, 5.243569643749999010 ) ) ;
#2898 = VECTOR ( 'NONE', #20773, 1000.000000000000000 ) ;
#2900 = CARTESIAN_POINT ( 'NONE',  ( 3.999999999999998668, 10.92500000122903536, 27.69059892324149530 ) ) ;
#2901 = CARTESIAN_POINT ( 'NONE',  ( 9.496875000614517504, 6.054752690667223547, 3.707466751127219781E-16 ) ) ;
#2902 = CARTESIAN_POINT ( 'NONE',  ( 15.30937500061451750, 4.541064518000418104, -2.621784821874998173 ) ) ;
#2903 = CARTESIAN_POINT ( 'NONE',  ( 26.89687500061451431, -3.027376345333610441, -5.243569643749999898 ) ) ;
#2904 = CARTESIAN_POINT ( 'NONE',  ( 28.19999999999999929, 0.000000000000000000, 4.999999999999998224 ) ) ;
#2905 = CARTESIAN_POINT ( 'NONE',  ( 12.00000000000000000, 0.000000000000000000, 4.999999999999998224 ) ) ;
#2906 = CARTESIAN_POINT ( 'NONE',  ( 19.77187500061451786, 3.027376345333613106, -5.243569643749998122 ) ) ;
#2907 = CARTESIAN_POINT ( 'NONE',  ( 12.90937500061451537, -4.541064518000417216, -2.621784821875001281 ) ) ;
#2908 = CARTESIAN_POINT ( 'NONE',  ( -7.967954043666661671E-16, 13.42812499938548321, 34.33755215474603517 ) ) ;
#2909 = CARTESIAN_POINT ( 'NONE',  ( 23.55000000000000071, 4.330127018922192761, -2.499999999999997780 ) ) ;
#2910 = CARTESIAN_POINT ( 'NONE',  ( -4.000000000000000000, 15.87500000000000000, 30.00000000000000000 ) ) ;
#2911 = CARTESIAN_POINT ( 'NONE',  ( -4.243569643749997233, 11.79687500061451999, -27.54997392385601174 ) ) ;
#2912 = CARTESIAN_POINT ( 'NONE',  ( 25.47187500061451715, -5.492252693125287522, -1.008910452111647106E-15 ) ) ;
#2913 = CARTESIAN_POINT ( 'NONE',  ( 14.46562500061451750, 3.027376345333611329, 5.243569643749999010 ) ) ;
#2914 = CARTESIAN_POINT ( 'NONE',  ( 4.087500000000001243, -2.886751345948125991, -5.000000000000000000 ) ) ;
#2915 = CYLINDRICAL_SURFACE ( 'NONE', #53610, 3.999999999999996447 ) ;
#2916 = DIRECTION ( 'NONE',  ( 1.000000000000000000, -0.000000000000000000, -0.000000000000000000 ) ) ;
#2917 = CARTESIAN_POINT ( 'NONE',  ( 12.00000000000000000, 0.000000000000000000, 4.999999999999998224 ) ) ;
#2918 = CARTESIAN_POINT ( 'NONE',  ( 3.999999999999998668, 17.67500000122903359, 27.69059892324149175 ) ) ;
#2920 =( BOUNDED_CURVE ( )  B_SPLINE_CURVE ( 1, ( #61889, #16451 ),
 .UNSPECIFIED., .F., .F. ) 
 B_SPLINE_CURVE_WITH_KNOTS ( ( 2, 2 ),
 ( 0.000000000000000000, 1.000000000000000000 ),
 .UNSPECIFIED. ) 
 CURVE ( )  GEOMETRIC_REPRESENTATION_ITEM ( )  RATIONAL_B_SPLINE_CURVE ( ( 0.9401540605060327849, 0.9401540605060327849 ) ) 
 REPRESENTATION_ITEM ( '' )  );
#2919 = CARTESIAN_POINT ( 'NONE',  ( 12.03750000122903430, 4.330127018922191873, 2.499999999999999556 ) ) ;
#2921 = CARTESIAN_POINT ( 'NONE',  ( 21.34687500061451715, -3.027376345333614438, 5.243569643749998122 ) ) ;
#2922 = CARTESIAN_POINT ( 'NONE',  ( 16.73437500061451644, 4.541064518000418104, 2.621784821874999949 ) ) ;
#2923 = CARTESIAN_POINT ( 'NONE',  ( 1.626862140677534273E-15, 16.51249999999999929, -26.00000000000000355 ) ) ;
#2924 = ORIENTED_EDGE ( 'NONE', *, *, #37057, .T. ) ;
#2925 = CARTESIAN_POINT ( 'NONE',  ( 19.49062500061451431, -3.027376345333614438, 5.243569643749998122 ) ) ;
#2926 = AXIS2_PLACEMENT_3D ( 'NONE', #23677, #1168, #63567 ) ;
#2927 = CARTESIAN_POINT ( 'NONE',  ( 4.415625000614518569, 3.027376345333613106, -5.243569643749998122 ) ) ;
#2928 = CARTESIAN_POINT ( 'NONE',  ( 17.10937500061451999, 4.541064518000418104, -2.621784821874998173 ) ) ;
#2929 = CARTESIAN_POINT ( 'NONE',  ( 28.09687500061451360, -3.027376345333614438, 5.243569643749998122 ) ) ;
#2930 = CARTESIAN_POINT ( 'NONE',  ( 3.928125000614516527, 6.421520780324663323E-16, -5.243569643749999010 ) ) ;
#2931 = CARTESIAN_POINT ( 'NONE',  ( 18.62812500061451715, -4.541064518000419881, 2.621784821874995952 ) ) ;
#2932 = CARTESIAN_POINT ( 'NONE',  ( 2.121784821875001281, 15.00312500061451715, 33.67503911421598417 ) ) ;
#2933 = CARTESIAN_POINT ( 'NONE',  ( 16.57500000122903216, 2.886751345948126879, 4.999999999999999112 ) ) ;
#2934 = CARTESIAN_POINT ( 'NONE',  ( 13.24687500061451750, -2.746126346562646425, 4.756430356249996549 ) ) ;
#2935 = CARTESIAN_POINT ( 'NONE',  ( 8.315625000614515372, -6.054752690667223547, -1.112240025338166033E-15 ) ) ;
#2936 = CARTESIAN_POINT ( 'NONE',  ( 29.57812500061451644, 6.421520780324663323E-16, -5.243569643749999010 ) ) ;
#2937 = CARTESIAN_POINT ( 'NONE',  ( 22.95937500061451431, 4.541064518000418104, -2.621784821874998173 ) ) ;
#2938 = CARTESIAN_POINT ( 'NONE',  ( 13.45312500061451466, 4.541064518000418104, -2.621784821874998173 ) ) ;
#2939 = CARTESIAN_POINT ( 'NONE',  ( 25.12500000122903288, 2.886751345948126879, 4.999999999999999112 ) ) ;
#2940 = CARTESIAN_POINT ( 'NONE',  ( 22.56562500061451715, 3.027376345333611329, 5.243569643749999010 ) ) ;
#2941 = CARTESIAN_POINT ( 'NONE',  ( 19.84687500061451360, 6.054752690667223547, 3.707466751127219781E-16 ) ) ;
#2942 = CARTESIAN_POINT ( 'NONE',  ( 14.87812500061451537, 4.541064518000418104, 2.621784821874999949 ) ) ;
#2943 = CARTESIAN_POINT ( 'NONE',  ( 4.243569643749999010, 15.17187500061451644, 27.54997392385601174 ) ) ;
#2944 =( BOUNDED_CURVE ( )  B_SPLINE_CURVE ( 2, ( #4358, #66399, #32416, #15411, #15051, #15776, #49781, #65291, #44243 ),
 .UNSPECIFIED., .F., .F. ) 
 B_SPLINE_CURVE_WITH_KNOTS ( ( 3, 2, 2, 2, 3 ),
 ( 0.6805555555555555802, 0.6851851851851852304, 0.6944444444444444198, 0.7037037037037037202, 0.7083333333333333703 ),
 .UNSPECIFIED. ) 
 CURVE ( )  GEOMETRIC_REPRESENTATION_ITEM ( )  RATIONAL_B_SPLINE_CURVE ( ( 0.9330127018922194093, 0.9330127018922194093, 1.000000000000000000, 0.8660254037844387076, 1.000000000000000000, 0.8660254037844387076, 1.000000000000000000, 0.9330127018922185211, 0.9330127018922192983 ) ) 
 REPRESENTATION_ITEM ( '' )  );
#2945 = CARTESIAN_POINT ( 'NONE',  ( 20.42812500061451431, -4.541064518000419881, 2.621784821874995952 ) ) ;
#2946 = CARTESIAN_POINT ( 'NONE',  ( 28.86562500061451786, 3.027376345333611329, 5.243569643749999010 ) ) ;
#2947 = ORIENTED_EDGE ( 'NONE', *, *, #20762, .F. ) ;
#2948 = ORIENTED_EDGE ( 'NONE', *, *, #66296, .T. ) ;
#2949 = CARTESIAN_POINT ( 'NONE',  ( 23.13749999999999929, 5.773502691896255534, 3.535250795749688894E-16 ) ) ;
#2950 = CARTESIAN_POINT ( 'NONE',  ( -3.999999999999999112, 10.55000000000000249, -30.00000000000000000 ) ) ;
#2951 = CARTESIAN_POINT ( 'NONE',  ( 13.16250000122903430, -4.330127018922190985, -2.500000000000001332 ) ) ;
#2952 = CARTESIAN_POINT ( 'NONE',  ( 28.04062500061451502, -3.027376345333614438, 5.243569643749998122 ) ) ;
#2953 = CARTESIAN_POINT ( 'NONE',  ( 8.503125000614515372, 4.541064518000418104, -2.621784821874998173 ) ) ;
#2954 = CARTESIAN_POINT ( 'NONE',  ( 19.57500000122903216, 2.886751345948129099, -4.999999999999998224 ) ) ;
#2955 = CARTESIAN_POINT ( 'NONE',  ( 24.29062500061451502, 6.054752690667223547, 3.707466751127219781E-16 ) ) ;
#2956 = CARTESIAN_POINT ( 'NONE',  ( 24.44999999999999929, 4.330127018922192761, -2.499999999999997780 ) ) ;
#2957 = CARTESIAN_POINT ( 'NONE',  ( 27.10312500061451502, 0.000000000000000000, 5.243569643749999010 ) ) ;
#2958 = CARTESIAN_POINT ( 'NONE',  ( 7.790625000614518569, -3.027376345333614438, 5.243569643749998122 ) ) ;
#2959 = ORIENTED_EDGE ( 'NONE', *, *, #70747, .F. ) ;
#2960 = CARTESIAN_POINT ( 'NONE',  ( 23.09062500061451573, -3.027376345333614438, 5.243569643749998122 ) ) ;
#2961 = CARTESIAN_POINT ( 'NONE',  ( 5.503125000614516260, 0.000000000000000000, 5.243569643749999010 ) ) ;
#2962 = CARTESIAN_POINT ( 'NONE',  ( 14.07187500061451679, 2.746126346562643317, 4.756430356249998326 ) ) ;
#2963 = CARTESIAN_POINT ( 'NONE',  ( 3.740625000614516527, -3.027376345333614438, 5.243569643749998122 ) ) ;
#2964 = EDGE_CURVE ( 'NONE', #47076, #64681, #6604, .T. ) ;
#2965 = CARTESIAN_POINT ( 'NONE',  ( -3.999999999999997335, 10.25000000122903643, 32.30940107675850470 ) ) ;
#2966 = VECTOR ( 'NONE', #39359, 1000.000000000000000 ) ;
#2967 = CARTESIAN_POINT ( 'NONE',  ( 13.68750000000000178, 5.773502691896255534, 3.535250795749688894E-16 ) ) ;
#2969 = CARTESIAN_POINT ( 'NONE',  ( 14.59687500061452070, -3.027376345333614438, 5.243569643749998122 ) ) ;
#2968 = AXIS2_PLACEMENT_3D ( 'NONE', #71232, #47603, #37613 ) ;
#2970 = CARTESIAN_POINT ( 'NONE',  ( 9.187500001229034652, 6.123233995736764310E-16, -4.999999999999998224 ) ) ;
#2971 = CARTESIAN_POINT ( 'NONE',  ( 15.53437500061451715, -4.541064518000419881, 2.621784821874995952 ) ) ;
#2972 = CARTESIAN_POINT ( 'NONE',  ( 14.96250000000000036, 2.886751345948129099, -4.999999999999998224 ) ) ;
#2973 = CARTESIAN_POINT ( 'NONE',  ( 9.496875000614517504, 6.054752690667223547, 3.707466751127219781E-16 ) ) ;
#2974 = CARTESIAN_POINT ( 'NONE',  ( 9.001249775931846008E-16, 11.81562500061451715, -25.09994784771203058 ) ) ;
#2975 = CARTESIAN_POINT ( 'NONE',  ( 24.71250000000000213, -5.773502691896255534, -1.060575238724906372E-15 ) ) ;
#2976 = CARTESIAN_POINT ( 'NONE',  ( 12.83437500061451786, -4.541064518000419881, 2.621784821874995952 ) ) ;
#2977 = CARTESIAN_POINT ( 'NONE',  ( 15.78749999999999432, -2.886751345948181946, -4.999999999999904077 ) ) ;
#2978 = CARTESIAN_POINT ( 'NONE',  ( 21.77812500061451928, -4.541064518000419881, 2.621784821874995952 ) ) ;
#2979 = CARTESIAN_POINT ( 'NONE',  ( -3.000416591977282496E-16, 10.29687500061451644, 25.09994784771203058 ) ) ;
#2980 = CARTESIAN_POINT ( 'NONE',  ( 26.33437500061451431, -4.541064518000419881, 2.621784821874995952 ) ) ;
#2981 = CARTESIAN_POINT ( 'NONE',  ( 29.10937500061451644, -4.541064518000417216, -2.621784821875001281 ) ) ;
#2982 = CARTESIAN_POINT ( 'NONE',  ( 3.328125000614516438, -4.541064518000419881, 2.621784821874995952 ) ) ;
#2983 = CARTESIAN_POINT ( 'NONE',  ( 23.10937500061451644, -5.492252693125287522, -1.008910452111647106E-15 ) ) ;
#2984 = CARTESIAN_POINT ( 'NONE',  ( 17.29687500061451999, -3.027376345333614438, 5.243569643749998122 ) ) ;
#2985 = CARTESIAN_POINT ( 'NONE',  ( 8.821875000614515017, 5.824947211148865298E-16, -4.756430356249998326 ) ) ;
#2986 = CARTESIAN_POINT ( 'NONE',  ( 3.815625000614518036, -6.054752690667223547, -1.112240025338166033E-15 ) ) ;
#2987 = CARTESIAN_POINT ( 'NONE',  ( 6.271875000614517859, 3.027376345333613106, -5.243569643749998122 ) ) ;
#2988 = CARTESIAN_POINT ( 'NONE',  ( 17.59687500061451715, 6.054752690667223547, 3.707466751127219781E-16 ) ) ;
#2989 = CARTESIAN_POINT ( 'NONE',  ( -3.594031514960484675, 25.10343495127339608, 28.22486214709212149 ) ) ;
#2990 = CARTESIAN_POINT ( 'NONE',  ( 24.78750000000000497, -2.886751345948125991, -5.000000000000000000 ) ) ;
#2991 = CARTESIAN_POINT ( 'NONE',  ( 27.90937500061451715, 4.541064518000418104, -2.621784821874998173 ) ) ;
#2992 = CARTESIAN_POINT ( 'NONE',  ( -3.756430356250000102, 13.87812499938548250, 30.00000000000000000 ) ) ;
#2993 = CARTESIAN_POINT ( 'NONE',  ( 30.00000000000000000, 0.000000000000000000, 4.999999999999998224 ) ) ;
#2994 = EDGE_LOOP ( 'NONE', ( #15905, #22606, #31537, #29961 ) ) ;
#2995 = CARTESIAN_POINT ( 'NONE',  ( 8.437500000000000000, -2.886751345948129988, 4.999999999999997335 ) ) ;
#2996 = CARTESIAN_POINT ( 'NONE',  ( 10.32187500061451679, 4.119189519843966529, 2.378215178124999607 ) ) ;
#2997 = CARTESIAN_POINT ( 'NONE',  ( 21.81562500061451004, -6.054752690667223547, -1.112240025338166033E-15 ) ) ;
#2998 = CARTESIAN_POINT ( 'NONE',  ( 11.81250000000000000, 2.886751345948129099, -4.999999999999998224 ) ) ;
#2999 = CARTESIAN_POINT ( 'NONE',  ( 6.290625000614517681, 6.054752690667223547, 3.707466751127219781E-16 ) ) ;
#3000 = CARTESIAN_POINT ( 'NONE',  ( 19.61249999999999716, 2.886751345948126879, 4.999999999999999112 ) ) ;
#3001 = CARTESIAN_POINT ( 'NONE',  ( 19.26562500061451644, 3.027376345333613106, -5.243569643749998122 ) ) ;
#3002 = LINE ( 'NONE', #42527, #72647 ) ;
#3003 = CARTESIAN_POINT ( 'NONE',  ( 23.70000000122903216, 5.773502691896255534, 3.535250795749688894E-16 ) ) ;
#3004 = CARTESIAN_POINT ( 'NONE',  ( -7.967954043666661671E-16, 18.82812499938548356, 34.33755215474603517 ) ) ;
#3005 = CARTESIAN_POINT ( 'NONE',  ( 4.462500000000001243, -5.773502691896255534, -1.060575238724906372E-15 ) ) ;
#3006 = ORIENTED_EDGE ( 'NONE', *, *, #11716, .F. ) ;
#3007 = CARTESIAN_POINT ( 'NONE',  ( 19.75312500061451360, 4.541064518000418104, -2.621784821874998173 ) ) ;
#3008 = CARTESIAN_POINT ( 'NONE',  ( 26.57812500061451644, 4.541064518000418104, 2.621784821874999949 ) ) ;
#3009 = CARTESIAN_POINT ( 'NONE',  ( 25.88437500061451502, -4.541064518000419881, 2.621784821874995952 ) ) ;
#3010 = CARTESIAN_POINT ( 'NONE',  ( 7.987500000000000711, -2.886751345948129988, 4.999999999999997335 ) ) ;
#3011 = CARTESIAN_POINT ( 'NONE',  ( 12.59062500061451573, 6.054752690667223547, 3.707466751127219781E-16 ) ) ;
#3012 = CARTESIAN_POINT ( 'NONE',  ( 29.12812500061451715, 6.421520780324663323E-16, -5.243569643749999010 ) ) ;
#3013 = CARTESIAN_POINT ( 'NONE',  ( 18.08437500061451431, 4.541064518000418104, 2.621784821874999949 ) ) ;
#3014 = CARTESIAN_POINT ( 'NONE',  ( 9.140625000614518214, -3.027376345333614438, 5.243569643749998122 ) ) ;
#3015 = CARTESIAN_POINT ( 'NONE',  ( 22.80000000000000071, 0.000000000000000000, 4.999999999999998224 ) ) ;
#3016 = CARTESIAN_POINT ( 'NONE',  ( 4.243569643749999898, 12.84687500061451715, 32.45002607614398471 ) ) ;
#3017 = CARTESIAN_POINT ( 'NONE',  ( 23.43750000122902932, -4.330127018922194537, 2.499999999999995559 ) ) ;
#3018 = CARTESIAN_POINT ( 'NONE',  ( 20.70937500061451786, 4.119189519843966529, -2.378215178124998275 ) ) ;
#3019 = CARTESIAN_POINT ( 'NONE',  ( 13.30312500061451786, -4.541064518000417216, -2.621784821875001281 ) ) ;
#3020 = CARTESIAN_POINT ( 'NONE',  ( 10.69687500061451679, -3.027376345333610441, -5.243569643749999898 ) ) ;
#3021 = CARTESIAN_POINT ( 'NONE',  ( 9.234375000614518214, -4.541064518000419881, 2.621784821874995952 ) ) ;
#3022 = CARTESIAN_POINT ( 'NONE',  ( 18.45937500061451431, 4.541064518000418104, -2.621784821874998173 ) ) ;
#3023 = ORIENTED_EDGE ( 'NONE', *, *, #4912, .T. ) ;
#3024 = CARTESIAN_POINT ( 'NONE',  ( 22.75312500061451360, -4.541064518000417216, -2.621784821875001281 ) ) ;
#3025 = EDGE_CURVE ( 'NONE', #38182, #55885, #22709, .T. ) ;
#3026 = CIRCLE ( 'NONE', #4197, 4.999999999999998224 ) ;
#3027 = CARTESIAN_POINT ( 'NONE',  ( 17.44687500061451857, -3.027376345333610441, -5.243569643749999898 ) ) ;
#3028 = CARTESIAN_POINT ( 'NONE',  ( 23.12812500061451360, -4.541064518000419881, 2.621784821874995952 ) ) ;
#3029 = CARTESIAN_POINT ( 'NONE',  ( 4.000000000000000000, 11.18750000000000178, 32.30940107675849049 ) ) ;
#3030 = CARTESIAN_POINT ( 'NONE',  ( 26.91562500061451146, 3.027376345333613106, -5.243569643749998122 ) ) ;
#3031 = CARTESIAN_POINT ( 'NONE',  ( 6.787500001229032520, -4.330127018922194537, 2.499999999999995559 ) ) ;
#3032 = ORIENTED_EDGE ( 'NONE', *, *, #18203, .F. ) ;
#3033 = CARTESIAN_POINT ( 'NONE',  ( 3.150000001229034119, -2.886751345948129988, 4.999999999999997335 ) ) ;
#3034 = CARTESIAN_POINT ( 'NONE',  ( 3.999999999999999112, 17.52499999999999858, -30.00000000000000000 ) ) ;
#3035 = CARTESIAN_POINT ( 'NONE',  ( 24.26250000122903216, 0.000000000000000000, 4.999999999999998224 ) ) ;
#3036 = CARTESIAN_POINT ( 'NONE',  ( 2.655984681222220721E-16, 14.21562499938548463, 25.66244784525396483 ) ) ;
#3037 = EDGE_CURVE ( 'NONE', #72150, #24785, #8967, .T. ) ;
#3038 = CARTESIAN_POINT ( 'NONE',  ( 7.809375000614519280, 0.000000000000000000, 5.243569643749999010 ) ) ;
#3039 = CARTESIAN_POINT ( 'NONE',  ( 12.82499999999999929, 4.330127018922191873, 2.499999999999999556 ) ) ;
#3040 = CARTESIAN_POINT ( 'NONE',  ( 14.72812500061451679, 6.421520780324663323E-16, -5.243569643749999010 ) ) ;
#3041 = CARTESIAN_POINT ( 'NONE',  ( 8.296875000614516438, -3.027376345333614438, 5.243569643749998122 ) ) ;
#3042 = CARTESIAN_POINT ( 'NONE',  ( 26.43750000122903288, 4.330127018922191873, 2.499999999999999556 ) ) ;
#3043 = CARTESIAN_POINT ( 'NONE',  ( 18.30937500061451928, -4.541064518000417216, -2.621784821875001281 ) ) ;
#3044 = CARTESIAN_POINT ( 'NONE',  ( 4.884375000614518569, 6.421520780324663323E-16, -5.243569643749999010 ) ) ;
#3045 = DIRECTION ( 'NONE',  ( -1.000000000000000000, -0.000000000000000000, -0.000000000000000000 ) ) ;
#3046 = EDGE_CURVE ( 'NONE', #17794, #72719, #54288, .T. ) ;
#3047 = CARTESIAN_POINT ( 'NONE',  ( 5.878125000614517148, 4.541064518000418104, 2.621784821874999949 ) ) ;
#3048 = CARTESIAN_POINT ( 'NONE',  ( 16.30312500061451786, 0.000000000000000000, 5.243569643749999010 ) ) ;
#3049 = ORIENTED_EDGE ( 'NONE', *, *, #50356, .F. ) ;
#3050 = CARTESIAN_POINT ( 'NONE',  ( 12.47812500061451502, 6.421520780324663323E-16, -5.243569643749999010 ) ) ;
#3051 = CARTESIAN_POINT ( 'NONE',  ( 4.875000001229034652, 2.886751345948126879, 4.999999999999999112 ) ) ;
#3052 = CARTESIAN_POINT ( 'NONE',  ( 11.80312500061451608, 0.000000000000000000, 5.243569643749999010 ) ) ;
#3053 = CARTESIAN_POINT ( 'NONE',  ( 21.45937500061451786, -4.119189519843965641, -2.378215178125001383 ) ) ;
#3054 = CARTESIAN_POINT ( 'NONE',  ( 11.96250000000000213, 2.886751345948126879, 4.999999999999999112 ) ) ;
#3055 = CARTESIAN_POINT ( 'NONE',  ( 7.687500001229033764, -4.330127018922194537, 2.499999999999995559 ) ) ;
#3056 = CARTESIAN_POINT ( 'NONE',  ( 20.69999999999999929, -4.330127018922190985, -2.500000000000001332 ) ) ;
#3057 = CARTESIAN_POINT ( 'NONE',  ( 13.84687500061451537, -3.027376345333610441, -5.243569643749999898 ) ) ;
#3058 = CARTESIAN_POINT ( 'NONE',  ( 17.10000000122903430, -2.886751345948129988, 4.999999999999997335 ) ) ;
#3059 = CARTESIAN_POINT ( 'NONE',  ( 22.83749999999999858, -2.886751345948129988, 4.999999999999997335 ) ) ;
#3060 = AXIS2_PLACEMENT_3D ( 'NONE', #34285, #693, #39859 ) ;
#3061 = CARTESIAN_POINT ( 'NONE',  ( 9.001249775931846008E-16, 18.11562500061451786, -25.09994784771203058 ) ) ;
#3062 = CARTESIAN_POINT ( 'NONE',  ( 25.27499999999999858, 6.123233995736764310E-16, -4.999999999999998224 ) ) ;
#3063 = CARTESIAN_POINT ( 'NONE',  ( 3.999999999999999112, 14.93750000122903288, -30.00000000000000000 ) ) ;
#3064 = CARTESIAN_POINT ( 'NONE',  ( 29.20312500061451644, 4.541064518000418104, -2.621784821874998173 ) ) ;
#3065 = EDGE_CURVE ( 'NONE', #50451, #66756, #62271, .T. ) ;
#3066 = CARTESIAN_POINT ( 'NONE',  ( 3.429892710759705476, -3.638108848382370919, 3.621991456395721620 ) ) ;
#3067 = CARTESIAN_POINT ( 'NONE',  ( 13.79999999999999893, 0.000000000000000000, 4.999999999999998224 ) ) ;
#3068 = CARTESIAN_POINT ( 'NONE',  ( 15.53437500061451715, -4.541064518000419881, 2.621784821874995952 ) ) ;
#3069 =( BOUNDED_CURVE ( )  B_SPLINE_CURVE ( 2, ( #24738, #69461, #63541, #68736, #28838, #2225, #62815 ),
 .UNSPECIFIED., .F., .F. ) 
 B_SPLINE_CURVE_WITH_KNOTS ( ( 3, 2, 2, 3 ),
 ( 0.3500000000000000888, 0.3533333333333333881, 0.3566666666666667429, 0.3599999999999999867 ),
 .UNSPECIFIED. ) 
 CURVE ( )  GEOMETRIC_REPRESENTATION_ITEM ( )  RATIONAL_B_SPLINE_CURVE ( ( 0.9999999999999955591, 0.8660254037844431485, 1.000000000000000000, 0.8660254037844387076, 1.000000000000000000, 0.8660254037844387076, 1.000000000000000000 ) ) 
 REPRESENTATION_ITEM ( '' )  );
#3070 = CARTESIAN_POINT ( 'NONE',  ( 27.89999999999999858, -4.330127018922190985, -2.500000000000001332 ) ) ;
#3071 = CARTESIAN_POINT ( 'NONE',  ( 11.87812500061451537, -4.541064518000419881, 2.621784821874995952 ) ) ;
#3072 = CARTESIAN_POINT ( 'NONE',  ( 7.181250001229034119, -4.330127018922194537, 2.499999999999995559 ) ) ;
#3073 = PRODUCT_DEFINITION_SHAPE ( 'NONE', 'NONE',  #73119 ) ;
#3074 = CARTESIAN_POINT ( 'NONE',  ( 22.73437500061451644, -4.541064518000419881, 2.621784821874995952 ) ) ;
#3075 = CARTESIAN_POINT ( 'NONE',  ( 16.99687500061451573, 4.119189519843966529, -2.378215178124998275 ) ) ;
#3076 = CARTESIAN_POINT ( 'NONE',  ( 9.965625000614517504, 3.027376345333611329, 5.243569643749999010 ) ) ;
#3077 = CARTESIAN_POINT ( 'NONE',  ( 12.30937500061451573, 0.000000000000000000, 5.243569643749999010 ) ) ;
#3078 = ORIENTED_EDGE ( 'NONE', *, *, #68758, .F. ) ;
#3079 = CARTESIAN_POINT ( 'NONE',  ( 24.68437500061451573, 6.421520780324663323E-16, -5.243569643749999010 ) ) ;
#3080 = CARTESIAN_POINT ( 'NONE',  ( 28.64062500061451289, -3.027376345333610441, -5.243569643749999898 ) ) ;
#3081 = CARTESIAN_POINT ( 'NONE',  ( 0.000000000000000000, 12.50000000000000000, 30.00000000000000000 ) ) ;
#3082 = CARTESIAN_POINT ( 'NONE',  ( 8.324999999999999289, 4.330127018922191873, 2.499999999999999556 ) ) ;
#3083 = CARTESIAN_POINT ( 'NONE',  ( 17.10000000122903430, -2.886751345948129988, 4.999999999999997335 ) ) ;
#3084 = DIRECTION ( 'NONE',  ( 0.000000000000000000, 0.000000000000000000, -1.000000000000000000 ) ) ;
#3085 = CARTESIAN_POINT ( 'NONE',  ( 3.286795329855858760, 3.767887532774327308, -3.286795329856085690 ) ) ;
#3086 = ORIENTED_EDGE ( 'NONE', *, *, #28669, .T. ) ;
#3087 = CARTESIAN_POINT ( 'NONE',  ( 14.69999999999999929, 0.000000000000000000, 4.999999999999998224 ) ) ;
#3088 = CARTESIAN_POINT ( 'NONE',  ( 20.13749999999999929, -2.886751345948129988, 4.999999999999997335 ) ) ;
#3089 = CARTESIAN_POINT ( 'NONE',  ( 12.74062500061451786, -3.027376345333614438, 5.243569643749998122 ) ) ;
#3090 = VERTEX_POINT ( 'NONE', #13068 ) ;
#3091 = CARTESIAN_POINT ( 'NONE',  ( 45.00000000000000000, 2.500000000000000444, 3.499999999999999112 ) ) ;
#3092 = CARTESIAN_POINT ( 'NONE',  ( 4.243569643749999898, 17.83437500061451786, -30.00000000000000000 ) ) ;
#3093 = CARTESIAN_POINT ( 'NONE',  ( 6.553125000614518747, -4.541064518000417216, -2.621784821875001281 ) ) ;
#3094 = DIRECTION ( 'NONE',  ( 1.000000000000000000, 0.000000000000000000, 0.000000000000000000 ) ) ;
#3095 = CARTESIAN_POINT ( 'NONE',  ( 12.75000000000000178, 4.330127018922192761, -2.499999999999997780 ) ) ;
#3096 = CARTESIAN_POINT ( 'NONE',  ( 28.17187500061451289, 5.824947211148865298E-16, -4.756430356249998326 ) ) ;
#3097 = ORIENTED_EDGE ( 'NONE', *, *, #60084, .T. ) ;
#3098 = CARTESIAN_POINT ( 'NONE',  ( -4.243569643749999898, 14.85312500061451679, 30.00000000000000000 ) ) ;
#3099 = CARTESIAN_POINT ( 'NONE',  ( 26.50312500061451360, 4.541064518000418104, -2.621784821874998173 ) ) ;
#3100 = CARTESIAN_POINT ( 'NONE',  ( 0.000000000000000000, 20.00000000000000000, 30.00000000000000000 ) ) ;
#3101 = CARTESIAN_POINT ( 'NONE',  ( -3.756430356250001434, 20.55312499938548498, 32.16877607737301048 ) ) ;
#3102 = CARTESIAN_POINT ( 'NONE',  ( 22.99687500061451573, 6.054752690667223547, 3.707466751127219781E-16 ) ) ;
#3103 = CARTESIAN_POINT ( 'NONE',  ( 18.10312500061451502, 0.000000000000000000, 5.243569643749999010 ) ) ;
#3104 = CARTESIAN_POINT ( 'NONE',  ( 4.243569643749999010, 15.11562500061459424, -32.45002607614398471 ) ) ;
#3105 = CARTESIAN_POINT ( 'NONE',  ( 22.91250000122903430, 0.000000000000000000, 4.999999999999998224 ) ) ;
#3106 = CARTESIAN_POINT ( 'NONE',  ( 3.028125000614518392, 6.421520780324663323E-16, -5.243569643749999010 ) ) ;
#3107 = CARTESIAN_POINT ( 'NONE',  ( 27.45937500061451786, 4.119189519843966529, -2.378215178124998275 ) ) ;
#3108 = CARTESIAN_POINT ( 'NONE',  ( 21.32812500061451644, -4.541064518000419881, 2.621784821874995952 ) ) ;
#3109 = CARTESIAN_POINT ( 'NONE',  ( 10.43437500061451750, 4.119189519843966529, 2.378215178124999607 ) ) ;
#3110 = CARTESIAN_POINT ( 'NONE',  ( 3.756430356249998770, 16.20312499938548356, 32.16877607737302469 ) ) ;
#3111 = CARTESIAN_POINT ( 'NONE',  ( 16.58437500061451786, 6.421520780324663323E-16, -5.243569643749999010 ) ) ;
#3112 = CARTESIAN_POINT ( 'NONE',  ( 16.58437500061451786, 6.421520780324663323E-16, -5.243569643749999010 ) ) ;
#3113 = CARTESIAN_POINT ( 'NONE',  ( 24.23437500061451644, 6.421520780324663323E-16, -5.243569643749999010 ) ) ;
#3114 = CARTESIAN_POINT ( 'NONE',  ( -4.243569643749999898, 13.07187500061452035, 27.54997392385601529 ) ) ;
#3115 = CARTESIAN_POINT ( 'NONE',  ( 5.615625000614517859, -6.054752690667223547, -1.112240025338166033E-15 ) ) ;
#3116 = CARTESIAN_POINT ( 'NONE',  ( 29.16562500061451502, 3.027376345333613106, -5.243569643749998122 ) ) ;
#3117 = CARTESIAN_POINT ( 'NONE',  ( 28.67812500061451431, 6.421520780324663323E-16, -5.243569643749999010 ) ) ;
#3118 = CARTESIAN_POINT ( 'NONE',  ( 45.00000000000000000, 0.000000000000000000, 4.999999999999998224 ) ) ;
#3119 = FACE_OUTER_BOUND ( 'NONE', #6310, .T. ) ;
#3120 = AXIS2_PLACEMENT_3D ( 'NONE', #19948, #42501, #14413 ) ;
#3121 = CARTESIAN_POINT ( 'NONE',  ( 3.590625000614518836, 6.054752690667223547, 3.707466751127219781E-16 ) ) ;
#3122 = CARTESIAN_POINT ( 'NONE',  ( 7.021875000614518747, -6.054752690667223547, -1.112240025338166033E-15 ) ) ;
#3123 = APPLICATION_PROTOCOL_DEFINITION ( 'draft international standard', 'automotive_design', 1998, #11543 ) ;
#3124 = CARTESIAN_POINT ( 'NONE',  ( 13.72500000122903074, 2.886751345948129099, -4.999999999999998224 ) ) ;
#3125 = CARTESIAN_POINT ( 'NONE',  ( 3.609375000614516882, 4.541064518000418104, -2.621784821874998173 ) ) ;
#3126 = CARTESIAN_POINT ( 'NONE',  ( 11.02500000122903501, 2.886751345948129099, -4.999999999999998224 ) ) ;
#3127 = CARTESIAN_POINT ( 'NONE',  ( 4.978125000614518569, 4.541064518000418104, 2.621784821874999949 ) ) ;
#3128 = CARTESIAN_POINT ( 'NONE',  ( 4.000000000000000000, 14.28124999877096535, 27.69059892324149530 ) ) ;
#3129 = CARTESIAN_POINT ( 'NONE',  ( 20.94375000122902719, 5.773502691896255534, 3.535250795749688894E-16 ) ) ;
#3130 = CARTESIAN_POINT ( 'NONE',  ( 14.59687500061452070, -3.027376345333614438, 5.243569643749998122 ) ) ;
#3131 = CARTESIAN_POINT ( 'NONE',  ( 0.000000000000000000, 20.00000000000000000, -30.00000000000000000 ) ) ;
#3132 = EDGE_LOOP ( 'NONE', ( #5371, #44532, #72446, #60602 ) ) ;
#3133 = CARTESIAN_POINT ( 'NONE',  ( 22.26562500061451644, -6.054752690667223547, -1.112240025338166033E-15 ) ) ;
#3134 = CARTESIAN_POINT ( 'NONE',  ( 7.303125000614516082, 0.000000000000000000, 5.243569643749999010 ) ) ;
#3135 = CARTESIAN_POINT ( 'NONE',  ( 24.04687500061451644, -3.027376345333614438, 5.243569643749998122 ) ) ;
#3136 = CARTESIAN_POINT ( 'NONE',  ( 6.403125000614517504, 0.000000000000000000, 5.243569643749999010 ) ) ;
#3137 = CARTESIAN_POINT ( 'NONE',  ( 3.495766807613835958, 4.011937492815293993, 3.051120425653408574 ) ) ;
#3139 = ADVANCED_FACE ( 'NONE', ( #51884 ), #35607, .F. ) ;
#3138 = CARTESIAN_POINT ( 'NONE',  ( 9.262500001229033941, 4.330127018922192761, -2.499999999999997780 ) ) ;
#3140 = EDGE_CURVE ( 'NONE', #72600, #46789, #39515, .T. ) ;
#3141 =( BOUNDED_CURVE ( )  B_SPLINE_CURVE ( 2, ( #30041, #52579, #8978, #48505, #48136, #41856, #69933 ),
 .UNSPECIFIED., .F., .F. ) 
 B_SPLINE_CURVE_WITH_KNOTS ( ( 3, 2, 2, 3 ),
 ( 0.5000000000000001110, 0.5033333333333334103, 0.5066666666666667096, 0.5100000000000000089 ),
 .UNSPECIFIED. ) 
 CURVE ( )  GEOMETRIC_REPRESENTATION_ITEM ( )  RATIONAL_B_SPLINE_CURVE ( ( 0.9999999999999955591, 0.8660254037844431485, 1.000000000000000000, 0.8660254037844387076, 1.000000000000000000, 0.8660254037844387076, 1.000000000000000000 ) ) 
 REPRESENTATION_ITEM ( '' )  );
#3142 = CARTESIAN_POINT ( 'NONE',  ( 22.60312500061451857, 0.000000000000000000, 5.243569643749999010 ) ) ;
#3143 = CARTESIAN_POINT ( 'NONE',  ( -2.121784821874999949, 11.62812500061451715, -33.67503911421598417 ) ) ;
#3144 = CARTESIAN_POINT ( 'NONE',  ( 9.525000001229033231, -5.773502691896255534, -1.060575238724906372E-15 ) ) ;
#3145 = CARTESIAN_POINT ( 'NONE',  ( 20.01562500061451644, -6.054752690667223547, -1.112240025338166033E-15 ) ) ;
#3146 = CARTESIAN_POINT ( 'NONE',  ( 18.36562500061451431, 3.027376345333613106, -5.243569643749998122 ) ) ;
#3147 = CARTESIAN_POINT ( 'NONE',  ( 29.29687500061451644, 5.492252693125287522, 3.363034840372157021E-16 ) ) ;
#3148 = CARTESIAN_POINT ( 'NONE',  ( 17.96250000000000213, -5.773502691896255534, -1.060575238724906372E-15 ) ) ;
#3149 = CARTESIAN_POINT ( 'NONE',  ( 14.43750000122903288, -4.330127018922194537, 2.499999999999995559 ) ) ;
#3150 = CARTESIAN_POINT ( 'NONE',  ( 9.365625000614519635, 3.027376345333613106, -5.243569643749998122 ) ) ;
#3151 = CARTESIAN_POINT ( 'NONE',  ( 13.82812500061451466, 6.421520780324663323E-16, -5.243569643749999010 ) ) ;
#3152 = CARTESIAN_POINT ( 'NONE',  ( 23.17500000122903359, 2.886751345948129099, -4.999999999999998224 ) ) ;
#3153 = CARTESIAN_POINT ( 'NONE',  ( 22.09687500061451715, 6.054752690667223547, 3.707466751127219781E-16 ) ) ;
#3154 = CARTESIAN_POINT ( 'NONE',  ( 20.59687500061451360, -3.027376345333610441, -5.243569643749999898 ) ) ;
#3155 = CARTESIAN_POINT ( 'NONE',  ( 3.546502191234963242, 3.524546877579638693, -3.882356442438433586 ) ) ;
#3156 = AXIS2_PLACEMENT_3D ( 'NONE', #73102, #22126, #5508 ) ;
#3157 = CARTESIAN_POINT ( 'NONE',  ( 7.125000001229033764, 2.886751345948126879, 4.999999999999999112 ) ) ;
#3158 = CARTESIAN_POINT ( 'NONE',  ( 6.121875000614517504, -6.054752690667223547, -1.112240025338166033E-15 ) ) ;
#3159 = CARTESIAN_POINT ( 'NONE',  ( 24.04687500061451644, -3.027376345333614438, 5.243569643749998122 ) ) ;
#3160 = CARTESIAN_POINT ( 'NONE',  ( 26.66250000122903430, -4.330127018922190985, -2.500000000000001332 ) ) ;
#3161 = CARTESIAN_POINT ( 'NONE',  ( 18.92812500061451431, 4.541064518000418104, 2.621784821874999949 ) ) ;
#3162 = CARTESIAN_POINT ( 'NONE',  ( 24.87187500061451573, 3.027376345333611329, 5.243569643749999010 ) ) ;
#3163 = CARTESIAN_POINT ( 'NONE',  ( 3.756430356249998770, 19.01562499938548356, 32.16877607737301759 ) ) ;
#3164 = CARTESIAN_POINT ( 'NONE',  ( -3.999999999999999112, 11.11250000122903536, -30.00000000000000000 ) ) ;
#3165 = VECTOR ( 'NONE', #44966, 1000.000000000000000 ) ;
#3166 = CARTESIAN_POINT ( 'NONE',  ( 11.00625000122903252, 4.330127018922192761, -2.499999999999997780 ) ) ;
#3167 = CARTESIAN_POINT ( 'NONE',  ( 4.396875000614516971, -3.027376345333610441, -5.243569643749999898 ) ) ;
#3168 = CARTESIAN_POINT ( 'NONE',  ( 18.29062500061451502, -3.027376345333610441, -5.243569643749999898 ) ) ;
#3169 = ORIENTED_EDGE ( 'NONE', *, *, #67378, .T. ) ;
#3170 = CARTESIAN_POINT ( 'NONE',  ( 11.51250000000000107, 2.886751345948126879, 4.999999999999998224 ) ) ;
#3171 = CARTESIAN_POINT ( 'NONE',  ( 24.32812500061451289, 4.541064518000418104, 2.621784821874999949 ) ) ;
#3172 = CARTESIAN_POINT ( 'NONE',  ( -1.071796769724496556, 16.04240381056766651, -26.00000000000000355 ) ) ;
#3173 = EDGE_CURVE ( 'NONE', #69337, #40700, #203, .T. ) ;
#3174 = CARTESIAN_POINT ( 'NONE',  ( 14.77500000000000036, -4.330127018922194537, 2.499999999999995559 ) ) ;
#3175 = CARTESIAN_POINT ( 'NONE',  ( 24.22500000122903430, 2.886751345948126879, 4.999999999999999112 ) ) ;
#3176 = CARTESIAN_POINT ( 'NONE',  ( 18.21562500061451573, -6.054752690667223547, -1.112240025338166033E-15 ) ) ;
#3177 = ORIENTED_EDGE ( 'NONE', *, *, #46955, .T. ) ;
#3178 = CARTESIAN_POINT ( 'NONE',  ( 22.98749999999999716, -2.886751345948125991, -5.000000000000000000 ) ) ;
#3179 = CARTESIAN_POINT ( 'NONE',  ( 23.70937500061451786, -4.541064518000417216, -2.621784821875001281 ) ) ;
#3180 = ORIENTED_EDGE ( 'NONE', *, *, #37148, .F. ) ;
#3181 = DIRECTION ( 'NONE',  ( 0.000000000000000000, 0.000000000000000000, 1.000000000000000000 ) ) ;
#3182 = CARTESIAN_POINT ( 'NONE',  ( 12.29062500061451857, -3.027376345333614438, 5.243569643749998122 ) ) ;
#3183 = CARTESIAN_POINT ( 'NONE',  ( 4.715625000614516615, -6.054752690667223547, -1.112240025338166033E-15 ) ) ;
#3184 = CARTESIAN_POINT ( 'NONE',  ( 16.80937500061451573, -5.492252693125287522, -1.008910452111647106E-15 ) ) ;
#3185 = CARTESIAN_POINT ( 'NONE',  ( 27.17812500061451786, -4.541064518000419881, 2.621784821874995952 ) ) ;
#3186 = CARTESIAN_POINT ( 'NONE',  ( 12.00000000122903465, 5.773502691896255534, 3.535250795749688894E-16 ) ) ;
#3187 = CARTESIAN_POINT ( 'NONE',  ( 20.54999999999999716, 0.000000000000000000, 4.999999999999998224 ) ) ;
#3188 = CARTESIAN_POINT ( 'NONE',  ( 25.72499999999999787, 6.123233995736764310E-16, -4.999999999999998224 ) ) ;
#3189 = CARTESIAN_POINT ( 'NONE',  ( 22.57499999999999929, 6.123233995736764310E-16, -4.999999999999998224 ) ) ;
#3190 = CARTESIAN_POINT ( 'NONE',  ( 7.134375000614516793, 6.421520780324663323E-16, -5.243569643749999010 ) ) ;
#3191 = CARTESIAN_POINT ( 'NONE',  ( 17.67187500061451644, 3.027376345333611329, 5.243569643749999010 ) ) ;
#3192 = DIRECTION ( 'NONE',  ( 1.000000000000000000, 0.000000000000000000, 0.000000000000000000 ) ) ;
#3193 = VERTEX_POINT ( 'NONE', #39726 ) ;
#3194 = CARTESIAN_POINT ( 'NONE',  ( 29.72812500061451502, 4.541064518000418104, 2.621784821874999949 ) ) ;
#3195 = CARTESIAN_POINT ( 'NONE',  ( 28.24687500061451573, -3.027376345333610441, -5.243569643749999898 ) ) ;
#3196 = CARTESIAN_POINT ( 'NONE',  ( 3.346875000614518036, -3.027376345333614438, 5.243569643749998122 ) ) ;
#3197 = CARTESIAN_POINT ( 'NONE',  ( 15.03749999999999964, 5.773502691896255534, 3.535250795749688894E-16 ) ) ;
#3198 = CARTESIAN_POINT ( 'NONE',  ( 14.31562500061451537, 3.027376345333613106, -5.243569643749998122 ) ) ;
#3199 = CARTESIAN_POINT ( 'NONE',  ( 3.486133158594716510E-16, 19.55000000122903359, -34.00000000000000000 ) ) ;
#3200 = CARTESIAN_POINT ( 'NONE',  ( 28.71562500061451573, 3.027376345333612662, -5.243569643749998122 ) ) ;
#3201 = CARTESIAN_POINT ( 'NONE',  ( 18.78750000122903430, 4.330127018922191873, 2.499999999999999556 ) ) ;
#3202 = LINE ( 'NONE', #48268, #1778 ) ;
#3203 = CARTESIAN_POINT ( 'NONE',  ( 18.19687500061451502, -2.746126346562646425, 4.756430356249996549 ) ) ;
#3204 = CARTESIAN_POINT ( 'NONE',  ( 8.165625000614516793, 3.027376345333611329, 5.243569643749999010 ) ) ;
#3205 = CARTESIAN_POINT ( 'NONE',  ( 23.37187500061451573, 3.027376345333613106, -5.243569643749998122 ) ) ;
#3206 = CARTESIAN_POINT ( 'NONE',  ( 4.243569643749999898, 16.48437500061451644, 30.00000000000000000 ) ) ;
#3207 = CARTESIAN_POINT ( 'NONE',  ( 23.70937500061451786, -4.541064518000417216, -2.621784821875001281 ) ) ;
#3208 = CARTESIAN_POINT ( 'NONE',  ( 4.087500000000001243, -2.886751345948125991, -5.000000000000000000 ) ) ;
#3209 = CARTESIAN_POINT ( 'NONE',  ( -2.828200636599751609E-16, 11.45000000122903394, 25.38119784648299770 ) ) ;
#3210 = CARTESIAN_POINT ( 'NONE',  ( 11.50312500061451892, -4.541064518000417216, -2.621784821875001281 ) ) ;
#3211 = CARTESIAN_POINT ( 'NONE',  ( 5.287500001229035185, 4.330127018922191873, 2.499999999999999556 ) ) ;
#3212 = CARTESIAN_POINT ( 'NONE',  ( 10.28437500061451715, 6.421520780324663323E-16, -5.243569643749999010 ) ) ;
#3213 = CARTESIAN_POINT ( 'NONE',  ( -3.026485248664591232, 3.985774251745327845, -27.37255237546152742 ) ) ;
#3214 = ORIENTED_EDGE ( 'NONE', *, *, #57780, .F. ) ;
#3215 = CARTESIAN_POINT ( 'NONE',  ( 10.19062500061451892, -3.027376345333610441, -5.243569643749999898 ) ) ;
#3216 = CARTESIAN_POINT ( 'NONE',  ( 14.74687500061451573, -3.027376345333610441, -5.243569643749999898 ) ) ;
#3217 = CARTESIAN_POINT ( 'NONE',  ( 1.626862140677534273E-15, 12.12500000122903465, -26.00000000000000355 ) ) ;
#3218 = CARTESIAN_POINT ( 'NONE',  ( 22.31250000122903288, 4.330127018922192761, -2.499999999999997780 ) ) ;
#3219 = CARTESIAN_POINT ( 'NONE',  ( 9.271875000614516082, -6.054752690667223547, -1.112240025338166033E-15 ) ) ;
#3220 = CARTESIAN_POINT ( 'NONE',  ( 12.21562500061451573, 3.027376345333611329, 5.243569643749999010 ) ) ;
#3221 = CARTESIAN_POINT ( 'NONE',  ( 27.05625000122903145, -4.330127018922190985, -2.500000000000001332 ) ) ;
#3222 = CARTESIAN_POINT ( 'NONE',  ( 20.93437500061451573, -4.541064518000419881, 2.621784821874995952 ) ) ;
#3223 = CARTESIAN_POINT ( 'NONE',  ( 14.02499999999999858, 6.123233995736764310E-16, -4.999999999999998224 ) ) ;
#3224 = AXIS2_PLACEMENT_3D ( 'NONE', #12254, #46972, #34423 ) ;
#3225 = CARTESIAN_POINT ( 'NONE',  ( 0.000000000000000000, 4.999999999999998224, 0.000000000000000000 ) ) ;
#3226 = EDGE_CURVE ( 'NONE', #34155, #66981, #56656, .T. ) ;
#3227 = CARTESIAN_POINT ( 'NONE',  ( 4.243569643749999898, 13.78437500061451715, -30.00000000000000000 ) ) ;
#3228 = CARTESIAN_POINT ( 'NONE',  ( 15.72187500061451892, 3.027376345333613106, -5.243569643749998122 ) ) ;
#3229 = CARTESIAN_POINT ( 'NONE',  ( 16.12500000122903288, 2.886751345948126879, 4.999999999999999112 ) ) ;
#3230 = EDGE_CURVE ( 'NONE', #69635, #14969, #49540, .T. ) ;
#3231 = CARTESIAN_POINT ( 'NONE',  ( 12.27187500061451786, 3.027376345333611329, 5.243569643749999010 ) ) ;
#3232 = CARTESIAN_POINT ( 'NONE',  ( 9.001249775931846008E-16, 18.11562500061451786, -25.09994784771203058 ) ) ;
#3233 = CARTESIAN_POINT ( 'NONE',  ( 17.47500000122903430, 2.886751345948126879, 4.999999999999999112 ) ) ;
#3234 = CARTESIAN_POINT ( 'NONE',  ( 11.50312500061451892, -4.541064518000417216, -2.621784821875001281 ) ) ;
#3235 = ORIENTED_EDGE ( 'NONE', *, *, #32753, .T. ) ;
#3236 = CARTESIAN_POINT ( 'NONE',  ( 14.73749999999999893, -2.886751345948129988, 4.999999999999997335 ) ) ;
#3237 = CARTESIAN_POINT ( 'NONE',  ( 10.95937500061451964, 0.000000000000000000, 5.243569643749999010 ) ) ;
#3238 = FACE_OUTER_BOUND ( 'NONE', #30268, .T. ) ;
#3239 = CARTESIAN_POINT ( 'NONE',  ( 12.48750000122903359, 4.330127018922191873, 2.499999999999999556 ) ) ;
#3240 = CARTESIAN_POINT ( 'NONE',  ( 20.43750000122903643, 6.123233995736764310E-16, -4.999999999999998224 ) ) ;
#3241 = CARTESIAN_POINT ( 'NONE',  ( 18.66562500061451146, -6.054752690667223547, -1.112240025338166033E-15 ) ) ;
#3242 = CARTESIAN_POINT ( 'NONE',  ( 19.64062500061451644, -3.027376345333610441, -5.243569643749999898 ) ) ;
#3243 = CARTESIAN_POINT ( 'NONE',  ( 28.98750000122903359, 6.123233995736764310E-16, -4.999999999999998224 ) ) ;
#3244 = CARTESIAN_POINT ( 'NONE',  ( 4.228125000614517681, -4.541064518000419881, 2.621784821874995952 ) ) ;
#3245 = CARTESIAN_POINT ( 'NONE',  ( 25.64999999999999858, -4.330127018922190985, -2.500000000000001332 ) ) ;
#3246 = CARTESIAN_POINT ( 'NONE',  ( 17.53125000122903288, -4.330127018922194537, 2.499999999999995559 ) ) ;
#3247 = CARTESIAN_POINT ( 'NONE',  ( 7.809375000614519280, 0.000000000000000000, 4.756430356249998326 ) ) ;
#3248 = CARTESIAN_POINT ( 'NONE',  ( 27.42187500061451644, 3.027376345333613106, -5.243569643749998122 ) ) ;
#3249 = CARTESIAN_POINT ( 'NONE',  ( 28.64999999999999858, 0.000000000000000000, 4.999999999999998224 ) ) ;
#3250 = CARTESIAN_POINT ( 'NONE',  ( -4.243569643749997233, 13.59687500061451715, -27.54997392385601174 ) ) ;
#3251 = CARTESIAN_POINT ( 'NONE',  ( 3.525000001229034119, 2.886751345948126879, 4.999999999999999112 ) ) ;
#3252 = CARTESIAN_POINT ( 'NONE',  ( 3.262500000000001510, 2.886751345948129099, -4.999999999999998224 ) ) ;
#3253 = CARTESIAN_POINT ( 'NONE',  ( 27.33750000000000213, -2.886751345948088243, 5.000000000000068390 ) ) ;
#3254 = CARTESIAN_POINT ( 'NONE',  ( 8.221875000614518925, 3.027376345333611329, 5.243569643749999010 ) ) ;
#3255 = CARTESIAN_POINT ( 'NONE',  ( 25.97812500061451502, 6.421520780324663323E-16, -5.243569643749999010 ) ) ;
#3256 = DIRECTION ( 'NONE',  ( -0.000000000000000000, -1.000000000000000000, -0.000000000000000000 ) ) ;
#3257 = CARTESIAN_POINT ( 'NONE',  ( 11.66250000122903430, 0.000000000000000000, 4.999999999999998224 ) ) ;
#3258 = LINE ( 'NONE', #42776, #39487 ) ;
#3259 = CARTESIAN_POINT ( 'NONE',  ( 6.309375000614517504, 4.541064518000418104, -2.621784821874998173 ) ) ;
#3260 = CARTESIAN_POINT ( 'NONE',  ( 9.346875000614517148, -3.027376345333610441, -5.243569643749999898 ) ) ;
#3261 = CARTESIAN_POINT ( 'NONE',  ( 3.487500000000000711, -2.886751345948129988, 4.999999999999997335 ) ) ;
#3262 = AXIS2_PLACEMENT_3D ( 'NONE', #70429, #46444, #7280 ) ;
#3263 = CARTESIAN_POINT ( 'NONE',  ( 2.121784821874999061, 11.55312500061459424, 26.32496088578401583 ) ) ;
#3264 = CARTESIAN_POINT ( 'NONE',  ( 30.00000000000000000, 0.000000000000000000, 4.999999999999998224 ) ) ;
#3265 = CARTESIAN_POINT ( 'NONE',  ( 3.112500000000000711, -5.773502691896255534, -1.060575238724906372E-15 ) ) ;
#3266 = CARTESIAN_POINT ( 'NONE',  ( 16.13437500061451502, 5.492252693125287522, 3.363034840372157021E-16 ) ) ;
#3267 = ORIENTED_EDGE ( 'NONE', *, *, #14679, .F. ) ;
#3268 = CARTESIAN_POINT ( 'NONE',  ( 20.09062500061451573, -3.027376345333610441, -5.243569643749999898 ) ) ;
#3269 = CARTESIAN_POINT ( 'NONE',  ( 10.00312500061451715, 0.000000000000000000, 5.243569643749999010 ) ) ;
#3270 = CARTESIAN_POINT ( 'NONE',  ( 23.74687500061451573, 4.119189519843966529, -2.378215178124998275 ) ) ;
#3271 = CARTESIAN_POINT ( 'NONE',  ( 6.871875000614517504, 3.027376345333611329, 5.243569643749999010 ) ) ;
#3272 = CARTESIAN_POINT ( 'NONE',  ( 26.58750000000000213, -2.886751345948125991, -5.000000000000000000 ) ) ;
#3273 = CARTESIAN_POINT ( 'NONE',  ( 20.70000000122903216, -2.886751345948129988, 4.999999999999997335 ) ) ;
#3274 = CARTESIAN_POINT ( 'NONE',  ( 27.55312500061451786, 0.000000000000000000, 5.243569643749999010 ) ) ;
#3275 = CARTESIAN_POINT ( 'NONE',  ( 15.88125000122903074, 6.123233995736764310E-16, -4.999999999999998224 ) ) ;
#3276 = CARTESIAN_POINT ( 'NONE',  ( 10.50937500061451679, 0.000000000000000000, 5.243569643749999010 ) ) ;
#3277 = CARTESIAN_POINT ( 'NONE',  ( 14.03437500061451715, 4.541064518000418104, 2.621784821874999949 ) ) ;
#3278 = CARTESIAN_POINT ( 'NONE',  ( 25.95937500061451431, -4.541064518000417216, -2.621784821875001281 ) ) ;
#3279 = CARTESIAN_POINT ( 'NONE',  ( 4.898587196589411843E-16, 20.00000000000000000, -26.00000000000000000 ) ) ;
#3280 = CARTESIAN_POINT ( 'NONE',  ( 14.02499999999999858, 6.123233995736764310E-16, -4.999999999999998224 ) ) ;
#3281 = CARTESIAN_POINT ( 'NONE',  ( 19.92187500061451644, 3.027376345333611329, 5.243569643749999010 ) ) ;
#3282 = CARTESIAN_POINT ( 'NONE',  ( 13.02187500061451608, 3.027376345333613106, -5.243569643749998122 ) ) ;
#3283 = CARTESIAN_POINT ( 'NONE',  ( -1.878215178125001827, 20.70312499938548001, 33.25316411605952283 ) ) ;
#3284 = CARTESIAN_POINT ( 'NONE',  ( 22.94999999999999929, -4.330127018922190985, -2.500000000000001332 ) ) ;
#3285 = CARTESIAN_POINT ( 'NONE',  ( -4.000000000000000888, 15.46250000000000036, 32.30940107675850470 ) ) ;
#3286 = CARTESIAN_POINT ( 'NONE',  ( 2.121784821875001281, 11.45937500061451786, -26.32496088578401938 ) ) ;
#3287 = CARTESIAN_POINT ( 'NONE',  ( 24.98437500061451644, -4.119189519843968306, 2.378215178124996054 ) ) ;
#3288 = CARTESIAN_POINT ( 'NONE',  ( 13.90312500061451750, 4.541064518000418104, -2.621784821874998173 ) ) ;
#3289 = CARTESIAN_POINT ( 'NONE',  ( 5.025000000000002132, 6.123233995736764310E-16, -4.999999999999998224 ) ) ;
#3290 =( BOUNDED_CURVE ( )  B_SPLINE_CURVE ( 2, ( #30362, #18528, #52169, #18885, #63244, #46991, #36266 ),
 .UNSPECIFIED., .F., .F. ) 
 B_SPLINE_CURVE_WITH_KNOTS ( ( 3, 2, 2, 3 ),
 ( 0.000000000000000000, 0.003333333333333326608, 0.006666666666666653217, 0.009999999999999979391 ),
 .UNSPECIFIED. ) 
 CURVE ( )  GEOMETRIC_REPRESENTATION_ITEM ( )  RATIONAL_B_SPLINE_CURVE ( ( 1.000000000000000000, 0.8660254037844387076, 1.000000000000000000, 0.8660254037844387076, 1.000000000000000000, 0.8660254037844395958, 0.9999999999999991118 ) ) 
 REPRESENTATION_ITEM ( '' )  );
#3291 = CARTESIAN_POINT ( 'NONE',  ( -1.071796769724490117, 19.12009619066136423, -34.00000000000000000 ) ) ;
#3292 = CARTESIAN_POINT ( 'NONE',  ( 1.626862140677534273E-15, 9.875000001229034652, -26.00000000000000355 ) ) ;
#3293 = CARTESIAN_POINT ( 'NONE',  ( 12.11250000000000249, -5.773502691896255534, -1.060575238724906372E-15 ) ) ;
#3294 = CARTESIAN_POINT ( 'NONE',  ( 3.999999999999999112, 18.98750000122903359, 30.00000000000000000 ) ) ;
#3295 = CARTESIAN_POINT ( 'NONE',  ( 11.40000000122903501, -2.886751345948125991, -5.000000000000000000 ) ) ;
#3296 = EDGE_CURVE ( 'NONE', #26188, #27675, #53328, .T. ) ;
#3297 = CARTESIAN_POINT ( 'NONE',  ( 22.28437500061451715, -4.541064518000419881, 2.621784821874995952 ) ) ;
#3298 = CARTESIAN_POINT ( 'NONE',  ( 17.44687500061451857, -3.027376345333610441, -5.243569643749999898 ) ) ;
#3299 = LINE ( 'NONE', #13628, #11247 ) ;
#3300 = ORIENTED_EDGE ( 'NONE', *, *, #46331, .T. ) ;
#3301 = CARTESIAN_POINT ( 'NONE',  ( 17.35312500061451502, -4.541064518000417216, -2.621784821875001281 ) ) ;
#3302 = CARTESIAN_POINT ( 'NONE',  ( 3.103125000614517237, 4.541064518000418104, -2.621784821874998173 ) ) ;
#3303 = CARTESIAN_POINT ( 'NONE',  ( 18.45937500061451431, 4.541064518000418104, -2.621784821874998173 ) ) ;
#3304 = CARTESIAN_POINT ( 'NONE',  ( 29.22187500061451715, 3.027376345333613106, -5.243569643749998122 ) ) ;
#3305 = CARTESIAN_POINT ( 'NONE',  ( 4.528125000614516615, 4.541064518000418104, 2.621784821874999949 ) ) ;
#3306 = CARTESIAN_POINT ( 'NONE',  ( 19.11562500061451431, -6.054752690667223547, -1.112240025338166033E-15 ) ) ;
#3307 = CARTESIAN_POINT ( 'NONE',  ( -4.243569643749997233, 12.19062500061451715, 32.45002607614398471 ) ) ;
#3308 = CARTESIAN_POINT ( 'NONE',  ( 16.38750000122903216, 6.123233995736764310E-16, -4.999999999999998224 ) ) ;
#3309 = CARTESIAN_POINT ( 'NONE',  ( 11.52187500061451608, -5.492252693125287522, -1.008910452111647106E-15 ) ) ;
#3310 = CARTESIAN_POINT ( 'NONE',  ( 6.328125000614515550, 4.541064518000418104, 2.621784821874999949 ) ) ;
#3311 = CARTESIAN_POINT ( 'NONE',  ( 26.24062500061451431, -3.027376345333614438, 5.243569643749998122 ) ) ;
#3312 = CARTESIAN_POINT ( 'NONE',  ( 11.77500000000000036, 6.123233995736764310E-16, -4.999999999999998224 ) ) ;
#3313 = CARTESIAN_POINT ( 'NONE',  ( 23.70937500061451786, -4.541064518000417216, -2.621784821875001281 ) ) ;
#3314 = CARTESIAN_POINT ( 'NONE',  ( 15.47812500061451679, -4.541064518000419881, 2.621784821874995952 ) ) ;
#3315 = CARTESIAN_POINT ( 'NONE',  ( 24.26250000122903216, 0.000000000000000000, 4.999999999999998224 ) ) ;
#3316 = EDGE_CURVE ( 'NONE', #2861, #7111, #61832, .T. ) ;
#3317 = CARTESIAN_POINT ( 'NONE',  ( 23.31562500061451715, 3.027376345333613106, -5.243569643749998122 ) ) ;
#3318 = CARTESIAN_POINT ( 'NONE',  ( 20.10937500061451289, -4.541064518000417216, -2.621784821875001281 ) ) ;
#3319 = CARTESIAN_POINT ( 'NONE',  ( 13.67812500061451786, -4.541064518000419881, 2.621784821874995952 ) ) ;
#3320 = CARTESIAN_POINT ( 'NONE',  ( 4.243569643749999898, 15.09687500061451892, 32.45002607614398471 ) ) ;
#3321 = CARTESIAN_POINT ( 'NONE',  ( 18.92812500061451431, 4.541064518000418104, 2.621784821874999949 ) ) ;
#3322 = CARTESIAN_POINT ( 'NONE',  ( 29.69062500061451715, 6.054752690667223547, 3.707466751127219781E-16 ) ) ;
#3323 = ORIENTED_EDGE ( 'NONE', *, *, #24627, .F. ) ;
#3324 = VERTEX_POINT ( 'NONE', #20057 ) ;
#3325 = CARTESIAN_POINT ( 'NONE',  ( 23.85000000000000142, -4.330127018922190985, -2.500000000000001332 ) ) ;
#3326 = CARTESIAN_POINT ( 'NONE',  ( -3.999999999999997335, 11.03750000000000142, -27.69059892324149175 ) ) ;
#3327 = CARTESIAN_POINT ( 'NONE',  ( 16.12500000000000000, -4.330127018922194537, 2.499999999999995559 ) ) ;
#3328 = CARTESIAN_POINT ( 'NONE',  ( 25.90312500061451573, -4.541064518000417216, -2.621784821875001281 ) ) ;
#3329 = CARTESIAN_POINT ( 'NONE',  ( 7.190625000614518036, 6.054752690667223547, 3.707466751127219781E-16 ) ) ;
#3330 = CARTESIAN_POINT ( 'NONE',  ( 19.12500000122903288, 2.886751345948129099, -4.999999999999998224 ) ) ;
#3331 = AXIS2_PLACEMENT_3D ( 'NONE', #51135, #6790, #28243 ) ;
#3332 = CARTESIAN_POINT ( 'NONE',  ( 25.56562500061452070, 3.027376345333613106, -5.243569643749998122 ) ) ;
#3333 = CARTESIAN_POINT ( 'NONE',  ( 22.68750000000000000, 5.773502691896255534, 3.535250795749688894E-16 ) ) ;
#3334 = EDGE_CURVE ( 'NONE', #68472, #39806, #37194, .T. ) ;
#3335 = CARTESIAN_POINT ( 'NONE',  ( 27.74062500061451431, -3.027376345333610441, -5.243569643749999898 ) ) ;
#3336 = CARTESIAN_POINT ( 'NONE',  ( 9.253125000614517148, -4.541064518000417216, -2.621784821875001281 ) ) ;
#3337 = ORIENTED_EDGE ( 'NONE', *, *, #39334, .T. ) ;
#3338 = CARTESIAN_POINT ( 'NONE',  ( 22.79062500061451502, -3.027376345333610441, -5.243569643749999898 ) ) ;
#3339 = CARTESIAN_POINT ( 'NONE',  ( 4.153125000614515727, 0.000000000000000000, 5.243569643749999010 ) ) ;
#3340 = UNCERTAINTY_MEASURE_WITH_UNIT (LENGTH_MEASURE( 1.000000000000000082E-05 ), #12739, 'distance_accuracy_value', 'NONE');
#3341 = CARTESIAN_POINT ( 'NONE',  ( 14.44687500061451679, 5.492252693125287522, 3.363034840372157021E-16 ) ) ;
#3342 = CARTESIAN_POINT ( 'NONE',  ( 3.703125000614516882, 0.000000000000000000, 5.243569643749999010 ) ) ;
#3343 = CARTESIAN_POINT ( 'NONE',  ( 3.999999999999998668, 13.62500000122903288, -32.30940107675850470 ) ) ;
#3344 = CARTESIAN_POINT ( 'NONE',  ( -1.071796769724488563, 10.30490381179670045, 34.00000000000000000 ) ) ;
#3345 =( BOUNDED_CURVE ( )  B_SPLINE_CURVE ( 2, ( #30261, #30988, #9917, #32455, #60884, #66437, #37262 ),
 .UNSPECIFIED., .F., .F. ) 
 B_SPLINE_CURVE_WITH_KNOTS ( ( 3, 2, 2, 3 ),
 ( 0.8416666666666667851, 0.8444444444444445530, 0.8472222222222222099, 0.8499999999999999778 ),
 .UNSPECIFIED. ) 
 CURVE ( )  GEOMETRIC_REPRESENTATION_ITEM ( )  RATIONAL_B_SPLINE_CURVE ( ( 0.9999999999999946709, 0.8660254037844440367, 1.000000000000000000, 0.8660254037844387076, 1.000000000000000000, 0.8660254037844387076, 1.000000000000000000 ) ) 
 REPRESENTATION_ITEM ( '' )  );
#3346 = CARTESIAN_POINT ( 'NONE',  ( 11.32500000000000107, 6.123233995736764310E-16, -4.999999999999998224 ) ) ;
#3347 = CARTESIAN_POINT ( 'NONE',  ( 10.24687500061451750, -3.027376345333610441, -5.243569643749999898 ) ) ;
#3348 = CARTESIAN_POINT ( 'NONE',  ( 8.437500001229034652, 4.330127018922191873, 2.499999999999999556 ) ) ;
#3349 = CARTESIAN_POINT ( 'NONE',  ( 15.75937500061451857, 4.541064518000418104, -2.621784821874998173 ) ) ;
#3350 = CARTESIAN_POINT ( 'NONE',  ( 14.43750000000000000, -2.886751345948125991, -5.000000000000000000 ) ) ;
#3351 = CARTESIAN_POINT ( 'NONE',  ( 6.009375000614519458, 0.000000000000000000, 5.243569643749999010 ) ) ;
#3352 = CARTESIAN_POINT ( 'NONE',  ( 3.999999999999999112, 18.42500000000000071, 30.00000000000000000 ) ) ;
#3353 = LINE ( 'NONE', #25875, #13495 ) ;
#3354 = CARTESIAN_POINT ( 'NONE',  ( 12.30937500061451573, 0.000000000000000000, 5.243569643749999010 ) ) ;
#3355 = DIRECTION ( 'NONE',  ( 0.000000000000000000, 0.000000000000000000, 1.000000000000000000 ) ) ;
#3356 = CARTESIAN_POINT ( 'NONE',  ( 23.01562500061451644, 3.027376345333611329, 5.243569643749999010 ) ) ;
#3357 = CARTESIAN_POINT ( 'NONE',  ( 1.071796769724476572, 11.58259618943233349, 34.00000000000000000 ) ) ;
#3358 = CARTESIAN_POINT ( 'NONE',  ( 19.96875000122903288, 2.886751345948073588, -5.000000000000094147 ) ) ;
#3359 = CARTESIAN_POINT ( 'NONE',  ( 25.69687500061451502, 6.054752690667223547, 3.707466751127219781E-16 ) ) ;
#3360 = CARTESIAN_POINT ( 'NONE',  ( 1.999999999999997335, 16.47500000000000142, 33.46410161513775705 ) ) ;
#3361 =( BOUNDED_CURVE ( )  B_SPLINE_CURVE ( 2, ( #72373, #21753, #38767, #10679, #5142, #50215, #27677 ),
 .UNSPECIFIED., .F., .T. ) 
 B_SPLINE_CURVE_WITH_KNOTS ( ( 3, 2, 2, 3 ),
 ( 0.05000000000000003053, 0.05277777777777779844, 0.05555555555555556635, 0.05833333333333334120 ),
 .UNSPECIFIED. ) 
 CURVE ( )  GEOMETRIC_REPRESENTATION_ITEM ( )  RATIONAL_B_SPLINE_CURVE ( ( 0.9999999999999986677, 0.8660254037844400399, 1.000000000000000000, 0.8660254037844387076, 1.000000000000000000, 0.8660254037844383745, 1.000000000000000222 ) ) 
 REPRESENTATION_ITEM ( '' )  );
#3362 = CARTESIAN_POINT ( 'NONE',  ( 5.653125000614517504, -4.541064518000417216, -2.621784821875001281 ) ) ;
#3363 = CARTESIAN_POINT ( 'NONE',  ( 21.90937500061451715, 2.746126346562645981, -4.756430356249997438 ) ) ;
#3364 = CARTESIAN_POINT ( 'NONE',  ( 17.03437500061451715, 6.421520780324663323E-16, -5.243569643749999010 ) ) ;
#3365 = CARTESIAN_POINT ( 'NONE',  ( 9.196875000614515017, -4.119189519843965641, -2.378215178125001383 ) ) ;
#3366 = CARTESIAN_POINT ( 'NONE',  ( 26.43750000122903288, 4.330127018922191873, 2.499999999999999556 ) ) ;
#3367 = CARTESIAN_POINT ( 'NONE',  ( 6.421875000614519102, 3.027376345333611329, 5.243569643749999010 ) ) ;
#3368 = CARTESIAN_POINT ( 'NONE',  ( 15.90937500061451892, 0.000000000000000000, 5.243569643749999010 ) ) ;
#3369 = CARTESIAN_POINT ( 'NONE',  ( -0.5270301578798420872, 25.53585070951882230, 26.02618134498960245 ) ) ;
#3370 = CARTESIAN_POINT ( 'NONE',  ( 23.77499999999999858, -4.330127018922194537, 2.499999999999995559 ) ) ;
#3371 = CARTESIAN_POINT ( 'NONE',  ( 3.150000001229034119, -2.886751345948129988, 4.999999999999997335 ) ) ;
#3372 = CARTESIAN_POINT ( 'NONE',  ( 28.28437500061451715, 6.421520780324663323E-16, -5.243569643749999010 ) ) ;
#3373 = CARTESIAN_POINT ( 'NONE',  ( 4.000000000000000000, 15.65000000000000036, 30.00000000000000000 ) ) ;
#3374 = CARTESIAN_POINT ( 'NONE',  ( 29.96250000000000213, 2.886751345948126879, 4.999999999999999112 ) ) ;
#3375 = CARTESIAN_POINT ( 'NONE',  ( 7.537500000000002309, -2.886751345948129988, 4.999999999999997335 ) ) ;
#3376 = CARTESIAN_POINT ( 'NONE',  ( 8.821875000614515017, 5.824947211148865298E-16, -4.756430356249998326 ) ) ;
#3377 = CARTESIAN_POINT ( 'NONE',  ( 21.62812500061451360, 4.541064518000418104, 2.621784821874999949 ) ) ;
#3378 = CARTESIAN_POINT ( 'NONE',  ( 10.65000000000000036, 0.000000000000000000, 4.999999999999998224 ) ) ;
#3379 = CARTESIAN_POINT ( 'NONE',  ( 3.628125000614518036, 4.541064518000418104, 2.621784821874999949 ) ) ;
#3380 = CARTESIAN_POINT ( 'NONE',  ( 20.69999999999999929, -4.330127018922190985, -2.500000000000001332 ) ) ;
#3381 = CARTESIAN_POINT ( 'NONE',  ( 18.10312500061451502, 0.000000000000000000, 5.243569643749999010 ) ) ;
#3382 = DIRECTION ( 'NONE',  ( -1.000000000000000000, -0.000000000000000000, -0.000000000000000000 ) ) ;
#3383 = CARTESIAN_POINT ( 'NONE',  ( 23.21250000122903501, 4.330127018922192761, -2.499999999999997780 ) ) ;
#3384 = CARTESIAN_POINT ( 'NONE',  ( -3.756430356250000990, 19.65312499938548640, 32.16877607737301048 ) ) ;
#3385 =( BOUNDED_CURVE ( )  B_SPLINE_CURVE ( 2, ( #40780, #51856, #46679, #27975, #57744, #1258, #18578 ),
 .UNSPECIFIED., .F., .F. ) 
 B_SPLINE_CURVE_WITH_KNOTS ( ( 3, 2, 2, 3 ),
 ( 0.2399999999999999634, 0.2433333333333333182, 0.2466666666666666452, 0.2499999999999999722 ),
 .UNSPECIFIED. ) 
 CURVE ( )  GEOMETRIC_REPRESENTATION_ITEM ( )  RATIONAL_B_SPLINE_CURVE ( ( 1.000000000000001110, 0.8660254037844374864, 1.000000000000000000, 0.8660254037844387076, 1.000000000000000000, 0.8660254037844398178, 0.9999999999999988898 ) ) 
 REPRESENTATION_ITEM ( '' )  );
#3386 = CARTESIAN_POINT ( 'NONE',  ( 3.225000000000002309, 6.123233995736764310E-16, -4.999999999999998224 ) ) ;
#3387 = ORIENTED_EDGE ( 'NONE', *, *, #58181, .F. ) ;
#3388 = CARTESIAN_POINT ( 'NONE',  ( 19.82812500061451644, 4.541064518000418104, 2.621784821874999949 ) ) ;
#3389 = CARTESIAN_POINT ( 'NONE',  ( 27.14062500061451644, -3.027376345333614438, 5.243569643749998122 ) ) ;
#3390 = CARTESIAN_POINT ( 'NONE',  ( 25.92187500061451999, -6.054752690667223547, -1.112240025338166033E-15 ) ) ;
#3391 = CARTESIAN_POINT ( 'NONE',  ( 8.625000000000000000, 6.123233995736764310E-16, -4.999999999999998224 ) ) ;
#3392 = CARTESIAN_POINT ( 'NONE',  ( 11.80312500061451608, 0.000000000000000000, 5.243569643749999010 ) ) ;
#3393 = CARTESIAN_POINT ( 'NONE',  ( 26.20312500061451644, 0.000000000000000000, 5.243569643749999010 ) ) ;
#3394 = CARTESIAN_POINT ( 'NONE',  ( 17.74687500061451928, -3.027376345333614438, 5.243569643749998122 ) ) ;
#3395 = CARTESIAN_POINT ( 'NONE',  ( 9.215625000614515727, -6.054752690667223547, -1.112240025338166033E-15 ) ) ;
#3396 = CARTESIAN_POINT ( 'NONE',  ( 4.000000000000000000, 14.73124999877096641, 27.69059892324149885 ) ) ;
#3397 = CARTESIAN_POINT ( 'NONE',  ( 9.001249775931846008E-16, 11.87187500061451750, 34.90005215228797653 ) ) ;
#3398 = CARTESIAN_POINT ( 'NONE',  ( 23.21250000122903501, 4.330127018922192761, -2.499999999999997780 ) ) ;
#3399 = CARTESIAN_POINT ( 'NONE',  ( 18.57187500061451857, 2.746126346562643317, 4.756430356249998326 ) ) ;
#3400 = CARTESIAN_POINT ( 'NONE',  ( 13.94062500061451537, 6.054752690667223547, 3.707466751127219781E-16 ) ) ;
#3401 = CARTESIAN_POINT ( 'NONE',  ( 9.571875000614518569, 3.027376345333611329, 5.243569643749999010 ) ) ;
#3402 = CARTESIAN_POINT ( 'NONE',  ( 9.084375000614517859, 4.541064518000418104, 2.621784821874999949 ) ) ;
#3403 = ORIENTED_EDGE ( 'NONE', *, *, #31488, .F. ) ;
#3404 = FACE_OUTER_BOUND ( 'NONE', #25177, .T. ) ;
#3405 = CARTESIAN_POINT ( 'NONE',  ( 21.29062500061451502, -3.027376345333614438, 5.243569643749998122 ) ) ;
#3406 = EDGE_CURVE ( 'NONE', #69693, #30697, #11344, .T. ) ;
#3407 = CARTESIAN_POINT ( 'NONE',  ( 16.88437500061451502, -4.541064518000419881, 2.621784821874995952 ) ) ;
#3408 = CARTESIAN_POINT ( 'NONE',  ( 22.64062500061451644, -3.027376345333614438, 5.243569643749998122 ) ) ;
#3409 = CARTESIAN_POINT ( 'NONE',  ( 1.999999999999998668, 10.85000000000000142, 26.53589838486224650 ) ) ;
#3410 = CARTESIAN_POINT ( 'NONE',  ( 27.36562500061451786, 3.027376345333613106, -5.243569643749998122 ) ) ;
#3411 = CARTESIAN_POINT ( 'NONE',  ( 8.100000001229034297, -2.886751345948129988, 4.999999999999997335 ) ) ;
#3412 = ORIENTED_EDGE ( 'NONE', *, *, #48851, .T. ) ;
#3413 = DIRECTION ( 'NONE',  ( -1.000000000000000000, -0.000000000000000000, -0.000000000000000000 ) ) ;
#3414 = CARTESIAN_POINT ( 'NONE',  ( 8.484601909799253346E-16, 18.76250000000000284, -25.38119784648299770 ) ) ;
#3415 = CARTESIAN_POINT ( 'NONE',  ( 25.42500000122903359, 2.886751345948129099, -4.999999999999998224 ) ) ;
#3416 = CARTESIAN_POINT ( 'NONE',  ( 3.756430356249998770, 15.86562499938548321, 32.16877607737302469 ) ) ;
#3417 = CARTESIAN_POINT ( 'NONE',  ( 6.121875000614517504, -6.054752690667223547, -1.112240025338166033E-15 ) ) ;
#3418 = DIRECTION ( 'NONE',  ( -1.000000000000000000, -0.000000000000000000, -0.000000000000000000 ) ) ;
#3419 = CARTESIAN_POINT ( 'NONE',  ( 14.99062500061451786, -3.027376345333614438, 5.243569643749998122 ) ) ;
#3420 = CARTESIAN_POINT ( 'NONE',  ( 8.709375000614517859, 0.000000000000000000, 5.243569643749999010 ) ) ;
#3421 = CARTESIAN_POINT ( 'NONE',  ( 27.18750000122903288, 6.123233995736764310E-16, -4.999999999999998224 ) ) ;
#3422 = CARTESIAN_POINT ( 'NONE',  ( 17.82187500061451502, -6.054752690667223547, -1.112240025338166033E-15 ) ) ;
#3423 = CARTESIAN_POINT ( 'NONE',  ( 6.046875000614519102, -3.027376345333614438, 5.243569643749998122 ) ) ;
#3424 = CARTESIAN_POINT ( 'NONE',  ( 1.071796769724495668, 17.43259618943233136, -26.00000000000000711 ) ) ;
#3425 = CARTESIAN_POINT ( 'NONE',  ( 6.140625000614516438, -3.027376345333610441, -5.243569643749999898 ) ) ;
#3426 = CARTESIAN_POINT ( 'NONE',  ( 15.40312500061451573, 0.000000000000000000, 5.243569643749999010 ) ) ;
#3427 = VERTEX_POINT ( 'NONE', #8627 ) ;
#3428 = CARTESIAN_POINT ( 'NONE',  ( 12.06562500061451537, 3.027376345333613106, -5.243569643749998122 ) ) ;
#3429 = CARTESIAN_POINT ( 'NONE',  ( 5.925000001229033586, -5.773502691896255534, -1.060575238724906372E-15 ) ) ;
#3430 = CARTESIAN_POINT ( 'NONE',  ( 10.41562500061451679, 3.027376345333611329, 5.243569643749999010 ) ) ;
#3431 = CARTESIAN_POINT ( 'NONE',  ( 20.07187500061451857, -5.492252693125287522, -1.008910452111647106E-15 ) ) ;
#3432 = CARTESIAN_POINT ( 'NONE',  ( 9.787499999999999645, -2.886751345948129988, 4.999999999999997335 ) ) ;
#3433 = PRODUCT_DEFINITION ( 'UNKNOWN', '', #16707, #69118 ) ;
#3434 = CARTESIAN_POINT ( 'NONE',  ( 3.525000001229034119, 2.886751345948126879, 4.999999999999999112 ) ) ;
#3435 = CARTESIAN_POINT ( 'NONE',  ( 17.66249999999999787, 2.886751345948129099, -4.999999999999998224 ) ) ;
#3436 = CARTESIAN_POINT ( 'NONE',  ( 17.78437500061451715, -4.541064518000419881, 2.621784821874995952 ) ) ;
#3437 = CARTESIAN_POINT ( 'NONE',  ( 15.33750000122903323, -4.330127018922194537, 2.499999999999995559 ) ) ;
#3438 = CARTESIAN_POINT ( 'NONE',  ( 22.34999999999999787, 0.000000000000000000, 4.999999999999998224 ) ) ;
#3439 = CARTESIAN_POINT ( 'NONE',  ( 2.121784821875001281, 16.80312500061451786, -26.32496088578401938 ) ) ;
#3440 = CARTESIAN_POINT ( 'NONE',  ( 9.187500000000001776, 5.773502691896255534, 3.535250795749688401E-16 ) ) ;
#3441 = CARTESIAN_POINT ( 'NONE',  ( 2.812500001229033320, -4.330127018922190985, -2.500000000000001332 ) ) ;
#3442 = CARTESIAN_POINT ( 'NONE',  ( 7.347880794884118750E-16, 20.00000000000000000, -24.00000000000000000 ) ) ;
#3443 = CARTESIAN_POINT ( 'NONE',  ( 12.05625000122903145, 0.000000000000000000, 4.999999999999998224 ) ) ;
#3444 = CYLINDRICAL_SURFACE ( 'NONE', #64377, 4.999999999999998224 ) ;
#3445 = CARTESIAN_POINT ( 'NONE',  ( 15.98437500061451821, -4.541064518000419881, 2.621784821874995952 ) ) ;
#3446 = CARTESIAN_POINT ( 'NONE',  ( 29.13749999999999929, -2.886751345948129988, 4.999999999999997335 ) ) ;
#3447 = EDGE_CURVE ( 'NONE', #60259, #55385, #31156, .T. ) ;
#3448 = CARTESIAN_POINT ( 'NONE',  ( 12.40312500061451573, -4.541064518000417216, -2.621784821875001281 ) ) ;
#3449 = CARTESIAN_POINT ( 'NONE',  ( 28.69687500061451502, 4.119189519843966529, -2.378215178124998275 ) ) ;
#3450 = CARTESIAN_POINT ( 'NONE',  ( 22.80937500061451573, -4.541064518000417216, -2.621784821875001281 ) ) ;
#3451 = CARTESIAN_POINT ( 'NONE',  ( 15.30937500061451573, 2.746126346562643317, 4.756430356249998326 ) ) ;
#3452 = CARTESIAN_POINT ( 'NONE',  ( 6.703125000614516438, 4.541064518000418104, -2.621784821874998173 ) ) ;
#3453 = CARTESIAN_POINT ( 'NONE',  ( 12.64687500061451608, 6.054752690667223547, 3.707466751127219781E-16 ) ) ;
#3454 = ORIENTED_EDGE ( 'NONE', *, *, #50099, .T. ) ;
#3455 = CARTESIAN_POINT ( 'NONE',  ( 23.52187500061451786, 3.027376345333611329, 5.243569643749999010 ) ) ;
#3456 = CARTESIAN_POINT ( 'NONE',  ( 27.51562500061451644, 3.027376345333611329, 5.243569643749999010 ) ) ;
#3457 = CARTESIAN_POINT ( 'NONE',  ( 24.78750000000000497, -2.886751345948109559, -5.000000000000028422 ) ) ;
#3458 = CARTESIAN_POINT ( 'NONE',  ( 8.062500000000000000, -5.773502691896255534, -1.060575238724906372E-15 ) ) ;
#3459 = CARTESIAN_POINT ( 'NONE',  ( 15.93750000122903110, 6.123233995736764310E-16, -4.999999999999998224 ) ) ;
#3460 = CARTESIAN_POINT ( 'NONE',  ( -4.000000000000000000, 19.86874999877096570, 30.00000000000000000 ) ) ;
#3461 = CARTESIAN_POINT ( 'NONE',  ( 9.121875000614517504, -4.119189519843968306, 2.378215178124996054 ) ) ;
#3462 = ORIENTED_EDGE ( 'NONE', *, *, #62341, .T. ) ;
#3463 = CARTESIAN_POINT ( 'NONE',  ( 15.07499999999999929, 4.330127018922191873, 2.499999999999999556 ) ) ;
#3464 = CARTESIAN_POINT ( 'NONE',  ( 18.37500000000000355, -4.330127018922194537, 2.499999999999995559 ) ) ;
#3465 = CARTESIAN_POINT ( 'NONE',  ( 14.39062500061451821, 6.054752690667223547, 3.707466751127219781E-16 ) ) ;
#3466 = ORIENTED_EDGE ( 'NONE', *, *, #3037, .T. ) ;
#3467 = CARTESIAN_POINT ( 'NONE',  ( 3.734827092922140768, -3.324314453528163682, -3.734827092927292203 ) ) ;
#3468 = CARTESIAN_POINT ( 'NONE',  ( -2.121784821874999949, 17.53437500061451715, -33.67503911421598417 ) ) ;
#3469 = CARTESIAN_POINT ( 'NONE',  ( 3.815625000614518036, -6.054752690667223547, -1.112240025338166033E-15 ) ) ;
#3470 = CARTESIAN_POINT ( 'NONE',  ( 10.31250000000000178, -5.773502691896255534, -1.060575238724906372E-15 ) ) ;
#3471 = CARTESIAN_POINT ( 'NONE',  ( 10.80000000000000071, -4.330127018922190985, -2.500000000000001332 ) ) ;
#3472 = CARTESIAN_POINT ( 'NONE',  ( 28.24687500061451217, 4.119189519843966529, -2.378215178124998275 ) ) ;
#3473 = ORIENTED_EDGE ( 'NONE', *, *, #55966, .T. ) ;
#3474 = CARTESIAN_POINT ( 'NONE',  ( -2.121784821874999949, 15.67812500061451608, 26.32496088578401938 ) ) ;
#3475 = CARTESIAN_POINT ( 'NONE',  ( 27.21562500061451928, -6.054752690667223547, -1.112240025338166033E-15 ) ) ;
#3476 = CARTESIAN_POINT ( 'NONE',  ( 9.225000000000001421, 4.330127018922191873, 2.499999999999999556 ) ) ;
#3477 =( BOUNDED_SURFACE ( )  B_SPLINE_SURFACE ( 1, 2, ( 
 ( #26135, #30218, #52752, #24666, #48676, #30584, #53110, #44237, #32777, #49047, #66393, #39052, #37947, #43502, #55314, #27239, #4708, #49776, #27605, #26506, #72669, #26879, #43869, #60466, #71940, #15770, #71575, #16497, #44609, #67139, #32409, #72300, #49408, #61212, #38312, #54947, #33136, #22048, #15044, #9513, #5070, #21680, #21316, #20949, #66768, #66027, #16141, #60839, #32046, #10607, #54578, #4352, #9875, #15405, #3982, #10244, #38693, #37582, #60104, #55673, #50138, #25639, #64791, #30813, #53346, #47810, #2744, #69975, #9384, #14182, #37816, #7918, #41900, #70339, #65897, #19345, #14546, #64427, #42268, #53718, #48545, #54452, #19716, #26006, #65156, #31916, #13819, #36359, #25263, #3851, #36716, #59238, #8646, #48177, #31175, #3110, #70701, #2380, #48912, #65528, #37082, #26372, #71443, #58873, #8283, #20818, #54090, #20076, #42632, #71072, #59606, #20447, #9020, #24898, #14914, #52984, #31550, #3488, #42997, #47443, #37456, #59975, #30455, #15277, #43373, #21550, #4942, #44105, #10115, #32645, #27111, #55186, #49280, #61803, #66631, #17096, #60336, #21183, #49644, #45191, #71813, #67008, #43735, #16008, #33007, #27846, #33733, #72171, #5300, #44477, #11206, #66259, #15637, #4581, #56279, #38557, #61080, #10478, #27476, #55546, #50008, #72533, #54813, #28204, #44836, #16369, #5668, #50733, #38178, #60702, #135, #21921, #38924, #67723, #39289, #61443, #4219, #10836, #9745, #33372, #22641, #55908, #50377, #72902, #26747, #22284, #67371, #16734, #32279, #2547, #12538, #18785, #52789, #35788, #58311, #13615, #19148, #63143, #57952, #68340, #35428, #7722, #30256, #7001, #18063, #23977, #7360, #63860, #41350, #46163, #35072, #24704, #69428, #52067, #40624, #30618, #12174 ),
 ( #13250, #1471, #2190, #12895, #29532, #47248, #36160, #58678, #17700, #69781, #29889, #41702, #64226, #8088, #46525, #53148, #45804, #51707, #40261, #69067, #18426, #62782, #34702, #57231, #6646, #1110, #29173, #23617, #52428, #40992, #68703, #57598, #63508, #1834, #24342, #46890, #37257, #59043, #47609, #54615, #53894, #19888, #42441, #42075, #49087, #14354, #13984, #20618, #60506, #9912, #32450, #3652, #65324, #54256, #65695, #9185, #30983, #42802, #54985, #64963, #25441, #26175, #48716, #71238, #31720, #20988, #8447, #15440, #31353, #20250, #36889, #25813, #14715, #53516, #25066, #70139, #19517, #59408, #43176, #3285, #32084, #59779, #8816, #4021, #37984, #64597, #36523, #26546, #15082, #48351, #2910, #37619, #47984, #60141, #70876, #70512, #71615, #9550, #43541, #66062, #55352, #43909, #10645, #39091, #34252, #11735, #49813, #38731, #22089, #61251, #27280, #72338, #44277, #21718, #66432, #5829, #33175, #4391, #26920, #38352, #66808, #62339, #15810, #11009, #60879, #55713, #50178, #44997, #50896, #16180, #22448, #61608, #28360, #10284, #32814, #5108, #296, #27642, #73067, #39825, #49445, #71979, #56080, #44647, #33530, #67534, #5471, #4746, #67177, #21352, #72706, #16538, #28011, #50539, #16897, #39452, #22805, #61973, #67891, #11375, #33894, #56438, #45357, #17263, #17620, #64141, #19064, #41622, #68617, #29808, #12457, #63778, #23895, #17980, #35707, #47167, #69699, #28719, #58229, #52343, #6918, #12095, #1746, #40180, #46807, #29448, #51259, #13166, #661, #40539, #23532, #34616, #23169, #63055, #18338, #13528, #56784, #29090, #34988, #1385, #57517, #6558, #51626, #46082, #1026, #45723, #7634, #51986, #6190, #68258, #62700, #46443, #57146, #68981, #63424, #40911, #12811 ) ),
 .UNSPECIFIED., .F., .F., .F. ) 
 B_SPLINE_SURFACE_WITH_KNOTS ( ( 2, 2 ),
 ( 3, 2, 2, 2, 2, 2, 2, 2, 2, 2, 2, 2, 2, 2, 2, 2, 2, 2, 2, 2, 2, 2, 2, 2, 2, 2, 2, 2, 2, 2, 2, 2, 2, 2, 2, 2, 2, 2, 2, 2, 2, 2, 2, 2, 2, 2, 2, 2, 2, 2, 2, 2, 2, 2, 2, 2, 2, 2, 2, 2, 2, 2, 2, 2, 2, 2, 2, 2, 2, 2, 2, 2, 2, 2, 2, 2, 2, 2, 2, 2, 2, 2, 2, 2, 2, 2, 2, 2, 2, 2, 2, 2, 2, 2, 2, 2, 2, 2, 2, 2, 2, 2, 2, 2, 2, 2, 2, 2, 3 ),
 ( 0.000000000000000000, 1.000000000000000000 ),
 ( 0.000000000000000000, 0.009259259259259258745, 0.01851851851851851749, 0.02777777777777777624, 0.03703703703703703498, 0.04629629629629629373, 0.05555555555555555247, 0.06481481481481481122, 0.07407407407407406996, 0.08333333333333332871, 0.09259259259259258745, 0.1018518518518518462, 0.1111111111111111049, 0.1203703703703703637, 0.1296296296296296224, 0.1388888888888888951, 0.1481481481481481399, 0.1574074074074074125, 0.1666666666666666574, 0.1759259259259259300, 0.1851851851851851749, 0.1944444444444444475, 0.2037037037037036924, 0.2129629629629629650, 0.2222222222222222099, 0.2314814814814814825, 0.2407407407407407274, 0.2500000000000000000, 0.2592592592592592449, 0.2685185185185185452, 0.2777777777777777901, 0.2870370370370370350, 0.2962962962962962798, 0.3055555555555555802, 0.3148148148148148251, 0.3240740740740740700, 0.3333333333333333148, 0.3425925925925926152, 0.3518518518518518601, 0.3611111111111111049, 0.3703703703703703498, 0.3796296296296296502, 0.3888888888888888951, 0.3981481481481481399, 0.4074074074074073848, 0.4166666666666666852, 0.4259259259259259300, 0.4351851851851851749, 0.4444444444444444198, 0.4537037037037037202, 0.4629629629629629650, 0.4722222222222222099, 0.4814814814814814548, 0.4907407407407407551, 0.5000000000000000000, 0.5092592592592593004, 0.5185185185185184897, 0.5277777777777777901, 0.5370370370370370905, 0.5462962962962962798, 0.5555555555555555802, 0.5648148148148147696, 0.5740740740740740700, 0.5833333333333333703, 0.5925925925925925597, 0.6018518518518518601, 0.6111111111111111605, 0.6203703703703703498, 0.6296296296296296502, 0.6388888888888888395, 0.6481481481481481399, 0.6574074074074074403, 0.6666666666666666297, 0.6759259259259259300, 0.6851851851851852304, 0.6944444444444444198, 0.7037037037037037202, 0.7129629629629629095, 0.7222222222222222099, 0.7314814814814815103, 0.7407407407407406996, 0.7500000000000000000, 0.7592592592592593004, 0.7685185185185184897, 0.7777777777777777901, 0.7870370370370370905, 0.7962962962962962798, 0.8055555555555555802, 0.8148148148148147696, 0.8240740740740740700, 0.8333333333333333703, 0.8425925925925925597, 0.8518518518518518601, 0.8611111111111111605, 0.8703703703703703498, 0.8796296296296296502, 0.8888888888888888395, 0.8981481481481481399, 0.9074074074074074403, 0.9166666666666666297, 0.9259259259259259300, 0.9351851851851852304, 0.9444444444444444198, 0.9537037037037037202, 0.9629629629629629095, 0.9722222222222222099, 0.9814814814814815103, 0.9876227234888749207, 0.9974989507237637110 ),
 .UNSPECIFIED. ) 
 GEOMETRIC_REPRESENTATION_ITEM ( )  RATIONAL_B_SPLINE_SURFACE ( (
 ( 1.000000000000000000, 0.8660254037844387076, 1.000000000000000000, 0.8660254037844387076, 1.000000000000000000, 0.8660254037844387076, 1.000000000000000000, 0.8660254037844387076, 1.000000000000000000, 0.8660254037844387076, 1.000000000000000000, 0.8660254037844387076, 1.000000000000000000, 0.8660254037844387076, 1.000000000000000000, 0.8660254037844387076, 1.000000000000000000, 0.8660254037844387076, 1.000000000000000000, 0.8660254037844387076, 1.000000000000000000, 0.8660254037844387076, 1.000000000000000000, 0.8660254037844387076, 1.000000000000000000, 0.8660254037844387076, 1.000000000000000000, 0.8660254037844387076, 1.000000000000000000, 0.8660254037844387076, 1.000000000000000000, 0.8660254037844387076, 1.000000000000000000, 0.8660254037844387076, 1.000000000000000000, 0.8660254037844387076, 1.000000000000000000, 0.8660254037844387076, 1.000000000000000000, 0.8660254037844387076, 1.000000000000000000, 0.8660254037844387076, 1.000000000000000000, 0.8660254037844387076, 1.000000000000000000, 0.8660254037844387076, 1.000000000000000000, 0.8660254037844387076, 1.000000000000000000, 0.8660254037844387076, 1.000000000000000000, 0.8660254037844387076, 1.000000000000000000, 0.8660254037844387076, 1.000000000000000000, 0.8660254037844387076, 1.000000000000000000, 0.8660254037844387076, 1.000000000000000000, 0.8660254037844387076, 1.000000000000000000, 0.8660254037844387076, 1.000000000000000000, 0.8660254037844387076, 1.000000000000000000, 0.8660254037844387076, 1.000000000000000000, 0.8660254037844387076, 1.000000000000000000, 0.8660254037844387076, 1.000000000000000000, 0.8660254037844387076, 1.000000000000000000, 0.8660254037844387076, 1.000000000000000000, 0.8660254037844387076, 1.000000000000000000, 0.8660254037844387076, 1.000000000000000000, 0.8660254037844387076, 1.000000000000000000, 0.8660254037844387076, 1.000000000000000000, 0.8660254037844387076, 1.000000000000000000, 0.8660254037844387076, 1.000000000000000000, 0.8660254037844387076, 1.000000000000000000, 0.8660254037844387076, 1.000000000000000000, 0.8660254037844387076, 1.000000000000000000, 0.8660254037844387076, 1.000000000000000000, 0.8660254037844387076, 1.000000000000000000, 0.8660254037844387076, 1.000000000000000000, 0.8660254037844387076, 1.000000000000000000, 0.8660254037844387076, 1.000000000000000000, 0.8660254037844387076, 1.000000000000000000, 0.8660254037844387076, 1.000000000000000000, 0.8660254037844387076, 1.000000000000000000, 0.8660254037844387076, 1.000000000000000000, 0.8660254037844387076, 1.000000000000000000, 0.8660254037844387076, 1.000000000000000000, 0.8660254037844387076, 1.000000000000000000, 0.8660254037844387076, 1.000000000000000000, 0.8660254037844387076, 1.000000000000000000, 0.8660254037844387076, 1.000000000000000000, 0.8660254037844387076, 1.000000000000000000, 0.8660254037844387076, 1.000000000000000000, 0.8660254037844387076, 1.000000000000000000, 0.8660254037844387076, 1.000000000000000000, 0.8660254037844387076, 1.000000000000000000, 0.8660254037844387076, 1.000000000000000000, 0.8660254037844387076, 1.000000000000000000, 0.8660254037844387076, 1.000000000000000000, 0.8660254037844387076, 1.000000000000000000, 0.8660254037844387076, 1.000000000000000000, 0.8660254037844387076, 1.000000000000000000, 0.8660254037844387076, 1.000000000000000000, 0.8660254037844387076, 1.000000000000000000, 0.8660254037844387076, 1.000000000000000000, 0.8660254037844387076, 1.000000000000000000, 0.8660254037844387076, 1.000000000000000000, 0.8660254037844387076, 1.000000000000000000, 0.8660254037844387076, 1.000000000000000000, 0.8660254037844387076, 1.000000000000000000, 0.8660254037844387076, 1.000000000000000000, 0.8660254037844387076, 1.000000000000000000, 0.8660254037844387076, 1.000000000000000000, 0.8660254037844387076, 1.000000000000000000, 0.8660254037844387076, 1.000000000000000000, 0.8660254037844387076, 1.000000000000000000, 0.8660254037844387076, 1.000000000000000000, 0.8660254037844387076, 1.000000000000000000, 0.8660254037844387076, 1.000000000000000000, 0.8660254037844387076, 1.000000000000000000, 0.8660254037844387076, 1.000000000000000000, 0.8660254037844387076, 1.000000000000000000, 0.8660254037844387076, 1.000000000000000000, 0.8660254037844387076, 1.000000000000000000, 0.8660254037844387076, 1.000000000000000000, 0.8660254037844387076, 1.000000000000000000, 0.8660254037844387076, 1.000000000000000000, 0.8660254037844387076, 1.000000000000000000, 0.8660254037844387076, 1.000000000000000000, 0.8660254037844387076, 1.000000000000000000, 0.8660254037844387076, 1.000000000000000000, 0.8660254037844387076, 1.000000000000000000, 0.8660254037844387076, 1.000000000000000000, 0.8660254037844387076, 1.000000000000000000, 0.8660254037844387076, 1.000000000000000000, 0.8660254037844387076, 1.000000000000000000, 0.9111407948341212482, 0.9401540605060327849, 0.9401540605060327849, 0.9401540605060327849),
 ( 1.000000000000000000, 0.8660254037844387076, 1.000000000000000000, 0.8660254037844387076, 1.000000000000000000, 0.8660254037844387076, 1.000000000000000000, 0.8660254037844387076, 1.000000000000000000, 0.8660254037844387076, 1.000000000000000000, 0.8660254037844387076, 1.000000000000000000, 0.8660254037844387076, 1.000000000000000000, 0.8660254037844387076, 1.000000000000000000, 0.8660254037844387076, 1.000000000000000000, 0.8660254037844387076, 1.000000000000000000, 0.8660254037844387076, 1.000000000000000000, 0.8660254037844387076, 1.000000000000000000, 0.8660254037844387076, 1.000000000000000000, 0.8660254037844387076, 1.000000000000000000, 0.8660254037844387076, 1.000000000000000000, 0.8660254037844387076, 1.000000000000000000, 0.8660254037844387076, 1.000000000000000000, 0.8660254037844387076, 1.000000000000000000, 0.8660254037844387076, 1.000000000000000000, 0.8660254037844387076, 1.000000000000000000, 0.8660254037844387076, 1.000000000000000000, 0.8660254037844387076, 1.000000000000000000, 0.8660254037844387076, 1.000000000000000000, 0.8660254037844387076, 1.000000000000000000, 0.8660254037844387076, 1.000000000000000000, 0.8660254037844387076, 1.000000000000000000, 0.8660254037844387076, 1.000000000000000000, 0.8660254037844387076, 1.000000000000000000, 0.8660254037844387076, 1.000000000000000000, 0.8660254037844387076, 1.000000000000000000, 0.8660254037844387076, 1.000000000000000000, 0.8660254037844387076, 1.000000000000000000, 0.8660254037844387076, 1.000000000000000000, 0.8660254037844387076, 1.000000000000000000, 0.8660254037844387076, 1.000000000000000000, 0.8660254037844387076, 1.000000000000000000, 0.8660254037844387076, 1.000000000000000000, 0.8660254037844387076, 1.000000000000000000, 0.8660254037844387076, 1.000000000000000000, 0.8660254037844387076, 1.000000000000000000, 0.8660254037844387076, 1.000000000000000000, 0.8660254037844387076, 1.000000000000000000, 0.8660254037844387076, 1.000000000000000000, 0.8660254037844387076, 1.000000000000000000, 0.8660254037844387076, 1.000000000000000000, 0.8660254037844387076, 1.000000000000000000, 0.8660254037844387076, 1.000000000000000000, 0.8660254037844387076, 1.000000000000000000, 0.8660254037844387076, 1.000000000000000000, 0.8660254037844387076, 1.000000000000000000, 0.8660254037844387076, 1.000000000000000000, 0.8660254037844387076, 1.000000000000000000, 0.8660254037844387076, 1.000000000000000000, 0.8660254037844387076, 1.000000000000000000, 0.8660254037844387076, 1.000000000000000000, 0.8660254037844387076, 1.000000000000000000, 0.8660254037844387076, 1.000000000000000000, 0.8660254037844387076, 1.000000000000000000, 0.8660254037844387076, 1.000000000000000000, 0.8660254037844387076, 1.000000000000000000, 0.8660254037844387076, 1.000000000000000000, 0.8660254037844387076, 1.000000000000000000, 0.8660254037844387076, 1.000000000000000000, 0.8660254037844387076, 1.000000000000000000, 0.8660254037844387076, 1.000000000000000000, 0.8660254037844387076, 1.000000000000000000, 0.8660254037844387076, 1.000000000000000000, 0.8660254037844387076, 1.000000000000000000, 0.8660254037844387076, 1.000000000000000000, 0.8660254037844387076, 1.000000000000000000, 0.8660254037844387076, 1.000000000000000000, 0.8660254037844387076, 1.000000000000000000, 0.8660254037844387076, 1.000000000000000000, 0.8660254037844387076, 1.000000000000000000, 0.8660254037844387076, 1.000000000000000000, 0.8660254037844387076, 1.000000000000000000, 0.8660254037844387076, 1.000000000000000000, 0.8660254037844387076, 1.000000000000000000, 0.8660254037844387076, 1.000000000000000000, 0.8660254037844387076, 1.000000000000000000, 0.8660254037844387076, 1.000000000000000000, 0.8660254037844387076, 1.000000000000000000, 0.8660254037844387076, 1.000000000000000000, 0.8660254037844387076, 1.000000000000000000, 0.8660254037844387076, 1.000000000000000000, 0.8660254037844387076, 1.000000000000000000, 0.8660254037844387076, 1.000000000000000000, 0.8660254037844387076, 1.000000000000000000, 0.8660254037844387076, 1.000000000000000000, 0.8660254037844387076, 1.000000000000000000, 0.8660254037844387076, 1.000000000000000000, 0.8660254037844387076, 1.000000000000000000, 0.8660254037844387076, 1.000000000000000000, 0.8660254037844387076, 1.000000000000000000, 0.8660254037844387076, 1.000000000000000000, 0.8660254037844387076, 1.000000000000000000, 0.8660254037844387076, 1.000000000000000000, 0.8660254037844387076, 1.000000000000000000, 0.8660254037844387076, 1.000000000000000000, 0.8660254037844387076, 1.000000000000000000, 0.8660254037844387076, 1.000000000000000000, 0.8660254037844387076, 1.000000000000000000, 0.8660254037844387076, 1.000000000000000000, 0.8660254037844387076, 1.000000000000000000, 0.8660254037844387076, 1.000000000000000000, 0.8660254037844387076, 1.000000000000000000, 0.9111407948341212482, 0.9401540605060327849, 0.9401540605060327849, 0.9401540605060327849) ) ) 
 REPRESENTATION_ITEM ( '' )  SURFACE ( )  );
#3478 = CARTESIAN_POINT ( 'NONE',  ( 1.878215178125000495, 19.01562499938548356, 26.74683588394047007 ) ) ;
#3479 = CARTESIAN_POINT ( 'NONE',  ( 23.44687500061451502, 6.054752690667223547, 3.707466751127219781E-16 ) ) ;
#3480 = EDGE_CURVE ( 'NONE', #25370, #59877, #65508, .T. ) ;
#3481 = CARTESIAN_POINT ( 'NONE',  ( 18.62812500061451715, -4.541064518000419881, 2.621784821874995952 ) ) ;
#3482 = CARTESIAN_POINT ( 'NONE',  ( -4.243569643749999898, 13.01562500061459460, -32.45002607614398471 ) ) ;
#3483 = CARTESIAN_POINT ( 'NONE',  ( 23.40000000122903145, -2.886751345948129988, 4.999999999999997335 ) ) ;
#3484 = CARTESIAN_POINT ( 'NONE',  ( 5.053125000614517859, 0.000000000000000000, 5.243569643749999010 ) ) ;
#3485 = CARTESIAN_POINT ( 'NONE',  ( 26.03437500061451715, 5.824947211148865298E-16, -4.756430356249998326 ) ) ;
#3486 = CARTESIAN_POINT ( 'NONE',  ( 21.47812500061451502, 6.421520780324663323E-16, -5.243569643749999010 ) ) ;
#3487 = CARTESIAN_POINT ( 'NONE',  ( 10.50937500061451679, 0.000000000000000000, 4.756430356249998326 ) ) ;
#3488 = CARTESIAN_POINT ( 'NONE',  ( -7.967954043666661671E-16, 17.02812499938548285, 34.33755215474603517 ) ) ;
#3489 = CARTESIAN_POINT ( 'NONE',  ( 16.43437500061451573, -4.541064518000419881, 2.621784821874995952 ) ) ;
#3490 = CARTESIAN_POINT ( 'NONE',  ( 15.83437500061451608, 4.541064518000418104, 2.621784821874999949 ) ) ;
#3491 = CARTESIAN_POINT ( 'NONE',  ( 25.92187500061451999, -6.054752690667223547, -1.112240025338166033E-15 ) ) ;
#3492 = CARTESIAN_POINT ( 'NONE',  ( -4.243569643749999898, 13.55937500061451750, 30.00000000000000000 ) ) ;
#3493 = CARTESIAN_POINT ( 'NONE',  ( 5.128125000614516260, -4.541064518000419881, 2.621784821874995952 ) ) ;
#3494 = CARTESIAN_POINT ( 'NONE',  ( 27.92812500061451431, 4.541064518000418104, 2.621784821874999949 ) ) ;
#3495 = CARTESIAN_POINT ( 'NONE',  ( 28.26562500061451289, 3.027376345333613106, -5.243569643749998122 ) ) ;
#3496 = CARTESIAN_POINT ( 'NONE',  ( 1.071796769724491893, 16.19509619066136707, -26.00000000000000355 ) ) ;
#3497 = CARTESIAN_POINT ( 'NONE',  ( -3.999999999999997335, 19.13750000000000284, 32.30940107675850470 ) ) ;
#3498 = CARTESIAN_POINT ( 'NONE',  ( 6.459375000614518747, 0.000000000000000000, 5.243569643749999010 ) ) ;
#3499 = CARTESIAN_POINT ( 'NONE',  ( 14.51250000122903394, -4.330127018922190985, -2.500000000000001332 ) ) ;
#3500 = CARTESIAN_POINT ( 'NONE',  ( 9.787500001229036073, 4.330127018922191873, 2.499999999999999556 ) ) ;
#3501 = CARTESIAN_POINT ( 'NONE',  ( 5.990625000614517859, -3.027376345333614438, 5.243569643749998122 ) ) ;
#3502 = CARTESIAN_POINT ( 'NONE',  ( -2.000000000000001776, 14.99374999877096570, 33.46410161513775705 ) ) ;
#3503 = CARTESIAN_POINT ( 'NONE',  ( 20.98125000122903216, 4.330127018922191873, 2.499999999999999556 ) ) ;
#3504 = CARTESIAN_POINT ( 'NONE',  ( 13.17187500061451999, 3.027376345333611329, 5.243569643749999010 ) ) ;
#3505 = CYLINDRICAL_SURFACE ( 'NONE', #30219, 3.999999999999996447 ) ;
#3506 = ORIENTED_EDGE ( 'NONE', *, *, #71167, .F. ) ;
#3507 = CARTESIAN_POINT ( 'NONE',  ( 22.34062500061451573, -3.027376345333610441, -5.243569643749999898 ) ) ;
#3508 = CARTESIAN_POINT ( 'NONE',  ( 8.353125000614518569, -4.541064518000417216, -2.621784821875001281 ) ) ;
#3509 = CARTESIAN_POINT ( 'NONE',  ( 25.02187500061451431, -6.054752690667223547, -1.112240025338166033E-15 ) ) ;
#3510 = CARTESIAN_POINT ( 'NONE',  ( 7.903125000614515727, -4.541064518000417216, -2.621784821875001281 ) ) ;
#3511 = CARTESIAN_POINT ( 'NONE',  ( 7.800000001229035362, -2.886751345948125991, -5.000000000000000000 ) ) ;
#3512 = CARTESIAN_POINT ( 'NONE',  ( 21.47812500061451502, 6.421520780324663323E-16, -5.243569643749999010 ) ) ;
#3513 = CARTESIAN_POINT ( 'NONE',  ( -4.243569643749999898, 11.70312500061451644, -30.00000000000000000 ) ) ;
#3514 = CARTESIAN_POINT ( 'NONE',  ( 10.42500000122903536, -5.773502691896255534, -1.060575238724906372E-15 ) ) ;
#3515 = CARTESIAN_POINT ( 'NONE',  ( 19.26562500061451644, 3.027376345333613106, -5.243569643749998122 ) ) ;
#3516 = CARTESIAN_POINT ( 'NONE',  ( 17.50312500061451715, 4.541064518000418104, -2.621784821874998173 ) ) ;
#3517 = CARTESIAN_POINT ( 'NONE',  ( 27.19687500061451857, -2.746126346562646425, 4.756430356249996549 ) ) ;
#3518 = CARTESIAN_POINT ( 'NONE',  ( 17.25000000000000000, 4.330127018922192761, -2.499999999999997780 ) ) ;
#3519 = CARTESIAN_POINT ( 'NONE',  ( 10.83750000122903501, -4.330127018922194537, 2.499999999999995559 ) ) ;
#3520 = CARTESIAN_POINT ( 'NONE',  ( 8.953125000614518214, 4.541064518000418104, -2.621784821874998173 ) ) ;
#3521 = CARTESIAN_POINT ( 'NONE',  ( 12.32812500061451821, -4.541064518000419881, 2.621784821874995952 ) ) ;
#3522 =( BOUNDED_CURVE ( )  B_SPLINE_CURVE ( 3, ( #7335, #47224, #41325, #57571 ),
 .UNSPECIFIED., .F., .F. ) 
 B_SPLINE_CURVE_WITH_KNOTS ( ( 4, 4 ),
 ( 5.521927013012204455, 5.555875059252146642 ),
 .UNSPECIFIED. ) 
 CURVE ( )  GEOMETRIC_REPRESENTATION_ITEM ( )  RATIONAL_B_SPLINE_CURVE ( ( 1.000000000000000000, 0.9999039631522317340, 0.9999039631522317340, 1.000000000000000000 ) ) 
 REPRESENTATION_ITEM ( '' )  );
#3523 = CARTESIAN_POINT ( 'NONE',  ( 23.81250000122903288, 0.000000000000000000, 4.999999999999998224 ) ) ;
#3524 = CARTESIAN_POINT ( 'NONE',  ( 22.62187500061451573, 3.027376345333611329, 5.243569643749999010 ) ) ;
#3525 = CARTESIAN_POINT ( 'NONE',  ( 22.14375000122903359, -2.886751345948153968, -4.999999999999952038 ) ) ;
#3526 = CARTESIAN_POINT ( 'NONE',  ( 4.387500001229033053, 4.330127018922191873, 2.499999999999999556 ) ) ;
#3527 = CARTESIAN_POINT ( 'NONE',  ( 6.159375000614517148, -4.541064518000417216, -2.621784821875001281 ) ) ;
#3528 = CARTESIAN_POINT ( 'NONE',  ( 23.97187500061451360, 3.027376345333611329, 5.243569643749999010 ) ) ;
#3529 = CARTESIAN_POINT ( 'NONE',  ( 4.790750098056429707, -1.432228568557152082, 4.843449711448116979 ) ) ;
#3530 = CARTESIAN_POINT ( 'NONE',  ( 18.32812500061451644, 6.421520780324663323E-16, -5.243569643749999010 ) ) ;
#3531 = CARTESIAN_POINT ( 'NONE',  ( 23.37187500061451573, 3.027376345333613106, -5.243569643749998122 ) ) ;
#3532 = CARTESIAN_POINT ( 'NONE',  ( -3.756430356249999214, 19.69062499938548427, 27.83122392262697176 ) ) ;
#3533 = CARTESIAN_POINT ( 'NONE',  ( -3.999999999999997335, 13.40000000122903323, -27.69059892324149530 ) ) ;
#3534 = CARTESIAN_POINT ( 'NONE',  ( 6.459375000614518747, 0.000000000000000000, 5.243569643749999010 ) ) ;
#3535 = CARTESIAN_POINT ( 'NONE',  ( 18.10312500061451502, 0.000000000000000000, 5.243569643749999010 ) ) ;
#3536 = CARTESIAN_POINT ( 'NONE',  ( 12.45937500061451786, -4.541064518000417216, -2.621784821875001281 ) ) ;
#3537 = ORIENTED_EDGE ( 'NONE', *, *, #17177, .F. ) ;
#3538 = CARTESIAN_POINT ( 'NONE',  ( 22.12500000000000000, 6.123233995736764310E-16, -4.999999999999998224 ) ) ;
#3539 = CARTESIAN_POINT ( 'NONE',  ( 25.30312500061451431, 0.000000000000000000, 5.243569643749999010 ) ) ;
#3540 = CARTESIAN_POINT ( 'NONE',  ( 3.503166010679463760, 3.567662455396273913, -3.772175302801220376 ) ) ;
#3541 = DIRECTION ( 'NONE',  ( -0.000000000000000000, -1.000000000000000000, -0.000000000000000000 ) ) ;
#3542 = CARTESIAN_POINT ( 'NONE',  ( 14.84999999999999964, -4.330127018922190985, -2.500000000000001332 ) ) ;
#3543 = CARTESIAN_POINT ( 'NONE',  ( 23.62500000122902932, 2.886751345948129099, -4.999999999999998224 ) ) ;
#3544 = CARTESIAN_POINT ( 'NONE',  ( 17.42812500061451786, 6.421520780324663323E-16, -5.243569643749999010 ) ) ;
#3545 = ORIENTED_EDGE ( 'NONE', *, *, #37237, .T. ) ;
#3546 = CARTESIAN_POINT ( 'NONE',  ( 22.83749999999999858, -2.886751345948129988, 4.999999999999997335 ) ) ;
#3547 = EDGE_CURVE ( 'NONE', #46020, #17018, #41522, .T. ) ;
#3548 = CARTESIAN_POINT ( 'NONE',  ( 22.69687500061451857, -3.027376345333614438, 5.243569643749998122 ) ) ;
#3549 = ORIENTED_EDGE ( 'NONE', *, *, #50844, .F. ) ;
#3550 = CARTESIAN_POINT ( 'NONE',  ( 11.66249999999999964, -5.773502691896255534, -1.060575238724906372E-15 ) ) ;
#3551 = CARTESIAN_POINT ( 'NONE',  ( 10.97812500061451679, -4.541064518000419881, 2.621784821874995952 ) ) ;
#3552 = CARTESIAN_POINT ( 'NONE',  ( 3.140625000614516882, 6.054752690667223547, 3.707466751127219781E-16 ) ) ;
#3553 = CARTESIAN_POINT ( 'NONE',  ( 16.13437500061451502, 5.492252693125287522, 3.363034840372157021E-16 ) ) ;
#3554 = CARTESIAN_POINT ( 'NONE',  ( 27.40312500061451573, 4.541064518000418104, -2.621784821874998173 ) ) ;
#3555 = CARTESIAN_POINT ( 'NONE',  ( 18.82500000000000284, -4.330127018922194537, 2.499999999999995559 ) ) ;
#3556 = CARTESIAN_POINT ( 'NONE',  ( 26.28749999999999432, 5.773502691896255534, 3.535250795749688894E-16 ) ) ;
#3557 = CARTESIAN_POINT ( 'NONE',  ( 3.046875000614519990, -3.027376345333610441, -5.243569643749999898 ) ) ;
#3558 = CARTESIAN_POINT ( 'NONE',  ( 7.809375000614519280, 0.000000000000000000, 5.243569643749999010 ) ) ;
#3559 = CARTESIAN_POINT ( 'NONE',  ( 17.93437500061451928, 6.421520780324663323E-16, -5.243569643749999010 ) ) ;
#3560 = CYLINDRICAL_SURFACE ( 'NONE', #58366, 9.000000000000000000 ) ;
#3561 = VERTEX_POINT ( 'NONE', #25620 ) ;
#3562 = CARTESIAN_POINT ( 'NONE',  ( 26.39062500061451644, -3.027376345333610441, -5.243569643749999898 ) ) ;
#3563 = CARTESIAN_POINT ( 'NONE',  ( 27.23437500061451644, -4.541064518000419881, 2.621784821874995952 ) ) ;
#3564 = CARTESIAN_POINT ( 'NONE',  ( 16.93125000122903145, 4.330127018922191873, 2.499999999999999556 ) ) ;
#3565 = CARTESIAN_POINT ( 'NONE',  ( 17.25000000000000000, 4.330127018922192761, -2.499999999999997780 ) ) ;
#3566 = CARTESIAN_POINT ( 'NONE',  ( 12.17812500061451608, 4.541064518000418104, 2.621784821874999949 ) ) ;
#3567 = CARTESIAN_POINT ( 'NONE',  ( -4.000000000000000888, 19.51250000000000284, 32.30940107675850470 ) ) ;
#3568 = CARTESIAN_POINT ( 'NONE',  ( 1.626862140677534273E-15, 10.66249999999999964, -26.00000000000000355 ) ) ;
#3569 = CARTESIAN_POINT ( 'NONE',  ( 28.56562500061451715, -6.054752690667223547, -1.112240025338166033E-15 ) ) ;
#3570 = CARTESIAN_POINT ( 'NONE',  ( 19.01250000122903216, -4.330127018922190985, -2.500000000000001332 ) ) ;
#3571 = CARTESIAN_POINT ( 'NONE',  ( 1.626862140677534273E-15, 10.77500000122903323, -26.00000000000000355 ) ) ;
#3572 = CARTESIAN_POINT ( 'NONE',  ( 17.70937500061451431, 0.000000000000000000, 4.756430356249998326 ) ) ;
#3573 = CARTESIAN_POINT ( 'NONE',  ( 5.953125000614519102, 0.000000000000000000, 5.243569643749999010 ) ) ;
#3574 = CARTESIAN_POINT ( 'NONE',  ( 21.87187500061451573, -6.054752690667223547, -1.112240025338166033E-15 ) ) ;
#3575 = CARTESIAN_POINT ( 'NONE',  ( -2.121784821874999949, 17.53437500061451715, 26.32496088578401938 ) ) ;
#3576 = CARTESIAN_POINT ( 'NONE',  ( 23.89687500061451786, 6.054752690667223547, 3.707466751127219781E-16 ) ) ;
#3577 = CARTESIAN_POINT ( 'NONE',  ( 5.437500000000001776, -2.886751345948125991, -5.000000000000000000 ) ) ;
#3578 = CARTESIAN_POINT ( 'NONE',  ( -1.999999999999997113, 9.837500001229035007, 33.46410161513775705 ) ) ;
#3579 = CARTESIAN_POINT ( 'NONE',  ( 12.77812500061451750, -4.541064518000419881, 2.621784821874995952 ) ) ;
#3581 =( BOUNDED_CURVE ( )  B_SPLINE_CURVE ( 2, ( #34857, #63293, #12685, #177, #57743, #7150, #46678 ),
 .UNSPECIFIED., .F., .F. ) 
 B_SPLINE_CURVE_WITH_KNOTS ( ( 3, 2, 2, 3 ),
 ( 0.8666666666666666963, 0.8694444444444444642, 0.8722222222222222321, 0.8750000000000000000 ),
 .UNSPECIFIED. ) 
 CURVE ( )  GEOMETRIC_REPRESENTATION_ITEM ( )  RATIONAL_B_SPLINE_CURVE ( ( 1.000000000000000000, 0.8660254037844387076, 1.000000000000000000, 0.8660254037844387076, 1.000000000000000000, 0.8660254037844387076, 1.000000000000000000 ) ) 
 REPRESENTATION_ITEM ( '' )  );
#3580 = CARTESIAN_POINT ( 'NONE',  ( 3.825000001229032609, 2.886751345948129099, -4.999999999999998224 ) ) ;
#3582 = CARTESIAN_POINT ( 'NONE',  ( 8.859375000614518214, -4.541064518000417216, -2.621784821875001281 ) ) ;
#3583 = FACE_OUTER_BOUND ( 'NONE', #19784, .T. ) ;
#3584 = CARTESIAN_POINT ( 'NONE',  ( 9.665625000614515017, -6.054752690667223547, -1.112240025338166033E-15 ) ) ;
#3585 = CARTESIAN_POINT ( 'NONE',  ( 14.10937500061451644, 0.000000000000000000, 5.243569643749999010 ) ) ;
#3586 = CARTESIAN_POINT ( 'NONE',  ( 30.00000000000000000, 0.000000000000000000, 0.000000000000000000 ) ) ;
#3587 = CARTESIAN_POINT ( 'NONE',  ( 22.23750000122903003, 6.123233995736764310E-16, -4.999999999999998224 ) ) ;
#3588 = CARTESIAN_POINT ( 'NONE',  ( 11.03437500061451715, -4.541064518000419881, 2.621784821874995952 ) ) ;
#3589 = CARTESIAN_POINT ( 'NONE',  ( 12.36562500061451608, -6.054752690667223547, -1.112240025338166033E-15 ) ) ;
#3590 = CARTESIAN_POINT ( 'NONE',  ( 28.36875000122903145, -5.773502691896255534, -1.060575238724906372E-15 ) ) ;
#3591 = CARTESIAN_POINT ( 'NONE',  ( 22.05937500061451573, 4.541064518000418104, -2.621784821874998173 ) ) ;
#3592 = CARTESIAN_POINT ( 'NONE',  ( 45.00000000000000000, 0.000000000000000000, 4.999999999999998224 ) ) ;
#3593 = CARTESIAN_POINT ( 'NONE',  ( -1.071796769724491005, 11.92009619066136850, -34.00000000000000000 ) ) ;
#3594 = CARTESIAN_POINT ( 'NONE',  ( 3.144856541311010556, 3.887142566792906706, -3.519253510942787599 ) ) ;
#3595 = CARTESIAN_POINT ( 'NONE',  ( 2.121784821875001281, 14.60937500061451821, -26.32496088578401938 ) ) ;
#3596 = CARTESIAN_POINT ( 'NONE',  ( 15.71250000122903501, 0.000000000000000000, 4.999999999999998224 ) ) ;
#3597 = CARTESIAN_POINT ( 'NONE',  ( 10.73437500061451644, 6.421520780324663323E-16, -5.243569643749999010 ) ) ;
#3598 = CARTESIAN_POINT ( 'NONE',  ( -4.243569643749999898, 16.65312500061451573, -30.00000000000000000 ) ) ;
#3599 = CARTESIAN_POINT ( 'NONE',  ( 17.73750000122903359, 6.123233995736764310E-16, -4.999999999999998224 ) ) ;
#3600 = CARTESIAN_POINT ( 'NONE',  ( 13.71562500061451750, -6.054752690667223547, -1.112240025338166033E-15 ) ) ;
#3601 = VERTEX_POINT ( 'NONE', #24880 ) ;
#3602 = CARTESIAN_POINT ( 'NONE',  ( 15.45000000000000107, 4.330127018922192761, -2.499999999999997780 ) ) ;
#3603 = CARTESIAN_POINT ( 'NONE',  ( 5.137500001229033941, 6.123233995736764310E-16, -4.999999999999998224 ) ) ;
#3604 = CARTESIAN_POINT ( 'NONE',  ( 10.47187500061451715, 3.027376345333611329, 5.243569643749999010 ) ) ;
#3605 = EDGE_CURVE ( 'NONE', #41592, #18509, #2726, .T. ) ;
#3606 = CARTESIAN_POINT ( 'NONE',  ( 9.487500001229033586, -4.330127018922194537, 2.499999999999995559 ) ) ;
#3607 = CARTESIAN_POINT ( 'NONE',  ( 18.86250000122903359, 0.000000000000000000, 4.999999999999998224 ) ) ;
#3608 = EDGE_CURVE ( 'NONE', #41920, #28631, #11780, .T. ) ;
#3609 = CARTESIAN_POINT ( 'NONE',  ( 16.67812500061451786, 4.541064518000418104, 2.621784821874999949 ) ) ;
#3610 = CARTESIAN_POINT ( 'NONE',  ( 19.82812500061451644, 4.541064518000418104, 2.621784821874999949 ) ) ;
#3611 = CARTESIAN_POINT ( 'NONE',  ( 28.53750000122903074, 6.123233995736764310E-16, -4.999999999999998224 ) ) ;
#3612 = CARTESIAN_POINT ( 'NONE',  ( 4.078125000614517326, 4.541064518000418104, 2.621784821874999949 ) ) ;
#3613 = CARTESIAN_POINT ( 'NONE',  ( 25.72499999999999787, 6.123233995736764310E-16, -4.999999999999998224 ) ) ;
#3614 = CARTESIAN_POINT ( 'NONE',  ( 25.05000000000000071, 0.000000000000000000, 4.999999999999998224 ) ) ;
#3615 = CARTESIAN_POINT ( 'NONE',  ( 29.62500000000000000, -4.330127018922194537, 2.499999999999995559 ) ) ;
#3616 = CARTESIAN_POINT ( 'NONE',  ( 27.83437500061451786, 6.421520780324663323E-16, -5.243569643749999010 ) ) ;
#3617 = CARTESIAN_POINT ( 'NONE',  ( 1.626862140677534273E-15, 12.46250000000000213, -26.00000000000000355 ) ) ;
#3618 = CARTESIAN_POINT ( 'NONE',  ( 12.00000000122903465, 5.773502691896255534, 3.535250795749688894E-16 ) ) ;
#3619 = CARTESIAN_POINT ( 'NONE',  ( 4.687500000000000000, 5.773502691896255534, 3.535250795749688894E-16 ) ) ;
#3620 = CARTESIAN_POINT ( 'NONE',  ( 21.67500000000000071, 6.123233995736764310E-16, -4.999999999999998224 ) ) ;
#3621 = CARTESIAN_POINT ( 'NONE',  ( 6.871875000614517504, 3.027376345333611329, 5.243569643749999010 ) ) ;
#3622 = CARTESIAN_POINT ( 'NONE',  ( 26.72812500061451502, -4.541064518000419881, 2.621784821874995952 ) ) ;
#3623 = CARTESIAN_POINT ( 'NONE',  ( 4.710420932447848763, -3.574158126769929833, 4.296515817649278368 ) ) ;
#3624 = CARTESIAN_POINT ( 'NONE',  ( -0.2030170140429786718, 10.00000000000000000, -23.99999999999999289 ) ) ;
#3625 = DIRECTION ( 'NONE',  ( -1.000000000000000000, -0.000000000000000000, -0.000000000000000000 ) ) ;
#3626 = CARTESIAN_POINT ( 'NONE',  ( 4.321875000614517681, -6.054752690667223547, -1.112240025338166033E-15 ) ) ;
#3627 = CARTESIAN_POINT ( 'NONE',  ( 9.309375000614517504, -4.541064518000417216, -2.621784821875001281 ) ) ;
#3628 = CARTESIAN_POINT ( 'NONE',  ( 3.037500000000002309, -2.886751345948129988, 4.999999999999997335 ) ) ;
#3629 = CARTESIAN_POINT ( 'NONE',  ( 9.001249775931846008E-16, 12.26562500061459282, 34.90005215228797653 ) ) ;
#3630 = CARTESIAN_POINT ( 'NONE',  ( 21.56250000000000000, -5.773502691896255534, -1.060575238724906372E-15 ) ) ;
#3631 = CARTESIAN_POINT ( 'NONE',  ( 1.626862140677534273E-15, 17.86250000000000071, -26.00000000000000355 ) ) ;
#3632 = CARTESIAN_POINT ( 'NONE',  ( 3.374999999999999556, 4.330127018922191873, 2.499999999999999556 ) ) ;
#3633 = CARTESIAN_POINT ( 'NONE',  ( 12.00937500061451502, 2.746126346562645981, -4.756430356249997438 ) ) ;
#3634 = ORIENTED_EDGE ( 'NONE', *, *, #56957, .F. ) ;
#3635 = CARTESIAN_POINT ( 'NONE',  ( 21.29062500061451502, -3.027376345333614438, 5.243569643749998122 ) ) ;
#3636 = CARTESIAN_POINT ( 'NONE',  ( 9.703125000614514661, -4.541064518000417216, -2.621784821875001281 ) ) ;
#3637 = CARTESIAN_POINT ( 'NONE',  ( 24.68437500061451573, 5.492252693125287522, 3.363034840372157021E-16 ) ) ;
#3638 = CARTESIAN_POINT ( 'NONE',  ( 6.721875000614518925, 3.027376345333613106, -5.243569643749998122 ) ) ;
#3639 = CARTESIAN_POINT ( 'NONE',  ( 24.67500000000000071, -4.330127018922194537, 2.499999999999995559 ) ) ;
#3640 = CARTESIAN_POINT ( 'NONE',  ( 21.15000000122903145, -2.886751345948129988, 4.999999999999997335 ) ) ;
#3641 = CARTESIAN_POINT ( 'NONE',  ( 28.04062500061451502, -3.027376345333614438, 5.243569643749998122 ) ) ;
#3642 = CARTESIAN_POINT ( 'NONE',  ( 1.626862140677534273E-15, 15.61250000000000071, 34.00000000000000000 ) ) ;
#3643 = CARTESIAN_POINT ( 'NONE',  ( 10.09687500061451715, -3.027376345333614438, 5.243569643749998122 ) ) ;
#3644 = CARTESIAN_POINT ( 'NONE',  ( 13.65937500061451715, 0.000000000000000000, 5.243569643749999010 ) ) ;
#3645 = CARTESIAN_POINT ( 'NONE',  ( 24.12187500061451217, -6.054752690667223547, -1.112240025338166033E-15 ) ) ;
#3646 = CARTESIAN_POINT ( 'NONE',  ( 4.000000000000000000, 18.05000000122903359, -27.69059892324149885 ) ) ;
#3647 = CARTESIAN_POINT ( 'NONE',  ( 12.86250000000000071, 2.886751345948126879, 4.999999999999999112 ) ) ;
#3648 = CARTESIAN_POINT ( 'NONE',  ( 18.75937500061451857, -4.541064518000417216, -2.621784821875001281 ) ) ;
#3649 = CARTESIAN_POINT ( 'NONE',  ( 10.05937500061451750, 0.000000000000000000, 5.243569643749999010 ) ) ;
#3650 = CARTESIAN_POINT ( 'NONE',  ( -1.878215178124999163, 20.55312499938548143, 26.74683588394047007 ) ) ;
#3651 = CARTESIAN_POINT ( 'NONE',  ( 24.00000000000000000, 4.330127018922192761, -2.499999999999997780 ) ) ;
#3652 = CARTESIAN_POINT ( 'NONE',  ( 2.828200636599751609E-16, 14.41249999999999964, 25.38119784648299415 ) ) ;
#3653 = CARTESIAN_POINT ( 'NONE',  ( -3.999999999999999112, 9.762500001229033941, -30.00000000000000000 ) ) ;
#3654 = CARTESIAN_POINT ( 'NONE',  ( 25.62187500061451573, 2.746126346562645981, -4.756430356249997438 ) ) ;
#3655 = CARTESIAN_POINT ( 'NONE',  ( 12.85312500061451502, -4.541064518000417216, -2.621784821875001281 ) ) ;
#3656 = CARTESIAN_POINT ( 'NONE',  ( 29.22187500061451715, 3.027376345333613106, -5.243569643749998122 ) ) ;
#3657 = LINE ( 'NONE', #37989, #39618 ) ;
#3658 = FACE_OUTER_BOUND ( 'NONE', #546, .T. ) ;
#3659 = CARTESIAN_POINT ( 'NONE',  ( 11.36250000000000071, 2.886751345948129099, -4.999999999999998224 ) ) ;
#3660 = CARTESIAN_POINT ( 'NONE',  ( 4.000000000000000000, 18.95000000122903216, 32.30940107675849049 ) ) ;
#3661 = CARTESIAN_POINT ( 'NONE',  ( 10.38750000122903572, -4.330127018922194537, 2.499999999999995559 ) ) ;
#3662 = CARTESIAN_POINT ( 'NONE',  ( 21.64687500061451786, 6.054752690667223547, 3.707466751127219781E-16 ) ) ;
#3663 = CARTESIAN_POINT ( 'NONE',  ( 17.22187500061451715, 3.027376345333611329, 5.243569643749999010 ) ) ;
#3664 = LINE ( 'NONE', #65337, #44264 ) ;
#3665 = ORIENTED_EDGE ( 'NONE', *, *, #40237, .F. ) ;
#3666 = CARTESIAN_POINT ( 'NONE',  ( 17.12812500061451715, 4.541064518000418104, 2.621784821874999949 ) ) ;
#3667 = CARTESIAN_POINT ( 'NONE',  ( 28.57500000122903572, 2.886751345948129099, -4.999999999999998224 ) ) ;
#3668 = CARTESIAN_POINT ( 'NONE',  ( 18.00937500061451502, 4.541064518000418104, -2.621784821874998173 ) ) ;
#3669 = CARTESIAN_POINT ( 'NONE',  ( 28.77187500061451431, 3.027376345333613106, -5.243569643749998122 ) ) ;
#3670 = CARTESIAN_POINT ( 'NONE',  ( 5.015625000614518214, 3.027376345333611329, 5.243569643749999010 ) ) ;
#3671 = CARTESIAN_POINT ( 'NONE',  ( 18.47812500061451857, 4.541064518000418104, 2.621784821874999949 ) ) ;
#3672 = CARTESIAN_POINT ( 'NONE',  ( 28.02187500061451431, 3.027376345333611329, 5.243569643749999010 ) ) ;
#3673 = CARTESIAN_POINT ( 'NONE',  ( 4.243569643749999898, 11.92812500061451608, 30.00000000000000000 ) ) ;
#3674 = CARTESIAN_POINT ( 'NONE',  ( 17.25000000122903288, -2.886751345948125991, -5.000000000000000000 ) ) ;
#3675 = CARTESIAN_POINT ( 'NONE',  ( 9.046875000614518214, 5.492252693125287522, 3.363034840372157021E-16 ) ) ;
#3676 = CARTESIAN_POINT ( 'NONE',  ( 7.865625000614516082, -6.054752690667223547, -1.112240025338166033E-15 ) ) ;
#3677 = CARTESIAN_POINT ( 'NONE',  ( 25.82812500061451644, -4.541064518000419881, 2.621784821874995952 ) ) ;
#3678 = CARTESIAN_POINT ( 'NONE',  ( 1.999999999999998668, 19.06250000122903288, -33.46410161513775705 ) ) ;
#3679 = CARTESIAN_POINT ( 'NONE',  ( 22.17187500061451644, 3.027376345333611329, 5.243569643749999010 ) ) ;
#3680 = CARTESIAN_POINT ( 'NONE',  ( 13.19062500061451537, -3.027376345333614438, 5.243569643749998122 ) ) ;
#3681 = CARTESIAN_POINT ( 'NONE',  ( 23.25000000122903288, 5.773502691896255534, 3.535250795749688894E-16 ) ) ;
#3682 = CARTESIAN_POINT ( 'NONE',  ( 22.30312500061451431, -4.541064518000417216, -2.621784821875001281 ) ) ;
#3683 = CARTESIAN_POINT ( 'NONE',  ( 17.29687500061451999, -3.027376345333614438, 5.243569643749998122 ) ) ;
#3684 = CARTESIAN_POINT ( 'NONE',  ( 13.00312500061451537, 4.541064518000418104, -2.621784821874998173 ) ) ;
#3685 = CARTESIAN_POINT ( 'NONE',  ( 2.121784821875001281, 14.60937500061451821, 33.67503911421598417 ) ) ;
#3686 = CARTESIAN_POINT ( 'NONE',  ( 18.81562500061452070, 3.027376345333613106, -5.243569643749998122 ) ) ;
#3687 = CARTESIAN_POINT ( 'NONE',  ( 10.20000000000000107, 0.000000000000000000, 4.999999999999998224 ) ) ;
#3688 = ORIENTED_EDGE ( 'NONE', *, *, #34392, .T. ) ;
#3689 = CARTESIAN_POINT ( 'NONE',  ( 23.36250000000000071, -5.773502691896255534, -1.060575238724906372E-15 ) ) ;
#3690 = CARTESIAN_POINT ( 'NONE',  ( -4.243569643749997233, 18.54687500061451289, -27.54997392385601174 ) ) ;
#3691 = CARTESIAN_POINT ( 'NONE',  ( 0.9778744620075204841, -4.999999999999998224, 0.9778744620075204841 ) ) ;
#3692 = CARTESIAN_POINT ( 'NONE',  ( 26.31562500061451715, -6.054752690667223547, -1.112240025338166033E-15 ) ) ;
#3693 = CARTESIAN_POINT ( 'NONE',  ( 4.565625000614516260, 3.027376345333611329, 5.243569643749999010 ) ) ;
#3694 = CARTESIAN_POINT ( 'NONE',  ( 19.31250000122903288, 0.000000000000000000, 4.999999999999998224 ) ) ;
#3695 = CARTESIAN_POINT ( 'NONE',  ( 24.25312500061451715, 4.541064518000418104, -2.621784821874998173 ) ) ;
#3696 = CARTESIAN_POINT ( 'NONE',  ( 23.55000000000000071, 4.330127018922192761, -2.499999999999997780 ) ) ;
#3697 = CARTESIAN_POINT ( 'NONE',  ( 27.55312500061451786, 0.000000000000000000, 5.243569643749999010 ) ) ;
#3698 = CARTESIAN_POINT ( 'NONE',  ( 7.640625000614517326, 6.054752690667223547, 3.707466751127219781E-16 ) ) ;
#3699 = ORIENTED_EDGE ( 'NONE', *, *, #55011, .T. ) ;
#3700 = CARTESIAN_POINT ( 'NONE',  ( 24.14062500061451289, -3.027376345333610441, -5.243569643749999898 ) ) ;
#3701 = CARTESIAN_POINT ( 'NONE',  ( 5.615625000614517859, -6.054752690667223547, -1.112240025338166033E-15 ) ) ;
#3702 = CARTESIAN_POINT ( 'NONE',  ( 13.17187500061451999, 2.746126346562643317, 4.756430356249998326 ) ) ;
#3703 = CARTESIAN_POINT ( 'NONE',  ( 3.778125000614519280, -4.541064518000419881, 2.621784821874995952 ) ) ;
#3704 = CARTESIAN_POINT ( 'NONE',  ( 3.999999999999998668, 13.17500000122903359, -32.30940107675850470 ) ) ;
#3705 = CARTESIAN_POINT ( 'NONE',  ( -1.071796769724488563, 10.64240381056766616, -26.00000000000000000 ) ) ;
#3706 = STYLED_ITEM ( 'NONE', ( #8294 ), #10934 ) ;
#3707 = CARTESIAN_POINT ( 'NONE',  ( 9.862500000000000711, -5.773502691896255534, -1.060575238724906372E-15 ) ) ;
#3708 = CARTESIAN_POINT ( 'NONE',  ( 12.45937500061451786, -4.541064518000417216, -2.621784821875001281 ) ) ;
#3709 = CARTESIAN_POINT ( 'NONE',  ( 5.775000001229033231, 2.886751345948126879, 4.999999999999999112 ) ) ;
#3710 = CARTESIAN_POINT ( 'NONE',  ( 13.65937500061451715, 0.000000000000000000, 5.243569643749999010 ) ) ;
#3711 = CARTESIAN_POINT ( 'NONE',  ( 15.48749999999999893, 5.773502691896255534, 3.535250795749688894E-16 ) ) ;
#3712 = CARTESIAN_POINT ( 'NONE',  ( 5.484375000614518214, 4.541064518000418104, 2.621784821874999949 ) ) ;
#3713 = CARTESIAN_POINT ( 'NONE',  ( 21.28125000122903288, 6.123233995736764310E-16, -4.999999999999998224 ) ) ;
#3714 = CARTESIAN_POINT ( 'NONE',  ( 20.96250000122903145, 4.330127018922192761, -2.499999999999997780 ) ) ;
#3715 = CARTESIAN_POINT ( 'NONE',  ( 11.55937500061451928, -4.541064518000417216, -2.621784821875001281 ) ) ;
#3716 = CARTESIAN_POINT ( 'NONE',  ( 0.000000000000000000, 20.00000000000000000, -30.00000000000000000 ) ) ;
#3717 = CARTESIAN_POINT ( 'NONE',  ( 21.32812500061451644, -4.541064518000419881, 2.621784821874995952 ) ) ;
#3718 = CARTESIAN_POINT ( 'NONE',  ( 2.121784821875001281, 10.55937500061451750, 33.67503911421598417 ) ) ;
#3719 = CARTESIAN_POINT ( 'NONE',  ( 2.121784821875001281, 19.50312500061459531, 33.67503911421598417 ) ) ;
#3720 = CARTESIAN_POINT ( 'NONE',  ( 26.85937500061451644, -4.541064518000417216, -2.621784821875001281 ) ) ;
#3721 =( BOUNDED_CURVE ( )  B_SPLINE_CURVE ( 2, ( #30837, #3137, #48203, #47108, #69640, #70365, #2402 ),
 .UNSPECIFIED., .F., .F. ) 
 B_SPLINE_CURVE_WITH_KNOTS ( ( 3, 2, 2, 3 ),
 ( 0.9687606754894464434, 0.9694444444444444420, 0.9722222222222222099, 0.9728271748341141834 ),
 .UNSPECIFIED. ) 
 CURVE ( )  GEOMETRIC_REPRESENTATION_ITEM ( )  RATIONAL_B_SPLINE_CURVE ( ( 0.9502783720093003206, 0.9670212389257863972, 1.000000000000000000, 0.8660254037844387076, 1.000000000000000000, 0.9708226185132003971, 0.9543539088861985320 ) ) 
 REPRESENTATION_ITEM ( '' )  );
#3722 = CARTESIAN_POINT ( 'NONE',  ( -2.556497649636125342E-15, 19.21250000000000213, 34.00000000000000000 ) ) ;
#3723 = EDGE_CURVE ( 'NONE', #27538, #329, #64188, .T. ) ;
#3724 = CARTESIAN_POINT ( 'NONE',  ( 3.740625000614516527, -3.027376345333614438, 5.243569643749998122 ) ) ;
#3725 = CARTESIAN_POINT ( 'NONE',  ( 23.37187500061451573, 4.119189519843966529, 2.378215178124999607 ) ) ;
#3726 = CARTESIAN_POINT ( 'NONE',  ( 13.24687500061451750, -3.027376345333614438, 5.243569643749998122 ) ) ;
#3727 = CARTESIAN_POINT ( 'NONE',  ( 7.312500001229033764, -4.330127018922190985, -2.500000000000001332 ) ) ;
#3728 = CARTESIAN_POINT ( 'NONE',  ( 26.28750000122903430, 6.123233995736764310E-16, -4.999999999999998224 ) ) ;
#3729 = CARTESIAN_POINT ( 'NONE',  ( 4.884375000614518569, 6.421520780324663323E-16, -5.243569643749999010 ) ) ;
#3730 = CARTESIAN_POINT ( 'NONE',  ( 16.84687500061451715, -3.027376345333614438, 5.243569643749998122 ) ) ;
#3731 = PLANE ( 'NONE',  #70149 ) ;
#3732 = CARTESIAN_POINT ( 'NONE',  ( 23.92499999999999716, 6.123233995736764310E-16, -4.999999999999998224 ) ) ;
#3733 = CARTESIAN_POINT ( 'NONE',  ( 2.737500001229034474, -4.330127018922194537, 2.499999999999995559 ) ) ;
#3734 = CARTESIAN_POINT ( 'NONE',  ( 25.99687500061451928, -3.027376345333610441, -5.243569643749999898 ) ) ;
#3735 = CARTESIAN_POINT ( 'NONE',  ( 3.756430356250000102, 13.20312499938548356, 30.00000000000000000 ) ) ;
#3736 = DIRECTION ( 'NONE',  ( -1.000000000000000000, -0.000000000000000000, -0.000000000000000000 ) ) ;
#3737 = CARTESIAN_POINT ( 'NONE',  ( 9.112500000000000711, 2.886751345948129099, -4.999999999999998224 ) ) ;
#3738 = CARTESIAN_POINT ( 'NONE',  ( 10.13437500061451502, -2.746126346562642428, -4.756430356249999214 ) ) ;
#3739 = CARTESIAN_POINT ( 'NONE',  ( 19.00312500061451715, 0.000000000000000000, 5.243569643749999010 ) ) ;
#3740 = CARTESIAN_POINT ( 'NONE',  ( 11.06250000000000000, 2.886751345948126879, 4.999999999999999112 ) ) ;
#3741 = CARTESIAN_POINT ( 'NONE',  ( 3.665625000614517681, 3.027376345333611329, 5.243569643749999010 ) ) ;
#3742 = CARTESIAN_POINT ( 'NONE',  ( 18.82500000000000284, -4.330127018922194537, 2.499999999999995559 ) ) ;
#3743 = CARTESIAN_POINT ( 'NONE',  ( 17.69062500061451715, -3.027376345333614438, 5.243569643749998122 ) ) ;
#3744 = CARTESIAN_POINT ( 'NONE',  ( -1.071796769724491005, 18.67009619066136494, 26.00000000000000355 ) ) ;
#3745 = CARTESIAN_POINT ( 'NONE',  ( 23.40000000122903145, -2.886751345948129988, 4.999999999999997335 ) ) ;
#3746 = CARTESIAN_POINT ( 'NONE',  ( -7.967954043666661671E-16, 19.72812499938547859, 34.33755215474603517 ) ) ;
#3747 = B_SPLINE_CURVE_WITH_KNOTS ( 'NONE', 3,
 ( #19091, #62189, #65635, #60446, #66005, #37560, #48655, #49024, #71179, #32384, #9855, #48290, #20928, #54923, #60082, #4332, #26856, #21294, #3960, #49388, #70814, #26483, #71554, #43481, #37927, #10223, #15385, #71919, #20189, #54196, #72280, #43109, #43846, #66373, #15749, #38288, #55294, #31662, #20552, #60815 ),
 .UNSPECIFIED., .F., .F.,
 ( 4, 2, 2, 2, 2, 2, 2, 2, 2, 2, 2, 2, 2, 2, 2, 2, 2, 2, 2, 4 ),
 ( 0.02627519828802195659, 0.02668902850172998054, 0.02710285871543800795, 0.02793051914285405585, 0.02958583999768615858, 0.03041350042510220647, 0.03124116085251825090, 0.03206882127993430226, 0.03248265149364232274, 0.03289648170735034322, 0.03331031192105837063, 0.03372414213476639111, 0.03455180256218243207, 0.03537946298959846608, 0.03620712341701450704, 0.03703478384443054106, 0.03786244427184658201, 0.03869010469926261603, 0.03910393491297063651, 0.03951776512667865005 ),
 .UNSPECIFIED. ) ;
#3748 = CARTESIAN_POINT ( 'NONE',  ( 29.48437500061451644, -4.541064518000419881, 2.621784821874995952 ) ) ;
#3749 = VERTEX_POINT ( 'NONE', #66613 ) ;
#3750 = CARTESIAN_POINT ( 'NONE',  ( 18.62812500061451715, -4.541064518000419881, 2.621784821874995952 ) ) ;
#3751 = CARTESIAN_POINT ( 'NONE',  ( 23.76562500061451644, 3.027376345333613106, -5.243569643749998122 ) ) ;
#3752 = CARTESIAN_POINT ( 'NONE',  ( 24.90937500061451715, 0.000000000000000000, 5.243569643749999010 ) ) ;
#3753 = CARTESIAN_POINT ( 'NONE',  ( 9.074999999999999289, 6.123233995736764310E-16, -4.999999999999998224 ) ) ;
#3754 = CARTESIAN_POINT ( 'NONE',  ( 11.16562500061451679, 3.027376345333613106, -5.243569643749998122 ) ) ;
#3755 = CARTESIAN_POINT ( 'NONE',  ( 26.61562500061451786, 3.027376345333611329, 5.243569643749999010 ) ) ;
#3756 = CARTESIAN_POINT ( 'NONE',  ( 17.44687500061451857, -3.027376345333610441, -5.243569643749999898 ) ) ;
#3757 = CARTESIAN_POINT ( 'NONE',  ( 7.940625000614518036, -3.027376345333610441, -5.243569643749999898 ) ) ;
#3758 = CARTESIAN_POINT ( 'NONE',  ( 0.000000000000000000, 20.00000000000000000, -30.00000000000000000 ) ) ;
#3759 = CARTESIAN_POINT ( 'NONE',  ( -4.243569643749999898, 9.959375000614517859, 30.00000000000000000 ) ) ;
#3760 = CARTESIAN_POINT ( 'NONE',  ( 22.98750000122903003, -4.330127018922194537, 2.499999999999995559 ) ) ;
#3761 = CARTESIAN_POINT ( 'NONE',  ( 16.58437500061451786, 5.824947211148865298E-16, -4.756430356249998326 ) ) ;
#3762 = CARTESIAN_POINT ( 'NONE',  ( 15.10312500061451502, -4.541064518000417216, -2.621784821875001281 ) ) ;
#3763 = CARTESIAN_POINT ( 'NONE',  ( 8.671875000614518214, 3.027376345333611329, 5.243569643749999010 ) ) ;
#3764 = CARTESIAN_POINT ( 'NONE',  ( 6.534375000614517148, -4.541064518000419881, 2.621784821874995952 ) ) ;
#3765 = ORIENTED_EDGE ( 'NONE', *, *, #66921, .T. ) ;
#3766 = CARTESIAN_POINT ( 'NONE',  ( 29.18437500061451573, 6.421520780324663323E-16, -5.243569643749999010 ) ) ;
#3767 = CARTESIAN_POINT ( 'NONE',  ( 21.89062500061451289, -3.027376345333610441, -5.243569643749999898 ) ) ;
#3768 = CARTESIAN_POINT ( 'NONE',  ( 17.29687500061451999, -3.027376345333614438, 5.243569643749998122 ) ) ;
#3769 = CARTESIAN_POINT ( 'NONE',  ( 20.50312500061451715, -4.541064518000417216, -2.621784821875001281 ) ) ;
#3770 = CARTESIAN_POINT ( 'NONE',  ( -3.999999999999999556, 11.86250000000000071, 27.69059892324149530 ) ) ;
#3771 = CARTESIAN_POINT ( 'NONE',  ( 27.14062500061451644, -3.027376345333614438, 5.243569643749998122 ) ) ;
#3772 = CARTESIAN_POINT ( 'NONE',  ( 5.925000001229033586, -5.773502691896255534, -1.060575238724906372E-15 ) ) ;
#3773 = ORIENTED_EDGE ( 'NONE', *, *, #43418, .F. ) ;
#3774 = CARTESIAN_POINT ( 'NONE',  ( 3.375000001229033320, 2.886751345948129099, -4.999999999999998224 ) ) ;
#3775 = CARTESIAN_POINT ( 'NONE',  ( -2.828200636599751609E-16, 17.63749999999999929, -34.61880215351700230 ) ) ;
#3776 = CARTESIAN_POINT ( 'NONE',  ( 25.46250000122903501, 4.330127018922192761, -2.499999999999997780 ) ) ;
#3777 = CARTESIAN_POINT ( 'NONE',  ( 2.655984681222220721E-16, 14.66562499938548214, 25.66244784525396483 ) ) ;
#3778 = CARTESIAN_POINT ( 'NONE',  ( 6.684375000614518392, 6.421520780324663323E-16, -5.243569643749999010 ) ) ;
#3779 = LINE ( 'NONE', #14845, #55017 ) ;
#3780 = CARTESIAN_POINT ( 'NONE',  ( 13.75312500061451715, -4.541064518000417216, -2.621784821875001281 ) ) ;
#3781 = CARTESIAN_POINT ( 'NONE',  ( 8.859375000614518214, -4.541064518000417216, -2.621784821875001281 ) ) ;
#3782 = CARTESIAN_POINT ( 'NONE',  ( 27.75000000122903288, 5.773502691896255534, 3.535250795749688894E-16 ) ) ;
#3783 =( BOUNDED_CURVE ( )  B_SPLINE_CURVE ( 2, ( #58927, #30865, #36774, #42323, #13138, #7972, #18309 ),
 .UNSPECIFIED., .F., .F. ) 
 B_SPLINE_CURVE_WITH_KNOTS ( ( 3, 2, 2, 3 ),
 ( 0.1750000000000000167, 0.1777777777777778123, 0.1805555555555555525, 0.1833333333333333204 ),
 .UNSPECIFIED. ) 
 CURVE ( )  GEOMETRIC_REPRESENTATION_ITEM ( )  RATIONAL_B_SPLINE_CURVE ( ( 0.9999999999999986677, 0.8660254037844400399, 1.000000000000000000, 0.8660254037844387076, 1.000000000000000000, 0.8660254037844387076, 1.000000000000000000 ) ) 
 REPRESENTATION_ITEM ( '' )  );
#3784 = CARTESIAN_POINT ( 'NONE',  ( 16.92187500061451999, -6.054752690667223547, -1.112240025338166033E-15 ) ) ;
#3785 = CARTESIAN_POINT ( 'NONE',  ( 4.246875000614519280, -3.027376345333614438, 5.243569643749998122 ) ) ;
#3786 = CARTESIAN_POINT ( 'NONE',  ( 29.88749999999999929, 5.773502691896255534, 3.535250795749688894E-16 ) ) ;
#3787 = CARTESIAN_POINT ( 'NONE',  ( 4.715625000614516615, -6.054752690667223547, -1.112240025338166033E-15 ) ) ;
#3788 =( BOUNDED_CURVE ( )  B_SPLINE_CURVE ( 2, ( #70049, #14258, #64870, #13520, #26082, #64134, #24975, #13895, #9093 ),
 .UNSPECIFIED., .F., .F. ) 
 B_SPLINE_CURVE_WITH_KNOTS ( ( 3, 2, 2, 2, 3 ),
 ( 0.7934782608695651884, 0.7971014492753623060, 0.8043478260869565410, 0.8115942028985507761, 0.8152173913043478937 ),
 .UNSPECIFIED. ) 
 CURVE ( )  GEOMETRIC_REPRESENTATION_ITEM ( )  RATIONAL_B_SPLINE_CURVE ( ( 0.9330127018922194093, 0.9330127018922194093, 1.000000000000000000, 0.8660254037844387076, 1.000000000000000000, 0.8660254037844387076, 1.000000000000000000, 0.9330127018922182991, 0.9330127018922192983 ) ) 
 REPRESENTATION_ITEM ( '' )  );
#3789 = CARTESIAN_POINT ( 'NONE',  ( 14.84062500061451750, 6.054752690667223547, 3.707466751127219781E-16 ) ) ;
#3790 = VERTEX_POINT ( 'NONE', #15258 ) ;
#3791 = B_SPLINE_CURVE_WITH_KNOTS ( 'NONE', 3,
 ( #68225, #40147, #62665, #12060, #41950, #8326, #47488, #31958, #31597, #54496 ),
 .UNSPECIFIED., .F., .F.,
 ( 4, 3, 3, 4 ),
 ( 1.786133494513239154E-16, 0.0001572325902286019026, 0.0003144664392359658575, 0.0005105429261828870087 ),
 .UNSPECIFIED. ) ;
#3792 = CARTESIAN_POINT ( 'NONE',  ( 13.41562500061451502, 3.027376345333613106, -5.243569643749998122 ) ) ;
#3793 = CARTESIAN_POINT ( 'NONE',  ( 5.887500001229034829, -4.330127018922194537, 2.499999999999995559 ) ) ;
#3794 = CARTESIAN_POINT ( 'NONE',  ( 9.403125000614517504, 4.541064518000418104, -2.621784821874998173 ) ) ;
#3795 = CARTESIAN_POINT ( 'NONE',  ( 22.24687500061451217, -2.746126346562646425, 4.756430356249996549 ) ) ;
#3796 = CARTESIAN_POINT ( 'NONE',  ( 8.287499999999999645, 5.773502691896255534, 3.535250795749688894E-16 ) ) ;
#3797 = CARTESIAN_POINT ( 'NONE',  ( 4.575000001229033941, -5.773502691896255534, -1.060575238724906372E-15 ) ) ;
#3798 = CARTESIAN_POINT ( 'NONE',  ( 17.21249999999999858, 2.886751345948129099, -4.999999999999998224 ) ) ;
#3799 =( BOUNDED_CURVE ( )  B_SPLINE_CURVE ( 2, ( #54792, #72152, #21902, #44458, #59957, #32989, #72885 ),
 .UNSPECIFIED., .F., .F. ) 
 B_SPLINE_CURVE_WITH_KNOTS ( ( 3, 2, 2, 3 ),
 ( 0.4083333333333333814, 0.4111111111111111494, 0.4138888888888889173, 0.4166666666666667407 ),
 .UNSPECIFIED. ) 
 CURVE ( )  GEOMETRIC_REPRESENTATION_ITEM ( )  RATIONAL_B_SPLINE_CURVE ( ( 0.9999999999999973355, 0.8660254037844413721, 1.000000000000000000, 0.8660254037844387076, 1.000000000000000000, 0.8660254037844360431, 1.000000000000002665 ) ) 
 REPRESENTATION_ITEM ( '' )  );
#3800 = CARTESIAN_POINT ( 'NONE',  ( 17.52187500061451431, 3.027376345333613106, -5.243569643749998122 ) ) ;
#3801 = CARTESIAN_POINT ( 'NONE',  ( 14.96250000122903323, -4.330127018922190985, -2.500000000000001332 ) ) ;
#3802 = CARTESIAN_POINT ( 'NONE',  ( 22.94999999999999929, -4.330127018922190985, -2.500000000000001332 ) ) ;
#3803 = CARTESIAN_POINT ( 'NONE',  ( -4.243569643749999898, 16.65312500061451573, -30.00000000000000000 ) ) ;
#3804 = CARTESIAN_POINT ( 'NONE',  ( 3.199386026630491209, 3.842393604469308777, 3.568064829105276115 ) ) ;
#3805 = CARTESIAN_POINT ( 'NONE',  ( 2.817472997146174052, -4.130598735093008678, -2.817472997146206026 ) ) ;
#3806 = CARTESIAN_POINT ( 'NONE',  ( 18.54375000122903216, -2.886751345948181946, -4.999999999999904077 ) ) ;
#3807 = CARTESIAN_POINT ( 'NONE',  ( 28.15312500061451573, -4.541064518000417216, -2.621784821875001281 ) ) ;
#3808 = CARTESIAN_POINT ( 'NONE',  ( 28.23749999999999716, -2.886751345948137093, 4.999999999999984901 ) ) ;
#3809 = CARTESIAN_POINT ( 'NONE',  ( 3.896829055840048017, -3.132845880275759054, -4.204794798714403647 ) ) ;
#3810 = CARTESIAN_POINT ( 'NONE',  ( 15.34687500061451537, 6.054752690667223547, 3.707466751127219781E-16 ) ) ;
#3811 = CARTESIAN_POINT ( 'NONE',  ( 28.46249999999999858, 2.886751345948129099, -4.999999999999998224 ) ) ;
#3812 = ADVANCED_FACE ( 'NONE', ( #16351 ), #38538, .F. ) ;
#3813 = CARTESIAN_POINT ( 'NONE',  ( 12.47812500061451502, 6.421520780324663323E-16, -5.243569643749999010 ) ) ;
#3814 = CARTESIAN_POINT ( 'NONE',  ( 29.48437500061451644, -2.746126346562642428, -4.756430356249999214 ) ) ;
#3815 = CARTESIAN_POINT ( 'NONE',  ( 20.40937500061451715, 0.000000000000000000, 5.243569643749999010 ) ) ;
#3816 = CARTESIAN_POINT ( 'NONE',  ( 16.95937500061451431, 2.746126346562645981, -4.756430356249997438 ) ) ;
#3817 = CARTESIAN_POINT ( 'NONE',  ( 8.090625000614515727, 6.054752690667223547, 3.707466751127219781E-16 ) ) ;
#3818 = CARTESIAN_POINT ( 'NONE',  ( 12.53437500061451537, 6.421520780324663323E-16, -5.243569643749999010 ) ) ;
#3819 = ORIENTED_EDGE ( 'NONE', *, *, #23299, .T. ) ;
#3820 = CARTESIAN_POINT ( 'NONE',  ( 24.83437500061451431, 4.541064518000418104, 2.621784821874999949 ) ) ;
#3821 = CARTESIAN_POINT ( 'NONE',  ( 27.44062500061451715, 6.054752690667223547, 3.707466751127219781E-16 ) ) ;
#3822 = CARTESIAN_POINT ( 'NONE',  ( 26.02499999999999858, -4.330127018922194537, 2.499999999999995559 ) ) ;
#3823 = CARTESIAN_POINT ( 'NONE',  ( 8.474999999999999645, -4.330127018922194537, 2.499999999999995559 ) ) ;
#3824 = CARTESIAN_POINT ( 'NONE',  ( 16.16250000122903430, 0.000000000000000000, 4.999999999999998224 ) ) ;
#3825 = CARTESIAN_POINT ( 'NONE',  ( 16.55625000122903145, 0.000000000000000000, 4.999999999999998224 ) ) ;
#3826 = CARTESIAN_POINT ( 'NONE',  ( 8.709375000614516082, -5.492252693125287522, -1.008910452111647106E-15 ) ) ;
#3827 = ORIENTED_EDGE ( 'NONE', *, *, #69060, .T. ) ;
#3828 = CARTESIAN_POINT ( 'NONE',  ( 15.48749999999999893, 5.773502691896255534, 3.535250795749688894E-16 ) ) ;
#3829 = CARTESIAN_POINT ( 'NONE',  ( 18.82500000000000284, -4.330127018922194537, 2.499999999999995559 ) ) ;
#3830 = CARTESIAN_POINT ( 'NONE',  ( 11.46562500061451573, -6.054752690667223547, -1.112240025338166033E-15 ) ) ;
#3831 = ORIENTED_EDGE ( 'NONE', *, *, #71724, .T. ) ;
#3832 = CARTESIAN_POINT ( 'NONE',  ( -3.999999999999999112, 10.96250000000000213, -32.30940107675850470 ) ) ;
#3833 = CARTESIAN_POINT ( 'NONE',  ( -2.121784821874999949, 17.98437500061451999, -33.67503911421598417 ) ) ;
#3834 = CARTESIAN_POINT ( 'NONE',  ( 3.140625000614516882, 6.054752690667223547, 3.707466751127219781E-16 ) ) ;
#3835 = CARTESIAN_POINT ( 'NONE',  ( 1.878215178125000495, 12.71562499938548463, 26.74683588394047007 ) ) ;
#3836 = CARTESIAN_POINT ( 'NONE',  ( 10.68750000000000000, -2.886751345948129988, 4.999999999999997335 ) ) ;
#3837 = CARTESIAN_POINT ( 'NONE',  ( 3.837848076843224376, 3.204827942194517831, -3.837848076843224376 ) ) ;
#3838 = VERTEX_POINT ( 'NONE', #26727 ) ;
#3839 = CARTESIAN_POINT ( 'NONE',  ( -4.243569643749997233, 13.99062500061451786, 32.45002607614398471 ) ) ;
#3840 = CARTESIAN_POINT ( 'NONE',  ( 26.69062500061451715, -3.027376345333614438, 5.243569643749998122 ) ) ;
#3841 = CARTESIAN_POINT ( 'NONE',  ( 29.36250000122903003, -4.330127018922190985, -2.500000000000001332 ) ) ;
#3842 = CARTESIAN_POINT ( 'NONE',  ( 20.10000000000000142, 0.000000000000000000, 4.999999999999998224 ) ) ;
#3843 = CARTESIAN_POINT ( 'NONE',  ( 20.70937500061451786, 4.541064518000418104, -2.621784821874998173 ) ) ;
#3844 = CARTESIAN_POINT ( 'NONE',  ( 19.94062500061451715, -3.027376345333614438, 5.243569643749998122 ) ) ;
#3845 = CARTESIAN_POINT ( 'NONE',  ( -2.121784821874999949, 13.87812500061459353, -33.67503911421598417 ) ) ;
#3846 = CARTESIAN_POINT ( 'NONE',  ( 23.66250000122903430, 4.330127018922192761, -2.499999999999997780 ) ) ;
#3847 = CARTESIAN_POINT ( 'NONE',  ( 3.178125000614515638, 4.541064518000418104, 2.621784821874999949 ) ) ;
#3848 = CARTESIAN_POINT ( 'NONE',  ( 26.67187500061451644, 2.746126346562643317, 4.756430356249998326 ) ) ;
#3849 = CARTESIAN_POINT ( 'NONE',  ( 21.59062500061451928, 6.054752690667223547, 3.707466751127219781E-16 ) ) ;
#3850 = CARTESIAN_POINT ( 'NONE',  ( 7.921875000614517326, -5.492252693125287522, -1.008910452111647106E-15 ) ) ;
#3851 = CARTESIAN_POINT ( 'NONE',  ( -3.756430356249999214, 15.97812499938548392, 27.83122392262697531 ) ) ;
#3852 = CARTESIAN_POINT ( 'NONE',  ( 15.08437500061451786, -4.541064518000419881, 2.621784821874995952 ) ) ;
#3853 = CARTESIAN_POINT ( 'NONE',  ( 13.39687500061451608, -3.027376345333610441, -5.243569643749999898 ) ) ;
#3854 = CARTESIAN_POINT ( 'NONE',  ( 24.04687500061451644, -3.027376345333614438, 5.243569643749998122 ) ) ;
#3855 = CARTESIAN_POINT ( 'NONE',  ( 4.243569643749999898, 13.29687500061451999, 32.45002607614398471 ) ) ;
#3856 = CARTESIAN_POINT ( 'NONE',  ( 4.978125000614518569, 4.541064518000418104, 2.621784821874999949 ) ) ;
#3857 = CARTESIAN_POINT ( 'NONE',  ( 29.09062500061451573, -3.027376345333610441, -5.243569643749999898 ) ) ;
#3858 = CARTESIAN_POINT ( 'NONE',  ( 28.07812500061451289, -4.541064518000419881, 2.621784821874995952 ) ) ;
#3859 = FACE_OUTER_BOUND ( 'NONE', #40436, .T. ) ;
#3860 = CARTESIAN_POINT ( 'NONE',  ( 7.284375000614518036, 4.541064518000418104, 2.621784821874999949 ) ) ;
#3861 =( NAMED_UNIT ( * ) PLANE_ANGLE_UNIT ( ) SI_UNIT ( $, .RADIAN. ) );
#3862 = CARTESIAN_POINT ( 'NONE',  ( 14.28750000122903430, 4.330127018922191873, 2.499999999999999556 ) ) ;
#3863 = CARTESIAN_POINT ( 'NONE',  ( 8.587500001229035007, -4.330127018922194537, 2.499999999999995559 ) ) ;
#3864 = CARTESIAN_POINT ( 'NONE',  ( 4.528125000614516615, 4.541064518000418104, 2.621784821874999949 ) ) ;
#3865 = CARTESIAN_POINT ( 'NONE',  ( -4.000000000000000000, 16.71874999877096712, 30.00000000000000000 ) ) ;
#3866 = CARTESIAN_POINT ( 'NONE',  ( 17.60625000122903572, -4.330127018922190985, -2.500000000000001332 ) ) ;
#3867 = CARTESIAN_POINT ( 'NONE',  ( 13.62187500061451750, 3.027376345333611329, 5.243569643749999010 ) ) ;
#3868 = CARTESIAN_POINT ( 'NONE',  ( 12.00000000000000000, 0.000000000000000000, 4.999999999999998224 ) ) ;
#3869 = VERTEX_POINT ( 'NONE', #49989 ) ;
#3870 = CARTESIAN_POINT ( 'NONE',  ( 21.96562500061451573, 3.027376345333613106, -5.243569643749998122 ) ) ;
#3871 = CARTESIAN_POINT ( 'NONE',  ( 7.490625000614516082, -3.027376345333610441, -5.243569643749999898 ) ) ;
#3872 = CARTESIAN_POINT ( 'NONE',  ( 24.94687500061451502, -3.027376345333614438, 5.243569643749998122 ) ) ;
#3873 = CARTESIAN_POINT ( 'NONE',  ( 7.153125000614518392, 4.541064518000418104, -2.621784821874998173 ) ) ;
#3874 = CARTESIAN_POINT ( 'NONE',  ( 1.626862140677534273E-15, 13.02500000122903501, 34.00000000000000000 ) ) ;
#3875 = CARTESIAN_POINT ( 'NONE',  ( 8.850000001229034297, 5.773502691896255534, 3.535250795749688894E-16 ) ) ;
#3876 = EDGE_CURVE ( 'NONE', #32339, #21346, #47148, .T. ) ;
#3877 = CARTESIAN_POINT ( 'NONE',  ( 23.42812500061451786, 4.541064518000418104, 2.621784821874999949 ) ) ;
#3878 = VECTOR ( 'NONE', #66320, 1000.000000000000000 ) ;
#3879 = CARTESIAN_POINT ( 'NONE',  ( -4.243569643749999898, 11.25312500061451892, -30.00000000000000000 ) ) ;
#3880 = CARTESIAN_POINT ( 'NONE',  ( 9.675000001229035362, 2.886751345948129099, -4.999999999999998224 ) ) ;
#3881 = CARTESIAN_POINT ( 'NONE',  ( 20.20312500061451644, 4.541064518000418104, -2.621784821874998173 ) ) ;
#3882 = ADVANCED_FACE ( 'NONE', ( #38906 ), #27093, .T. ) ;
#3883 = CARTESIAN_POINT ( 'NONE',  ( 15.66562500061451857, 3.027376345333613106, -5.243569643749998122 ) ) ;
#3884 = CARTESIAN_POINT ( 'NONE',  ( 28.24687500061451573, -2.746126346562642428, -4.756430356249999214 ) ) ;
#3885 = CARTESIAN_POINT ( 'NONE',  ( 19.01249999999999929, 2.886751345948129099, -4.999999999999998224 ) ) ;
#3886 = CARTESIAN_POINT ( 'NONE',  ( 11.06250000122903288, 4.330127018922192761, -2.499999999999997780 ) ) ;
#3887 = CARTESIAN_POINT ( 'NONE',  ( 7.640625000614517326, 6.054752690667223547, 3.707466751127219781E-16 ) ) ;
#3888 = CARTESIAN_POINT ( 'NONE',  ( 12.10312500061451857, 4.541064518000418104, -2.621784821874998173 ) ) ;
#3889 = EDGE_CURVE ( 'NONE', #52141, #43575, #36784, .T. ) ;
#3890 = CARTESIAN_POINT ( 'NONE',  ( 23.88750000122903216, -4.330127018922194537, 2.499999999999995559 ) ) ;
#3891 = CARTESIAN_POINT ( 'NONE',  ( 21.53437500061451715, 6.421520780324663323E-16, -5.243569643749999010 ) ) ;
#3892 = CARTESIAN_POINT ( 'NONE',  ( 9.528763966825557376E-15, 17.41249999999999787, 34.00000000000000000 ) ) ;
#3893 = EDGE_CURVE ( 'NONE', #19531, #54070, #3799, .T. ) ;
#3894 = CARTESIAN_POINT ( 'NONE',  ( 4.800000001229032698, 5.773502691896255534, 3.535250795749688894E-16 ) ) ;
#3895 = CARTESIAN_POINT ( 'NONE',  ( 4.284375000614518925, -4.541064518000419881, 2.621784821874995952 ) ) ;
#3896 = CARTESIAN_POINT ( 'NONE',  ( 22.50937500061451857, 4.541064518000418104, -2.621784821874998173 ) ) ;
#3897 = CARTESIAN_POINT ( 'NONE',  ( 1.626862140677534470E-15, 12.83750000000000213, 34.00000000000000000 ) ) ;
#3898 = CARTESIAN_POINT ( 'NONE',  ( 19.82812500061451644, 4.541064518000418104, 2.621784821874999949 ) ) ;
#3899 = CARTESIAN_POINT ( 'NONE',  ( 24.34687500061451715, 6.054752690667223547, 3.707466751127219781E-16 ) ) ;
#3900 = CARTESIAN_POINT ( 'NONE',  ( 3.756430356250000546, 19.54062499938548214, 27.83122392262697886 ) ) ;
#3901 = DIRECTION ( 'NONE',  ( 0.000000000000000000, 0.000000000000000000, -1.000000000000000000 ) ) ;
#3902 = CARTESIAN_POINT ( 'NONE',  ( -1.999999999999997113, 13.43750000122903465, -26.53589838486224295 ) ) ;
#3903 = CARTESIAN_POINT ( 'NONE',  ( 4.959375000614516971, 4.541064518000418104, -2.621784821874998173 ) ) ;
#3904 = CARTESIAN_POINT ( 'NONE',  ( 15.44062500061451537, -3.027376345333614438, 5.243569643749998122 ) ) ;
#3905 = CARTESIAN_POINT ( 'NONE',  ( 13.58437500061451786, 4.541064518000418104, 2.621784821874999949 ) ) ;
#3906 = EDGE_LOOP ( 'NONE', ( #30780, #16162, #10676, #50533 ) ) ;
#3907 = CARTESIAN_POINT ( 'NONE',  ( 1.999999999999998668, 17.15000000000000213, -33.46410161513775705 ) ) ;
#3908 = CARTESIAN_POINT ( 'NONE',  ( 25.56562500061452070, 3.027376345333613106, -5.243569643749998122 ) ) ;
#3909 = CARTESIAN_POINT ( 'NONE',  ( 4.000000000000000000, 17.03750000000000142, 32.30940107675849760 ) ) ;
#3910 = CARTESIAN_POINT ( 'NONE',  ( -5.810221930991193690E-16, 11.45000000122903216, -34.00000000000000000 ) ) ;
#3911 = CARTESIAN_POINT ( 'NONE',  ( 14.17500000000000071, 4.330127018922191873, 2.499999999999999556 ) ) ;
#3912 = CARTESIAN_POINT ( 'NONE',  ( 23.32500000122903572, 2.886751345948126879, 4.999999999999999112 ) ) ;
#3913 = CARTESIAN_POINT ( 'NONE',  ( 19.64062500061451644, -3.027376345333610441, -5.243569643749999898 ) ) ;
#3914 = ORIENTED_EDGE ( 'NONE', *, *, #55506, .T. ) ;
#3915 = CARTESIAN_POINT ( 'NONE',  ( 23.55000000000000071, 4.330127018922192761, -2.499999999999997780 ) ) ;
#3916 = CARTESIAN_POINT ( 'NONE',  ( 24.98437500061451644, -4.541064518000419881, 2.621784821874995952 ) ) ;
#3917 = VERTEX_POINT ( 'NONE', #21531 ) ;
#3918 = CARTESIAN_POINT ( 'NONE',  ( 11.55000000000000071, 0.000000000000000000, 4.999999999999998224 ) ) ;
#3919 = CARTESIAN_POINT ( 'NONE',  ( 11.35312500061451679, 0.000000000000000000, 5.243569643749999010 ) ) ;
#3920 = CARTESIAN_POINT ( 'NONE',  ( 4.565625000614516260, 3.027376345333611329, 5.243569643749999010 ) ) ;
#3921 = CARTESIAN_POINT ( 'NONE',  ( 13.47187500061451715, 4.119189519843966529, 2.378215178124999607 ) ) ;
#3922 = CARTESIAN_POINT ( 'NONE',  ( 26.99062500061451431, 6.054752690667223547, 3.707466751127219781E-16 ) ) ;
#3923 = CARTESIAN_POINT ( 'NONE',  ( 16.80000000000000071, 4.330127018922192761, -2.499999999999997780 ) ) ;
#3924 = CARTESIAN_POINT ( 'NONE',  ( 27.75000000000000000, 0.000000000000000000, 4.999999999999998224 ) ) ;
#3925 = CARTESIAN_POINT ( 'NONE',  ( 1.071796769724491893, 14.15134618820330203, 34.00000000000000000 ) ) ;
#3926 = CARTESIAN_POINT ( 'NONE',  ( 7.284375000614518036, 4.541064518000418104, 2.621784821874999949 ) ) ;
#3927 = CARTESIAN_POINT ( 'NONE',  ( 18.12187500061451573, 3.027376345333611329, 5.243569643749999010 ) ) ;
#3928 = CARTESIAN_POINT ( 'NONE',  ( 25.98750000000000782, -2.886751345948163738, 4.999999999999939604 ) ) ;
#3929 = ORIENTED_EDGE ( 'NONE', *, *, #23306, .F. ) ;
#3930 = CARTESIAN_POINT ( 'NONE',  ( 26.42812500061451431, 6.421520780324663323E-16, -5.243569643749999010 ) ) ;
#3931 = CARTESIAN_POINT ( 'NONE',  ( 27.94687500061451502, 6.054752690667223547, 3.707466751127219781E-16 ) ) ;
#3932 = DIRECTION ( 'NONE',  ( -0.000000000000000000, -1.000000000000000000, -0.000000000000000000 ) ) ;
#3933 = CARTESIAN_POINT ( 'NONE',  ( 13.57500000000000107, 6.123233995736764310E-16, -4.999999999999998224 ) ) ;
#3934 = CARTESIAN_POINT ( 'NONE',  ( 11.12812500061451715, 6.421520780324663323E-16, -5.243569643749999010 ) ) ;
#3935 = CARTESIAN_POINT ( 'NONE',  ( -3.999999999999999112, 19.43750000000000000, 27.69059892324149530 ) ) ;
#3936 = CARTESIAN_POINT ( 'NONE',  ( -1.999999999999999112, 17.99374999877096570, 26.53589838486224650 ) ) ;
#3937 = CARTESIAN_POINT ( 'NONE',  ( 27.85312500061451502, 4.541064518000418104, -2.621784821874998173 ) ) ;
#3938 = CARTESIAN_POINT ( 'NONE',  ( 16.76250000122903216, -4.330127018922190985, -2.500000000000001332 ) ) ;
#3939 = CARTESIAN_POINT ( 'NONE',  ( 3.766124272970669651, -4.056654931390053953, 3.460806837557585336 ) ) ;
#3940 = CARTESIAN_POINT ( 'NONE',  ( 15.60937500061451644, -4.119189519843965641, -2.378215178125001383 ) ) ;
#3941 = CARTESIAN_POINT ( 'NONE',  ( 4.790625000614518569, -3.027376345333610441, -5.243569643749999898 ) ) ;
#3942 = CARTESIAN_POINT ( 'NONE',  ( 20.89687500061452141, -3.027376345333614438, 5.243569643749998122 ) ) ;
#3943 = CARTESIAN_POINT ( 'NONE',  ( 2.121784821875001281, 17.75937500061451502, 33.67503911421598417 ) ) ;
#3944 = CARTESIAN_POINT ( 'NONE',  ( 23.03437500061451715, 4.541064518000418104, 2.621784821874999949 ) ) ;
#3945 = CARTESIAN_POINT ( 'NONE',  ( 4.237500000000001599, 5.773502691896255534, 3.535250795749688894E-16 ) ) ;
#3946 = CARTESIAN_POINT ( 'NONE',  ( 3.999999999999999112, 11.33750000122903501, 30.00000000000000000 ) ) ;
#3947 = CARTESIAN_POINT ( 'NONE',  ( 11.91562500061451857, -6.054752690667223547, -1.112240025338166033E-15 ) ) ;
#3948 = CARTESIAN_POINT ( 'NONE',  ( 4.987500001229032698, -4.330127018922194537, 2.499999999999995559 ) ) ;
#3949 = CARTESIAN_POINT ( 'NONE',  ( 9.646875000614516082, -3.027376345333614438, 5.243569643749998122 ) ) ;
#3950 = CARTESIAN_POINT ( 'NONE',  ( 13.06875000122903252, -5.773502691896255534, -1.060575238724906372E-15 ) ) ;
#3951 = CARTESIAN_POINT ( 'NONE',  ( 9.140625000614518214, -3.027376345333614438, 5.243569643749998122 ) ) ;
#3952 = CARTESIAN_POINT ( 'NONE',  ( 14.07187500061451679, 3.027376345333611329, 5.243569643749999010 ) ) ;
#3953 = CARTESIAN_POINT ( 'NONE',  ( 24.50625000122903074, 4.330127018922192761, -2.499999999999997780 ) ) ;
#3954 = CARTESIAN_POINT ( 'NONE',  ( 21.52500000122903145, 2.886751345948126879, 4.999999999999999112 ) ) ;
#3955 = CARTESIAN_POINT ( 'NONE',  ( 10.17187500061451999, -6.054752690667223547, -1.112240025338166033E-15 ) ) ;
#3956 = CARTESIAN_POINT ( 'NONE',  ( 11.76562500061451644, 3.027376345333611329, 5.243569643749999010 ) ) ;
#3957 = CARTESIAN_POINT ( 'NONE',  ( 29.15625000122903288, 0.000000000000000000, 4.999999999999998224 ) ) ;
#3958 = CARTESIAN_POINT ( 'NONE',  ( 22.47187500061451715, 3.027376345333613106, -5.243569643749998122 ) ) ;
#3959 = CARTESIAN_POINT ( 'NONE',  ( 26.90625000122902932, 0.000000000000000000, 4.999999999999998224 ) ) ;
#3960 = CARTESIAN_POINT ( 'NONE',  ( -4.000165449326166467, 2.999779401354844222, 29.86626784624999686 ) ) ;
#3961 = CARTESIAN_POINT ( 'NONE',  ( 3.286795329855858760, 3.767887532774327308, -3.286795329856085690 ) ) ;
#3962 = CARTESIAN_POINT ( 'NONE',  ( 4.243569643749999898, 11.49687500061451928, -27.54997392385601529 ) ) ;
#3963 = CARTESIAN_POINT ( 'NONE',  ( 15.18750000122903465, 4.330127018922191873, 2.499999999999999556 ) ) ;
#3964 = EDGE_CURVE ( 'NONE', #33074, #10265, #6156, .T. ) ;
#3965 = CARTESIAN_POINT ( 'NONE',  ( 8.971875000614515372, 3.027376345333613106, -5.243569643749998122 ) ) ;
#3966 = CARTESIAN_POINT ( 'NONE',  ( -4.243569643749999898, 16.61562500061451786, -32.45002607614398471 ) ) ;
#3967 = CARTESIAN_POINT ( 'NONE',  ( 18.52500000122903145, -5.773502691896255534, -1.060575238724906372E-15 ) ) ;
#3968 = CARTESIAN_POINT ( 'NONE',  ( 10.60312500061451679, -4.541064518000417216, -2.621784821875001281 ) ) ;
#3969 = EDGE_LOOP ( 'NONE', ( #38470, #37871, #37135, #21085, #9447, #39565, #454, #49334, #57532, #30105, #69830, #43814, #15641, #22569, #61517, #15338, #6826, #41283, #5734, #50296, #19819, #53002, #52502, #21761, #36258, #29483, #62501, #50659, #31162, #28528, #2803, #23071, #10901, #23829, #14031, #59663, #20232, #21301, #19195, #60039, #44630, #32712, #23652, #32547, #4840, #34362, #911, #52509, #22582, #58085, #33339, #45827, #27225, #48022, #64051, #16436, #17205, #44911, #31975, #29923, #29249, #3387, #7442, #35869, #45244, #40070, #52077, #23066, #67874, #71276, #16373, #61647, #11771, #14855, #44854, #54439, #45179, #33522, #29666, #14102, #18956, #50395, #23163, #18490, #48751, #64611, #55896, #8587, #54471, #58855, #52237, #6386, #37665, #7894, #21537, #71421, #47543, #41892, #71650, #64408, #39084, #40079, #67576 ) ) ;
#3970 = CARTESIAN_POINT ( 'NONE',  ( 15.15000000000000036, 0.000000000000000000, 4.999999999999998224 ) ) ;
#3971 = CARTESIAN_POINT ( 'NONE',  ( 10.13437500061451679, -4.541064518000419881, 2.621784821874995952 ) ) ;
#3972 = EDGE_CURVE ( 'NONE', #20508, #37144, #21249, .T. ) ;
#3973 = DIRECTION ( 'NONE',  ( -0.000000000000000000, -1.000000000000000000, -0.000000000000000000 ) ) ;
#3974 = CARTESIAN_POINT ( 'NONE',  ( 10.01250000122903394, -4.330127018922190985, -2.500000000000001332 ) ) ;
#3975 = CARTESIAN_POINT ( 'NONE',  ( 18.26250000122903216, 4.330127018922192761, -2.499999999999997780 ) ) ;
#3976 = CARTESIAN_POINT ( 'NONE',  ( 14.24062500061451608, -3.027376345333610441, -5.243569643749999898 ) ) ;
#3977 = ADVANCED_FACE ( 'NONE', ( #20799 ), #51796, .T. ) ;
#3978 = CARTESIAN_POINT ( 'NONE',  ( 19.22812500061451502, 6.421520780324663323E-16, -5.243569643749999010 ) ) ;
#3979 = CARTESIAN_POINT ( 'NONE',  ( 27.18750000122903288, 6.123233995736764310E-16, -4.999999999999998224 ) ) ;
#3980 = CARTESIAN_POINT ( 'NONE',  ( 29.55000000122903003, 5.773502691896255534, 3.535250795749688894E-16 ) ) ;
#3981 = CARTESIAN_POINT ( 'NONE',  ( 24.07499999999999929, 4.330127018922191873, 2.499999999999999556 ) ) ;
#3982 = CARTESIAN_POINT ( 'NONE',  ( -3.756430356250000102, 14.66562499938548214, 30.00000000000000000 ) ) ;
#3983 = CARTESIAN_POINT ( 'NONE',  ( 27.56250000000000000, 2.886751345948129099, -4.999999999999998224 ) ) ;
#3984 = CARTESIAN_POINT ( 'NONE',  ( 25.24687500061451573, 6.054752690667223547, 3.707466751127219781E-16 ) ) ;
#3985 = CARTESIAN_POINT ( 'NONE',  ( -5.810221930991193690E-16, 12.68750000000000000, -34.00000000000000000 ) ) ;
#3986 = CARTESIAN_POINT ( 'NONE',  ( 13.16250000122903430, -4.330127018922190985, -2.500000000000001332 ) ) ;
#3987 = CARTESIAN_POINT ( 'NONE',  ( 3.825000000000001954, 4.330127018922191873, 2.499999999999999556 ) ) ;
#3988 = CYLINDRICAL_SURFACE ( 'NONE', #17234, 3.999999999999996447 ) ;
#3989 = CARTESIAN_POINT ( 'NONE',  ( 6.496875000614517504, -3.027376345333614438, 5.243569643749998122 ) ) ;
#3990 = CARTESIAN_POINT ( 'NONE',  ( 26.54062500061451146, 6.054752690667223547, 3.707466751127219781E-16 ) ) ;
#3991 = CARTESIAN_POINT ( 'NONE',  ( 0.000000000000000000, 27.50000000000000000, 30.00000000000000000 ) ) ;
#3992 = CARTESIAN_POINT ( 'NONE',  ( -0.8069677186600781038, 9.969399234781869623, -24.05111887509274737 ) ) ;
#3993 = LINE ( 'NONE', #20959, #19397 ) ;
#3994 = CARTESIAN_POINT ( 'NONE',  ( 6.384375000614516793, 4.541064518000418104, 2.621784821874999949 ) ) ;
#3995 = CARTESIAN_POINT ( 'NONE',  ( 8.934375000614517504, 6.421520780324663323E-16, -5.243569643749999010 ) ) ;
#3996 = CARTESIAN_POINT ( 'NONE',  ( 29.29687500061451644, 6.054752690667223547, 3.707466751127219781E-16 ) ) ;
#3997 = EDGE_CURVE ( 'NONE', #49995, #54869, #13553, .T. ) ;
#3998 = CARTESIAN_POINT ( 'NONE',  ( 2.121784821875001281, 12.75312500061459353, 33.67503911421598417 ) ) ;
#3999 = CARTESIAN_POINT ( 'NONE',  ( 22.12500000000000000, 6.123233995736764310E-16, -4.999999999999998224 ) ) ;
#4000 =( REPRESENTATION_RELATIONSHIP ('NONE','NONE', #33485, #68023 ) REPRESENTATION_RELATIONSHIP_WITH_TRANSFORMATION ( #67734 )SHAPE_REPRESENTATION_RELATIONSHIP( ) );
#4001 = CARTESIAN_POINT ( 'NONE',  ( 29.36250000000000071, 2.886751345948129099, -4.999999999999998224 ) ) ;
#4002 =( BOUNDED_CURVE ( )  B_SPLINE_CURVE ( 2, ( #62035, #11431, #33950, #62755, #5885, #28416, #57202 ),
 .UNSPECIFIED., .F., .F. ) 
 B_SPLINE_CURVE_WITH_KNOTS ( ( 3, 2, 2, 3 ),
 ( 0.9685383496433896955, 0.9694444444444444420, 0.9722222222222222099, 0.9730456312742340463 ),
 .UNSPECIFIED. ) 
 CURVE ( )  GEOMETRIC_REPRESENTATION_ITEM ( )  RATIONAL_B_SPLINE_CURVE ( ( 0.9411070399833363354, 0.9562982733624414422, 1.000000000000000000, 0.8660254037844387076, 1.000000000000000000, 0.9602862777051311971, 0.9441170150774715886 ) ) 
 REPRESENTATION_ITEM ( '' )  );
#4003 = CARTESIAN_POINT ( 'NONE',  ( 4.837500000000001243, -2.886751345948129988, 4.999999999999997335 ) ) ;
#4004 = VERTEX_POINT ( 'NONE', #33714 ) ;
#4005 = CARTESIAN_POINT ( 'NONE',  ( 17.35312500061451502, -4.541064518000417216, -2.621784821875001281 ) ) ;
#4006 = CARTESIAN_POINT ( 'NONE',  ( 11.84062500061451750, -3.027376345333614438, 5.243569643749998122 ) ) ;
#4007 = CARTESIAN_POINT ( 'NONE',  ( 20.85937500061451644, -5.492252693125287522, -1.008910452111647106E-15 ) ) ;
#4008 = CARTESIAN_POINT ( 'NONE',  ( 8.071875000614518569, 3.027376345333613106, -5.243569643749998122 ) ) ;
#4009 = CARTESIAN_POINT ( 'NONE',  ( 23.40000000000000213, -4.330127018922190985, -2.500000000000001332 ) ) ;
#4010 = CARTESIAN_POINT ( 'NONE',  ( 21.18750000122903288, -4.330127018922194537, 2.499999999999995559 ) ) ;
#4011 = CARTESIAN_POINT ( 'NONE',  ( 16.06875000122903074, 2.886751345948126879, 4.999999999999998224 ) ) ;
#4012 = CARTESIAN_POINT ( 'NONE',  ( 8.634375000614518569, 4.541064518000418104, 2.621784821874999949 ) ) ;
#4013 = CARTESIAN_POINT ( 'NONE',  ( 15.08437500061451786, -4.541064518000419881, 2.621784821874995952 ) ) ;
#4014 = CARTESIAN_POINT ( 'NONE',  ( 23.97187500061451360, 3.027376345333611329, 5.243569643749999010 ) ) ;
#4015 = CARTESIAN_POINT ( 'NONE',  ( 4.342984975361706468, -2.477595912125914790, -4.621313785610477787 ) ) ;
#4016 = CARTESIAN_POINT ( 'NONE',  ( 13.19999999999999929, 4.330127018922192761, -2.499999999999997780 ) ) ;
#4017 = CARTESIAN_POINT ( 'NONE',  ( 18.12187500061451573, 3.027376345333611329, 5.243569643749999010 ) ) ;
#4018 = CARTESIAN_POINT ( 'NONE',  ( 8.484375000614518214, 6.421520780324663323E-16, -5.243569643749999010 ) ) ;
#4019 = CARTESIAN_POINT ( 'NONE',  ( -3.756430356250000102, 20.62812499938548072, 30.00000000000000000 ) ) ;
#4020 = CARTESIAN_POINT ( 'NONE',  ( 20.85000000000000142, 4.330127018922192761, -2.499999999999997780 ) ) ;
#4021 = CARTESIAN_POINT ( 'NONE',  ( 3.999999999999998668, 15.61250000000000249, 32.30940107675850470 ) ) ;
#4022 = CARTESIAN_POINT ( 'NONE',  ( -4.243569643749999898, 9.959375000614517859, -30.00000000000000000 ) ) ;
#4023 = CARTESIAN_POINT ( 'NONE',  ( 24.60937500061451644, -4.119189519843965641, -2.378215178125001383 ) ) ;
#4024 = CARTESIAN_POINT ( 'NONE',  ( 13.45312500061451466, 4.541064518000418104, -2.621784821874998173 ) ) ;
#4025 = CARTESIAN_POINT ( 'NONE',  ( 28.65937500061451715, -4.541064518000417216, -2.621784821875001281 ) ) ;
#4026 = CARTESIAN_POINT ( 'NONE',  ( -1.071796769724490339, 19.30490381179669868, -26.00000000000000355 ) ) ;
#4027 = DIRECTION ( 'NONE',  ( -0.000000000000000000, -1.000000000000000000, -0.000000000000000000 ) ) ;
#4028 = CARTESIAN_POINT ( 'NONE',  ( 12.18750000000000000, -2.886751345948125991, -5.000000000000000000 ) ) ;
#4029 = CARTESIAN_POINT ( 'NONE',  ( 3.999999999999998668, 19.02500000122903501, 27.69059892324149175 ) ) ;
#4030 = CARTESIAN_POINT ( 'NONE',  ( 12.75000000122903643, -2.886751345948125991, -5.000000000000000000 ) ) ;
#4031 = CARTESIAN_POINT ( 'NONE',  ( 22.73437500061451644, -4.541064518000419881, 2.621784821874995952 ) ) ;
#4032 = CARTESIAN_POINT ( 'NONE',  ( 15.64687500061451608, -3.027376345333610441, -5.243569643749999898 ) ) ;
#4033 = CARTESIAN_POINT ( 'NONE',  ( 3.999999999999998668, 16.77500000122903145, 27.69059892324149530 ) ) ;
#4034 = VERTEX_POINT ( 'NONE', #22979 ) ;
#4035 = AXIS2_PLACEMENT_3D ( 'NONE', #59247, #14557, #66270 ) ;
#4036 = CARTESIAN_POINT ( 'NONE',  ( 16.30312500061451786, 0.000000000000000000, 5.243569643749999010 ) ) ;
#4037 = CARTESIAN_POINT ( 'NONE',  ( 28.38750000122903216, -4.330127018922194537, 2.499999999999995559 ) ) ;
#4038 = CARTESIAN_POINT ( 'NONE',  ( 16.73437500061451644, 4.541064518000418104, 2.621784821874999949 ) ) ;
#4039 = CARTESIAN_POINT ( 'NONE',  ( 5.878125000614517148, 4.541064518000418104, 2.621784821874999949 ) ) ;
#4040 = CARTESIAN_POINT ( 'NONE',  ( 20.16562500061451146, 3.027376345333613106, -5.243569643749998122 ) ) ;
#4041 = CARTESIAN_POINT ( 'NONE',  ( 28.69687500061451502, -3.027376345333610441, -5.243569643749999898 ) ) ;
#4042 = CARTESIAN_POINT ( 'NONE',  ( 2.121784821875001281, 11.85312500061451857, 33.67503911421598417 ) ) ;
#4043 = CARTESIAN_POINT ( 'NONE',  ( 16.12500000122903288, 2.886751345948126879, 4.999999999999999112 ) ) ;
#4044 = CARTESIAN_POINT ( 'NONE',  ( 9.909375000614517148, 4.119189519843966529, -2.378215178124998275 ) ) ;
#4045 = CARTESIAN_POINT ( 'NONE',  ( 27.02812500061451573, 4.541064518000418104, 2.621784821874999949 ) ) ;
#4046 = CARTESIAN_POINT ( 'NONE',  ( -2.498395430326213790E-14, 18.85624999877096641, 26.00000000000000000 ) ) ;
#4047 = CARTESIAN_POINT ( 'NONE',  ( 21.68437500061451573, 4.541064518000418104, 2.621784821874999949 ) ) ;
#4048 = CARTESIAN_POINT ( 'NONE',  ( 23.43750000122902932, -4.330127018922194537, 2.499999999999995559 ) ) ;
#4049 = CARTESIAN_POINT ( 'NONE',  ( 24.06562500061451715, -6.054752690667223547, -1.112240025338166033E-15 ) ) ;
#4050 = CARTESIAN_POINT ( 'NONE',  ( 16.69687500061451502, 6.054752690667223547, 3.707466751127219781E-16 ) ) ;
#4051 = CARTESIAN_POINT ( 'NONE',  ( 11.39062500061451644, -3.027376345333614438, 5.243569643749998122 ) ) ;
#4052 = CARTESIAN_POINT ( 'NONE',  ( -2.121784821874999949, 15.73437500061451644, 26.32496088578401938 ) ) ;
#4053 = CARTESIAN_POINT ( 'NONE',  ( 16.22812500061451857, 4.541064518000418104, 2.621784821874999949 ) ) ;
#4054 = CARTESIAN_POINT ( 'NONE',  ( 29.31562500061451715, 3.027376345333611329, 5.243569643749999010 ) ) ;
#4055 = VERTEX_POINT ( 'NONE', #69160 ) ;
#4056 = CARTESIAN_POINT ( 'NONE',  ( 23.73749999999999716, -2.886751345948129988, 4.999999999999997335 ) ) ;
#4057 = CARTESIAN_POINT ( 'NONE',  ( 2.121784821874999061, 18.80937500061451928, -33.67503911421598417 ) ) ;
#4058 = CARTESIAN_POINT ( 'NONE',  ( 16.27499999999999858, 6.123233995736764310E-16, -4.999999999999998224 ) ) ;
#4059 = CARTESIAN_POINT ( 'NONE',  ( 24.74062500061451786, 6.054752690667223547, 3.707466751127219781E-16 ) ) ;
#4060 = CARTESIAN_POINT ( 'NONE',  ( 5.540625000614515905, -3.027376345333614438, 5.243569643749998122 ) ) ;
#4061 = CARTESIAN_POINT ( 'NONE',  ( 17.88750000122903216, 4.330127018922191873, 2.499999999999999556 ) ) ;
#4062 = CARTESIAN_POINT ( 'NONE',  ( 22.45312500061451644, 4.541064518000418104, -2.621784821874998173 ) ) ;
#4063 = CARTESIAN_POINT ( 'NONE',  ( 23.13749999999999929, 5.773502691896255534, 3.535250795749688894E-16 ) ) ;
#4064 = EDGE_CURVE ( 'NONE', #19771, #2103, #50714, .T. ) ;
#4065 = CARTESIAN_POINT ( 'NONE',  ( 28.41562500061451502, 3.027376345333611329, 5.243569643749999010 ) ) ;
#4066 = CARTESIAN_POINT ( 'NONE',  ( 8.615625000614517859, 3.027376345333611329, 5.243569643749999010 ) ) ;
#4067 = ORIENTED_EDGE ( 'NONE', *, *, #24303, .T. ) ;
#4068 = CARTESIAN_POINT ( 'NONE',  ( 23.01562500061451644, 3.027376345333611329, 5.243569643749999010 ) ) ;
#4069 = CARTESIAN_POINT ( 'NONE',  ( -2.000000000000001776, 13.19374999877096677, 33.46410161513775705 ) ) ;
#4070 = CARTESIAN_POINT ( 'NONE',  ( 11.85937500061451644, 0.000000000000000000, 4.756430356249998326 ) ) ;
#4071 = CARTESIAN_POINT ( 'NONE',  ( 0.000000000000000000, 27.50000000000000000, 26.00000000000000000 ) ) ;
#4072 = CARTESIAN_POINT ( 'NONE',  ( -3.999999999999997335, 13.85000000122903607, -27.69059892324149175 ) ) ;
#4073 = CARTESIAN_POINT ( 'NONE',  ( -3.486133158594716510E-16, 13.00624999877096855, 26.00000000000000355 ) ) ;
#4074 = CARTESIAN_POINT ( 'NONE',  ( 9.637499999999999289, 5.773502691896255534, 3.535250795749688894E-16 ) ) ;
#4075 = CARTESIAN_POINT ( 'NONE',  ( 10.69687500061451679, -3.027376345333610441, -5.243569643749999898 ) ) ;
#4076 = CARTESIAN_POINT ( 'NONE',  ( 6.000000001229033764, -2.886751345948125991, -5.000000000000000000 ) ) ;
#4077 = CARTESIAN_POINT ( 'NONE',  ( 15.38437500061451679, 4.541064518000418104, 2.621784821874999949 ) ) ;
#4078 = CARTESIAN_POINT ( 'NONE',  ( 5.184375000614516615, -4.541064518000419881, 2.621784821874995952 ) ) ;
#4079 = CARTESIAN_POINT ( 'NONE',  ( -4.243569643749997233, 9.940625000614515372, -27.54997392385601174 ) ) ;
#4080 = CARTESIAN_POINT ( 'NONE',  ( 0.000000000000000000, 20.00000000000000000, -33.99999999999999289 ) ) ;
#4081 = CARTESIAN_POINT ( 'NONE',  ( 12.23437500061451821, 4.541064518000418104, 2.621784821874999949 ) ) ;
#4082 = CARTESIAN_POINT ( 'NONE',  ( 21.90000000122903856, 5.773502691896255534, 3.535250795749688401E-16 ) ) ;
#4083 = CARTESIAN_POINT ( 'NONE',  ( 23.24062500061451786, -3.027376345333610441, -5.243569643749999898 ) ) ;
#4084 = CARTESIAN_POINT ( 'NONE',  ( -4.243569643749998122, 9.996875000614517504, 32.45002607614398471 ) ) ;
#4085 = CARTESIAN_POINT ( 'NONE',  ( -2.121784821874999949, 19.72812500061459318, 26.32496088578401938 ) ) ;
#4086 = CARTESIAN_POINT ( 'NONE',  ( 23.03437500061451715, 4.541064518000418104, 2.621784821874999949 ) ) ;
#4087 = CARTESIAN_POINT ( 'NONE',  ( 1.510657702057710734E-15, 19.43750000000000000, 26.00000000000000000 ) ) ;
#4088 = CARTESIAN_POINT ( 'NONE',  ( 4.753125000614515372, -4.541064518000417216, -2.621784821875001281 ) ) ;
#4089 = VECTOR ( 'NONE', #15173, 1000.000000000000000 ) ;
#4090 = CARTESIAN_POINT ( 'NONE',  ( 21.04687500061451644, 4.119189519843966529, -2.378215178124998275 ) ) ;
#4091 = CARTESIAN_POINT ( 'NONE',  ( 25.86562500061451431, -6.054752690667223547, -1.112240025338166033E-15 ) ) ;
#4092 = CARTESIAN_POINT ( 'NONE',  ( 17.65312500061451573, 0.000000000000000000, 5.243569643749999010 ) ) ;
#4093 = CARTESIAN_POINT ( 'NONE',  ( 14.53125000122903288, 6.123233995736764310E-16, -4.999999999999998224 ) ) ;
#4094 = CARTESIAN_POINT ( 'NONE',  ( 14.55937500061451573, 0.000000000000000000, 5.243569643749999010 ) ) ;
#4095 = CARTESIAN_POINT ( 'NONE',  ( 7.200000001229033053, -2.886751345948063374, 5.000000000000112799 ) ) ;
#4096 = CARTESIAN_POINT ( 'NONE',  ( 28.01250000122903216, -4.330127018922190985, -2.500000000000001332 ) ) ;
#4097 = CARTESIAN_POINT ( 'NONE',  ( 5.521875000614517859, 3.027376345333611329, 5.243569643749999010 ) ) ;
#4098 = VECTOR ( 'NONE', #808, 1000.000000000000000 ) ;
#4099 = CARTESIAN_POINT ( 'NONE',  ( 17.70937500061451431, 0.000000000000000000, 5.243569643749999010 ) ) ;
#4100 = CARTESIAN_POINT ( 'NONE',  ( -3.999999999999997335, 11.93750000000000000, 32.30940107675850470 ) ) ;
#4101 = CARTESIAN_POINT ( 'NONE',  ( 24.00000000000000000, 4.330127018922192761, -2.499999999999997780 ) ) ;
#4102 = ADVANCED_FACE ( 'NONE', ( #1561 ), #62510, .T. ) ;
#4103 = CARTESIAN_POINT ( 'NONE',  ( 3.450000001229036162, 5.773502691896255534, 3.535250795749688894E-16 ) ) ;
#4104 = CARTESIAN_POINT ( 'NONE',  ( 24.72187500061451360, 3.027376345333613106, -5.243569643749998122 ) ) ;
#4105 = CARTESIAN_POINT ( 'NONE',  ( 17.07187500061451502, 3.027376345333613106, -5.243569643749998122 ) ) ;
#4106 = CARTESIAN_POINT ( 'NONE',  ( -1.878215178124999163, 12.90312499938548463, 26.74683588394047007 ) ) ;
#4107 = CARTESIAN_POINT ( 'NONE',  ( 27.11249999999999716, 2.886751345948129099, -4.999999999999998224 ) ) ;
#4108 = CARTESIAN_POINT ( 'NONE',  ( 8.099999999999999645, -4.330127018922190985, -2.500000000000001332 ) ) ;
#4109 = CARTESIAN_POINT ( 'NONE',  ( 9.084375000614516082, -2.746126346562646425, 4.756430356249996549 ) ) ;
#4110 = CARTESIAN_POINT ( 'NONE',  ( 18.59062500061451573, -3.027376345333614438, 5.243569643749998122 ) ) ;
#4111 = CARTESIAN_POINT ( 'NONE',  ( 10.16249999999999964, 2.886751345948126879, 4.999999999999999112 ) ) ;
#4112 = CARTESIAN_POINT ( 'NONE',  ( 3.815625000614518036, -6.054752690667223547, -1.112240025338166033E-15 ) ) ;
#4113 = CARTESIAN_POINT ( 'NONE',  ( 20.58750000000000213, -2.886751345948129988, 4.999999999999997335 ) ) ;
#4114 = CARTESIAN_POINT ( 'NONE',  ( 9.528763966825557376E-15, 17.41249999999999787, 34.00000000000000000 ) ) ;
#4115 = CARTESIAN_POINT ( 'NONE',  ( 22.05000000122903714, -2.886751345948129988, 4.999999999999997335 ) ) ;
#4116 = DIRECTION ( 'NONE',  ( -0.000000000000000000, -1.000000000000000000, -0.000000000000000000 ) ) ;
#4117 = CARTESIAN_POINT ( 'NONE',  ( 29.14687500061451075, -3.027376345333610441, -5.243569643749999898 ) ) ;
#4118 = ORIENTED_EDGE ( 'NONE', *, *, #36651, .T. ) ;
#4119 = CARTESIAN_POINT ( 'NONE',  ( 17.31562500061451715, -6.054752690667223547, -1.112240025338166033E-15 ) ) ;
#4120 = CARTESIAN_POINT ( 'NONE',  ( 24.74062500061451786, 6.054752690667223547, 3.707466751127219781E-16 ) ) ;
#4121 = CARTESIAN_POINT ( 'NONE',  ( 24.30937500061451573, 4.541064518000418104, -2.621784821874998173 ) ) ;
#4122 = CARTESIAN_POINT ( 'NONE',  ( 10.16249999999999964, 2.886751345948126879, 4.999999999999999112 ) ) ;
#4123 = CARTESIAN_POINT ( 'NONE',  ( 11.95312500061451644, -4.541064518000417216, -2.621784821875001281 ) ) ;
#4124 = CARTESIAN_POINT ( 'NONE',  ( 27.59062500061451573, -3.027376345333614438, 5.243569643749998122 ) ) ;
#4125 = CARTESIAN_POINT ( 'NONE',  ( 13.62187500061451750, 3.027376345333611329, 5.243569643749999010 ) ) ;
#4126 = CARTESIAN_POINT ( 'NONE',  ( 20.10937500061451289, -4.541064518000417216, -2.621784821875001281 ) ) ;
#4127 = CARTESIAN_POINT ( 'NONE',  ( 3.006050052715787846, -3.995483127527877265, 3.173080537200223983 ) ) ;
#4128 = CARTESIAN_POINT ( 'NONE',  ( -4.243569643749997233, 10.44687500061451857, 32.45002607614398471 ) ) ;
#4129 = CARTESIAN_POINT ( 'NONE',  ( 22.76250000122903216, 4.330127018922192761, -2.499999999999997780 ) ) ;
#4130 = CARTESIAN_POINT ( 'NONE',  ( 17.18437500061451573, 4.119189519843966529, 2.378215178124999607 ) ) ;
#4131 = CARTESIAN_POINT ( 'NONE',  ( 14.39062500061451821, 6.054752690667223547, 3.707466751127219781E-16 ) ) ;
#4132 = CARTESIAN_POINT ( 'NONE',  ( 7.096875000614517148, -3.027376345333610441, -5.243569643749999898 ) ) ;
#4133 = CARTESIAN_POINT ( 'NONE',  ( 7.396875000614519635, -3.027376345333614438, 5.243569643749998122 ) ) ;
#4134 = EDGE_LOOP ( 'NONE', ( #10893, #69862, #12720, #34518 ) ) ;
#4135 = CARTESIAN_POINT ( 'NONE',  ( 27.19687500061451857, -3.027376345333614438, 5.243569643749998122 ) ) ;
#4136 = CARTESIAN_POINT ( 'NONE',  ( 20.12812500061451715, 6.421520780324663323E-16, -5.243569643749999010 ) ) ;
#4137 = CARTESIAN_POINT ( 'NONE',  ( 23.63437500061451502, -4.541064518000419881, 2.621784821874995952 ) ) ;
#4138 = CARTESIAN_POINT ( 'NONE',  ( 19.41562500061451146, 3.027376345333611329, 5.243569643749999010 ) ) ;
#4139 = CARTESIAN_POINT ( 'NONE',  ( 3.999999999999999112, 12.57500000000000107, 30.00000000000000000 ) ) ;
#4140 = CARTESIAN_POINT ( 'NONE',  ( 25.86562500061451431, -6.054752690667223547, -1.112240025338166033E-15 ) ) ;
#4141 = CARTESIAN_POINT ( 'NONE',  ( 7.762500001229033053, -4.330127018922190985, -2.500000000000001332 ) ) ;
#4142 = ORIENTED_EDGE ( 'NONE', *, *, #19175, .F. ) ;
#4143 = CARTESIAN_POINT ( 'NONE',  ( 2.962500001229034119, 4.330127018922192761, -2.499999999999997780 ) ) ;
#4144 = CARTESIAN_POINT ( 'NONE',  ( 3.999999999999999112, 16.62500000000000000, -30.00000000000000000 ) ) ;
#4145 = CARTESIAN_POINT ( 'NONE',  ( 23.51250000122903216, -4.330127018922190985, -2.500000000000001332 ) ) ;
#4146 = CARTESIAN_POINT ( 'NONE',  ( 3.756430356249998770, 14.96562499938548108, 32.16877607737302469 ) ) ;
#4147 = CARTESIAN_POINT ( 'NONE',  ( 3.796875000614517326, -3.027376345333614438, 5.243569643749998122 ) ) ;
#4148 = LINE ( 'NONE', #53275, #62074 ) ;
#4149 = CARTESIAN_POINT ( 'NONE',  ( 13.26562500061451644, -6.054752690667223547, -1.112240025338166033E-15 ) ) ;
#4150 = CARTESIAN_POINT ( 'NONE',  ( 9.046875000614518214, 6.054752690667223547, 3.707466751127219781E-16 ) ) ;
#4151 = CARTESIAN_POINT ( 'NONE',  ( 23.96250000122903145, -4.330127018922190985, -2.500000000000001332 ) ) ;
#4152 = CARTESIAN_POINT ( 'NONE',  ( 14.55937500061451573, 0.000000000000000000, 5.243569643749999010 ) ) ;
#4153 = CARTESIAN_POINT ( 'NONE',  ( 5.109375000614518214, 0.000000000000000000, 5.243569643749999010 ) ) ;
#4154 = CARTESIAN_POINT ( 'NONE',  ( 29.66249999999999432, -5.773502691896255534, -1.060575238724906372E-15 ) ) ;
#4155 = CARTESIAN_POINT ( 'NONE',  ( 5.690625000614516260, -3.027376345333610441, -5.243569643749999898 ) ) ;
#4156 = CARTESIAN_POINT ( 'NONE',  ( 15.74062500061451608, 6.054752690667223547, 3.707466751127219781E-16 ) ) ;
#4157 = EDGE_CURVE ( 'NONE', #64403, #12255, #28810, .T. ) ;
#4158 = VERTEX_POINT ( 'NONE', #17790 ) ;
#4159 = AXIS2_PLACEMENT_3D ( 'NONE', #29800, #57509, #6911 ) ;
#4160 = CARTESIAN_POINT ( 'NONE',  ( 12.59062500061451573, 6.054752690667223547, 3.707466751127219781E-16 ) ) ;
#4161 = CARTESIAN_POINT ( 'NONE',  ( 8.540625000614518569, 6.054752690667223547, 3.707466751127219781E-16 ) ) ;
#4162 = CARTESIAN_POINT ( 'NONE',  ( 20.52187500061451786, -5.492252693125287522, -1.008910452111647106E-15 ) ) ;
#4163 = CARTESIAN_POINT ( 'NONE',  ( 8.250000000000000000, 4.330127018922192761, -2.499999999999997780 ) ) ;
#4164 = CARTESIAN_POINT ( 'NONE',  ( 4.987500001229032698, -4.330127018922194537, 2.499999999999995559 ) ) ;
#4165 = CARTESIAN_POINT ( 'NONE',  ( 18.86249999999999716, -5.773502691896255534, -1.060575238724906372E-15 ) ) ;
#4166 =( BOUNDED_CURVE ( )  B_SPLINE_CURVE ( 2, ( #7490, #48116, #41477, #1967, #2680, #65095, #41124, #47741, #47382 ),
 .UNSPECIFIED., .F., .F. ) 
 B_SPLINE_CURVE_WITH_KNOTS ( ( 3, 2, 2, 2, 3 ),
 ( 0.3152173913043478382, 0.3188405797101449002, 0.3260869565217391353, 0.3333333333333333148, 0.3369565217391304324 ),
 .UNSPECIFIED. ) 
 CURVE ( )  GEOMETRIC_REPRESENTATION_ITEM ( )  RATIONAL_B_SPLINE_CURVE ( ( 0.9330127018922194093, 0.9330127018922198534, 1.000000000000000000, 0.8660254037844387076, 1.000000000000000000, 0.8660254037844387076, 1.000000000000000000, 0.9330127018922194093, 0.9330127018922194093 ) ) 
 REPRESENTATION_ITEM ( '' )  );
#4167 = CARTESIAN_POINT ( 'NONE',  ( 18.19687500061451502, -3.027376345333614438, 5.243569643749998122 ) ) ;
#4168 = CARTESIAN_POINT ( 'NONE',  ( 14.13750000122903394, 6.123233995736764310E-16, -4.999999999999998224 ) ) ;
#4169 = CARTESIAN_POINT ( 'NONE',  ( 23.25000000000000000, 0.000000000000000000, 4.999999999999998224 ) ) ;
#4170 = CARTESIAN_POINT ( 'NONE',  ( -4.243569643749999898, 17.06562500061451360, -32.45002607614398471 ) ) ;
#4171 = CARTESIAN_POINT ( 'NONE',  ( 5.810221930991193690E-16, 19.81250000000000000, 26.00000000000000000 ) ) ;
#4172 = CARTESIAN_POINT ( 'NONE',  ( 18.43125000122903501, -4.330127018922194537, 2.499999999999995559 ) ) ;
#4173 = CARTESIAN_POINT ( 'NONE',  ( 28.97812500061451502, -4.541064518000419881, 2.621784821874995952 ) ) ;
#4174 = CYLINDRICAL_SURFACE ( 'NONE', #72883, 4.999999999999998224 ) ;
#4175 = CARTESIAN_POINT ( 'NONE',  ( 24.22500000000000142, -4.330127018922194537, 2.499999999999995559 ) ) ;
#4176 = CARTESIAN_POINT ( 'NONE',  ( 14.52187500061451608, 3.027376345333611329, 5.243569643749999010 ) ) ;
#4177 = CARTESIAN_POINT ( 'NONE',  ( 26.28749999999999432, 5.773502691896255534, 3.535250795749688894E-16 ) ) ;
#4178 = CARTESIAN_POINT ( 'NONE',  ( 11.35312500061451679, 0.000000000000000000, 5.243569643749999010 ) ) ;
#4179 = CARTESIAN_POINT ( 'NONE',  ( 26.74687500061451573, -4.119189519843965641, -2.378215178125001383 ) ) ;
#4180 = CARTESIAN_POINT ( 'NONE',  ( 22.02187500061452141, 3.027376345333613106, -5.243569643749998122 ) ) ;
#4181 = CARTESIAN_POINT ( 'NONE',  ( 13.39687500061451431, 4.119189519843966529, -2.378215178124998275 ) ) ;
#4182 = AXIS2_PLACEMENT_3D ( 'NONE', #27291, #44290, #37997 ) ;
#4183 = CARTESIAN_POINT ( 'NONE',  ( 7.903125000614515727, -4.541064518000417216, -2.621784821875001281 ) ) ;
#4184 = CARTESIAN_POINT ( 'NONE',  ( 13.43437500061451750, 6.421520780324663323E-16, -5.243569643749999010 ) ) ;
#4185 = ORIENTED_EDGE ( 'NONE', *, *, #42052, .F. ) ;
#4186 = CARTESIAN_POINT ( 'NONE',  ( 23.48437500061451644, 4.541064518000418104, 2.621784821874999949 ) ) ;
#4187 = CARTESIAN_POINT ( 'NONE',  ( 2.485350534231660191, 4.344988454211105022, -26.85539458128546286 ) ) ;
#4188 = CARTESIAN_POINT ( 'NONE',  ( 7.320879633048903241E-15, 17.30000000122903003, 26.00000000000000355 ) ) ;
#4189 = CARTESIAN_POINT ( 'NONE',  ( 4.837500000000001243, -2.886751345948129988, 4.999999999999997335 ) ) ;
#4190 = CARTESIAN_POINT ( 'NONE',  ( 16.50000000122903288, 5.773502691896255534, 3.535250795749688894E-16 ) ) ;
#4191 = CARTESIAN_POINT ( 'NONE',  ( -1.071796769724487453, 17.77009619066136636, -34.00000000000000000 ) ) ;
#4192 = CARTESIAN_POINT ( 'NONE',  ( 8.934375000614515727, 5.492252693125287522, 3.363034840372157021E-16 ) ) ;
#4193 = ORIENTED_EDGE ( 'NONE', *, *, #3893, .F. ) ;
#4194 = CARTESIAN_POINT ( 'NONE',  ( 14.24999999999999822, 0.000000000000000000, 4.999999999999998224 ) ) ;
#4195 = CARTESIAN_POINT ( 'NONE',  ( 16.35000000000000142, 4.330127018922192761, -2.499999999999997780 ) ) ;
#4196 = CARTESIAN_POINT ( 'NONE',  ( 11.87812500061451537, -4.541064518000419881, 2.621784821874995952 ) ) ;
#4198 = ORIENTED_EDGE ( 'NONE', *, *, #50924, .F. ) ;
#4197 = AXIS2_PLACEMENT_3D ( 'NONE', #19143, #47604, #46158 ) ;
#4199 = CARTESIAN_POINT ( 'NONE',  ( -3.999999999999999112, 15.57500000122903216, 27.69059892324149885 ) ) ;
#4200 = CARTESIAN_POINT ( 'NONE',  ( -4.243569643749997233, 16.29687500061451644, -27.54997392385601174 ) ) ;
#4201 = CARTESIAN_POINT ( 'NONE',  ( 29.40000000122903145, -2.886751345948125991, -5.000000000000000000 ) ) ;
#4202 = CARTESIAN_POINT ( 'NONE',  ( -1.878215178125001827, 14.29062499938548392, 33.25316411605952283 ) ) ;
#4203 = CARTESIAN_POINT ( 'NONE',  ( 9.449999999999999289, -4.330127018922190985, -2.500000000000001332 ) ) ;
#4204 = CARTESIAN_POINT ( 'NONE',  ( 16.33125000122903359, 6.123233995736764310E-16, -4.999999999999998224 ) ) ;
#4205 = ORIENTED_EDGE ( 'NONE', *, *, #49986, .F. ) ;
#4206 = CARTESIAN_POINT ( 'NONE',  ( -4.243569643749999898, 12.56562500061451715, 27.54997392385601529 ) ) ;
#4207 = CARTESIAN_POINT ( 'NONE',  ( 25.00312500061451715, -4.541064518000417216, -2.621784821875001281 ) ) ;
#4208 = CARTESIAN_POINT ( 'NONE',  ( 3.651773823418189124, 3.415340091791402966, 3.978752903393068863 ) ) ;
#4209 = CARTESIAN_POINT ( 'NONE',  ( -3.756430356250001434, 19.20312499938548356, 32.16877607737301048 ) ) ;
#4210 = CARTESIAN_POINT ( 'NONE',  ( 20.59687500061451360, -3.027376345333610441, -5.243569643749999898 ) ) ;
#4211 = CARTESIAN_POINT ( 'NONE',  ( 20.24062500061451431, 6.054752690667223547, 3.707466751127219781E-16 ) ) ;
#4212 = CARTESIAN_POINT ( 'NONE',  ( 2.121784821874999061, 15.15312500061459566, -33.67503911421598417 ) ) ;
#4213 = CARTESIAN_POINT ( 'NONE',  ( 22.53750000122903430, -4.330127018922194537, 2.499999999999995559 ) ) ;
#4214 =( BOUNDED_CURVE ( )  B_SPLINE_CURVE ( 2, ( #3805, #31505, #3441, #25960, #71025, #42951, #65479 ),
 .UNSPECIFIED., .F., .F. ) 
 B_SPLINE_CURVE_WITH_KNOTS ( ( 3, 2, 2, 3 ),
 ( 0.9942380576293760042, 0.9944444444444444642, 0.9972222222222222321, 0.9973736731814578649 ),
 .UNSPECIFIED. ) 
 CURVE ( )  GEOMETRIC_REPRESENTATION_ITEM ( )  RATIONAL_B_SPLINE_CURVE ( ( 0.9815707561575266471, 0.9900457875233154015, 1.000000000000000000, 0.8660254037844387076, 1.000000000000000000, 0.9926953908003807170, 0.9861873104512506316 ) ) 
 REPRESENTATION_ITEM ( '' )  );
#4215 = CARTESIAN_POINT ( 'NONE',  ( 4.190625000614518925, -3.027376345333614438, 5.243569643749998122 ) ) ;
#4216 = CARTESIAN_POINT ( 'NONE',  ( 23.22187500061451715, -5.492252693125287522, -1.008910452111647106E-15 ) ) ;
#4217 = CARTESIAN_POINT ( 'NONE',  ( 22.67812500061451431, -4.541064518000419881, 2.621784821874995952 ) ) ;
#4218 = CARTESIAN_POINT ( 'NONE',  ( 8.784375000614518925, -4.119189519843968306, 2.378215178124996054 ) ) ;
#4219 = CARTESIAN_POINT ( 'NONE',  ( -1.878215178125001827, 19.24062499938548143, 33.25316411605952283 ) ) ;
#4220 = CARTESIAN_POINT ( 'NONE',  ( 15.79687500061451821, 6.054752690667223547, 3.707466751127219781E-16 ) ) ;
#4221 = CARTESIAN_POINT ( 'NONE',  ( 14.89687500061451786, 6.054752690667223547, 3.707466751127219781E-16 ) ) ;
#4222 = CARTESIAN_POINT ( 'NONE',  ( 21.98437500061451644, 6.421520780324663323E-16, -5.243569643749999010 ) ) ;
#4223 = CARTESIAN_POINT ( 'NONE',  ( 2.121784821875001281, 12.80937500061451928, 33.67503911421598417 ) ) ;
#4224 = CARTESIAN_POINT ( 'NONE',  ( 4.303125000614516971, -4.541064518000417216, -2.621784821875001281 ) ) ;
#4226 =( BOUNDED_CURVE ( )  B_SPLINE_CURVE ( 2, ( #60031, #71128, #20501, #43058, #44537, #65583, #14973, #9443, #31971 ),
 .UNSPECIFIED., .F., .F. ) 
 B_SPLINE_CURVE_WITH_KNOTS ( ( 3, 2, 2, 2, 3 ),
 ( 0.9583333333333333703, 0.9629629629629629095, 0.9722222222222222099, 0.9814814814814815103, 0.9861111111111111605 ),
 .UNSPECIFIED. ) 
 CURVE ( )  GEOMETRIC_REPRESENTATION_ITEM ( )  RATIONAL_B_SPLINE_CURVE ( ( 0.9330127018922192983, 0.9330127018922200755, 1.000000000000000000, 0.8660254037844387076, 1.000000000000000000, 0.8660254037844387076, 1.000000000000000000, 0.9330127018922186322, 0.9330127018922194093 ) ) 
 REPRESENTATION_ITEM ( '' )  );
#4225 = CARTESIAN_POINT ( 'NONE',  ( 25.41562500061451146, -6.054752690667223547, -1.112240025338166033E-15 ) ) ;
#4227 = ADVANCED_FACE ( 'NONE', ( #45896 ), #6365, .F. ) ;
#4228 = CARTESIAN_POINT ( 'NONE',  ( 26.01562500061451289, 3.027376345333613106, -5.243569643749998122 ) ) ;
#4229 = LINE ( 'NONE', #20454, #24997 ) ;
#4230 = CARTESIAN_POINT ( 'NONE',  ( -3.999999999999997335, 18.23750000000000071, 32.30940107675850470 ) ) ;
#4231 = CARTESIAN_POINT ( 'NONE',  ( 7.059375000614518392, -4.541064518000417216, -2.621784821875001281 ) ) ;
#4232 = PRODUCT_CONTEXT ( 'NONE', #25218, 'mechanical' ) ;
#4233 = CARTESIAN_POINT ( 'NONE',  ( 13.91250000122903252, 0.000000000000000000, 4.999999999999998224 ) ) ;
#4234 = CARTESIAN_POINT ( 'NONE',  ( 8.362500001229031810, 4.330127018922192761, -2.499999999999997780 ) ) ;
#4235 = CARTESIAN_POINT ( 'NONE',  ( 29.06250000122903288, 4.330127018922192761, -2.499999999999997780 ) ) ;
#4236 = CARTESIAN_POINT ( 'NONE',  ( -1.999999999999999112, 16.19374999877096499, 26.53589838486224650 ) ) ;
#4237 = CARTESIAN_POINT ( 'NONE',  ( 18.65625000122902932, 4.330127018922192761, -2.499999999999997780 ) ) ;
#4238 = CARTESIAN_POINT ( 'NONE',  ( 14.85937500061451644, 4.541064518000418104, -2.621784821874998173 ) ) ;
#4239 = DIRECTION ( 'NONE',  ( 0.000000000000000000, 0.000000000000000000, 1.000000000000000000 ) ) ;
#4240 = VERTEX_POINT ( 'NONE', #46616 ) ;
#4241 = CARTESIAN_POINT ( 'NONE',  ( 18.81562500061452070, 3.027376345333613106, -5.243569643749998122 ) ) ;
#4242 = CARTESIAN_POINT ( 'NONE',  ( 6.515625000614516438, -6.054752690667223547, -1.112240025338166033E-15 ) ) ;
#4243 = CARTESIAN_POINT ( 'NONE',  ( 21.53437500061451715, 6.421520780324663323E-16, -5.243569643749999010 ) ) ;
#4244 = CARTESIAN_POINT ( 'NONE',  ( 5.840625000614516615, 6.054752690667223547, 3.707466751127219781E-16 ) ) ;
#4245 = CARTESIAN_POINT ( 'NONE',  ( 45.00000000000000000, -8.874999999999998224, -1.494782592887687667 ) ) ;
#4246 = CARTESIAN_POINT ( 'NONE',  ( 7.762500001229033053, -4.330127018922190985, -2.500000000000001332 ) ) ;
#4247 = CARTESIAN_POINT ( 'NONE',  ( 22.00312500061451360, 4.541064518000418104, -2.621784821874998173 ) ) ;
#4248 = EDGE_CURVE ( 'NONE', #28698, #19531, #36365, .T. ) ;
#4249 =( BOUNDED_CURVE ( )  B_SPLINE_CURVE ( 2, ( #54139, #36409, #3902, #3533, #26056, #58561, #37503, #58923, #60023 ),
 .UNSPECIFIED., .F., .T. ) 
 B_SPLINE_CURVE_WITH_KNOTS ( ( 3, 2, 2, 2, 3 ),
 ( 0.5978260869565217295, 0.6014492753623188470, 0.6086956521739130821, 0.6159420289855072062, 0.6195652173913043237 ),
 .UNSPECIFIED. ) 
 CURVE ( )  GEOMETRIC_REPRESENTATION_ITEM ( )  RATIONAL_B_SPLINE_CURVE ( ( 0.9330127018922194093, 0.9330127018922194093, 1.000000000000000000, 0.8660254037844387076, 1.000000000000000000, 0.8660254037844387076, 1.000000000000000000, 0.9330127018922194093, 0.9330127018922194093 ) ) 
 REPRESENTATION_ITEM ( '' )  );
#4250 = CARTESIAN_POINT ( 'NONE',  ( -3.999999999999997335, 17.45000000122903216, -27.69059892324149175 ) ) ;
#4251 = CARTESIAN_POINT ( 'NONE',  ( 11.25000000122903288, -2.886751345948129988, 4.999999999999997335 ) ) ;
#4252 = CARTESIAN_POINT ( 'NONE',  ( 18.96562500061451573, 3.027376345333611329, 5.243569643749999010 ) ) ;
#4253 = CARTESIAN_POINT ( 'NONE',  ( 16.34062500061451573, -3.027376345333614438, 5.243569643749998122 ) ) ;
#4254 = CARTESIAN_POINT ( 'NONE',  ( 28.99687500061451573, -2.746126346562646425, 4.756430356249996549 ) ) ;
#4255 = CARTESIAN_POINT ( 'NONE',  ( 15.78749999999999964, -2.886751345948125991, -5.000000000000000000 ) ) ;
#4256 = CARTESIAN_POINT ( 'NONE',  ( 12.33750000122903145, 6.123233995736764310E-16, -4.999999999999998224 ) ) ;
#4257 = CARTESIAN_POINT ( 'NONE',  ( 7.940625000614518036, -3.027376345333610441, -5.243569643749999898 ) ) ;
#4258 = CARTESIAN_POINT ( 'NONE',  ( 11.99062500061451608, -3.027376345333610441, -5.243569643749999898 ) ) ;
#4259 = ADVANCED_FACE ( 'NONE', ( #62155 ), #12265, .T. ) ;
#4260 = CARTESIAN_POINT ( 'NONE',  ( 21.30000000122903359, -2.886751345948125991, -5.000000000000000000 ) ) ;
#4261 = AXIS2_PLACEMENT_3D ( 'NONE', #52143, #28882, #11894 ) ;
#4262 = CARTESIAN_POINT ( 'NONE',  ( 20.59687500061451360, -3.027376345333610441, -5.243569643749999898 ) ) ;
#4263 = CARTESIAN_POINT ( 'NONE',  ( 24.97499999999999787, 4.330127018922191873, 2.499999999999999556 ) ) ;
#4264 = CARTESIAN_POINT ( 'NONE',  ( 5.512500001229033941, -4.330127018922190985, -2.500000000000001332 ) ) ;
#4265 = CARTESIAN_POINT ( 'NONE',  ( 5.146875000614517859, -3.027376345333614438, 5.243569643749998122 ) ) ;
#4266 = CARTESIAN_POINT ( 'NONE',  ( 23.37187500061451573, 3.027376345333613106, -5.243569643749998122 ) ) ;
#4267 = CARTESIAN_POINT ( 'NONE',  ( 1.071796769724491893, 18.44509619066136707, 33.99999999999999289 ) ) ;
#4268 = CARTESIAN_POINT ( 'NONE',  ( 18.59062500061451573, -3.027376345333614438, 5.243569643749998122 ) ) ;
#4269 = CARTESIAN_POINT ( 'NONE',  ( 23.97187500061451360, 3.027376345333611329, 5.243569643749999010 ) ) ;
#4270 = CARTESIAN_POINT ( 'NONE',  ( -7.967954043666661671E-16, 18.94062499938548427, 34.33755215474603517 ) ) ;
#4271 = CARTESIAN_POINT ( 'NONE',  ( -1.999999999999999112, 14.45000000000000107, 26.53589838486224650 ) ) ;
#4272 = CARTESIAN_POINT ( 'NONE',  ( 28.50937500061451502, 0.000000000000000000, 5.243569643749999010 ) ) ;
#4273 = CARTESIAN_POINT ( 'NONE',  ( 21.23437500061451644, -2.746126346562646425, 4.756430356249996549 ) ) ;
#4274 = CARTESIAN_POINT ( 'NONE',  ( 14.24062500061451608, -3.027376345333610441, -5.243569643749999898 ) ) ;
#4275 = CARTESIAN_POINT ( 'NONE',  ( 12.23437500061451821, 4.541064518000418104, 2.621784821874999949 ) ) ;
#4276 = ORIENTED_EDGE ( 'NONE', *, *, #28806, .T. ) ;
#4277 = CARTESIAN_POINT ( 'NONE',  ( 22.71562500061451573, -6.054752690667223547, -1.112240025338166033E-15 ) ) ;
#4278 = CARTESIAN_POINT ( 'NONE',  ( 3.413604573517995622, 3.653464791278348667, -3.457471840445726752 ) ) ;
#4279 = CARTESIAN_POINT ( 'NONE',  ( 13.87500000000000178, -4.330127018922194537, 2.499999999999995559 ) ) ;
#4280 = CARTESIAN_POINT ( 'NONE',  ( 23.21250000122903501, 4.330127018922192761, -2.499999999999997780 ) ) ;
#4281 = CARTESIAN_POINT ( 'NONE',  ( 19.67812500061451786, 6.421520780324663323E-16, -5.243569643749999010 ) ) ;
#4282 = VERTEX_POINT ( 'NONE', #62869 ) ;
#4283 = CARTESIAN_POINT ( 'NONE',  ( 22.31250000000000000, 2.886751345948126879, 4.999999999999999112 ) ) ;
#4284 = EDGE_CURVE ( 'NONE', #4034, #40431, #7092, .T. ) ;
#4285 = CARTESIAN_POINT ( 'NONE',  ( 22.95937500061451431, 4.541064518000418104, -2.621784821874998173 ) ) ;
#4286 = EDGE_LOOP ( 'NONE', ( #45626, #43800, #7187, #7569 ) ) ;
#4287 = CARTESIAN_POINT ( 'NONE',  ( 3.999999999999998668, 19.21250000000000213, 32.30940107675850470 ) ) ;
#4288 = CARTESIAN_POINT ( 'NONE',  ( 9.965625000614517504, 3.027376345333611329, 5.243569643749999010 ) ) ;
#4289 = LINE ( 'NONE', #47882, #49075 ) ;
#4290 = CARTESIAN_POINT ( 'NONE',  ( 15.23437500061451644, 5.492252693125287522, 3.363034840372157021E-16 ) ) ;
#4291 = CARTESIAN_POINT ( 'NONE',  ( 26.61562500061451786, 3.027376345333611329, 5.243569643749999010 ) ) ;
#4292 = AXIS2_PLACEMENT_3D ( 'NONE', #32297, #36736, #4239 ) ;
#4293 = CARTESIAN_POINT ( 'NONE',  ( 16.19999999999999929, -4.330127018922190985, -2.500000000000001332 ) ) ;
#4294 = CARTESIAN_POINT ( 'NONE',  ( 23.58749999999999858, 5.773502691896255534, 3.535250795749688894E-16 ) ) ;
#4295 = DIRECTION ( 'NONE',  ( -1.000000000000000000, -0.000000000000000000, -0.000000000000000000 ) ) ;
#4296 = CARTESIAN_POINT ( 'NONE',  ( 7.696875000614516793, 6.054752690667223547, 3.707466751127219781E-16 ) ) ;
#4297 = CARTESIAN_POINT ( 'NONE',  ( 17.63437500061451502, 4.541064518000418104, 2.621784821874999949 ) ) ;
#4298 = CARTESIAN_POINT ( 'NONE',  ( 29.48437500061451644, -4.541064518000419881, 2.621784821874995952 ) ) ;
#4299 = ORIENTED_EDGE ( 'NONE', *, *, #54732, .F. ) ;
#4300 = CARTESIAN_POINT ( 'NONE',  ( 26.01562500061451289, 3.027376345333613106, -5.243569643749998122 ) ) ;
#4301 = CARTESIAN_POINT ( 'NONE',  ( 28.73437500061451644, 6.421520780324663323E-16, -5.243569643749999010 ) ) ;
#4302 = CARTESIAN_POINT ( 'NONE',  ( 30.00000000000000000, 6.123233995736764310E-16, -4.999999999999998224 ) ) ;
#4303 = CARTESIAN_POINT ( 'NONE',  ( 12.97499999999999964, -4.330127018922194537, 2.499999999999995559 ) ) ;
#4304 = CARTESIAN_POINT ( 'NONE',  ( 11.80312500061451608, 0.000000000000000000, 5.243569643749999010 ) ) ;
#4305 = LINE ( 'NONE', #16094, #27556 ) ;
#4306 = LINE ( 'NONE', #9831, #25391 ) ;
#4307 = CARTESIAN_POINT ( 'NONE',  ( 28.19062500061451715, -3.027376345333610441, -5.243569643749999898 ) ) ;
#4308 = CARTESIAN_POINT ( 'NONE',  ( 16.27500000122903501, -5.773502691896255534, -1.060575238724906372E-15 ) ) ;
#4309 = CARTESIAN_POINT ( 'NONE',  ( 27.13125000122903430, 6.123233995736764310E-16, -4.999999999999998224 ) ) ;
#4310 = CARTESIAN_POINT ( 'NONE',  ( 14.82187500061451679, 2.746126346562645981, -4.756430356249997438 ) ) ;
#4311 = CARTESIAN_POINT ( 'NONE',  ( 5.503125000614516260, 0.000000000000000000, 5.243569643749999010 ) ) ;
#4312 = CARTESIAN_POINT ( 'NONE',  ( 21.75937500061451502, 0.000000000000000000, 5.243569643749999010 ) ) ;
#4313 = CARTESIAN_POINT ( 'NONE',  ( -4.243569643749999898, 16.67187500061451644, 27.54997392385601529 ) ) ;
#4314 = CARTESIAN_POINT ( 'NONE',  ( 20.59687500061451360, -3.027376345333610441, -5.243569643749999898 ) ) ;
#4315 = CARTESIAN_POINT ( 'NONE',  ( 28.88437500061451502, 4.541064518000418104, 2.621784821874999949 ) ) ;
#4316 = CARTESIAN_POINT ( 'NONE',  ( -2.121784821874996840, 18.13437500061451502, 33.67503911421598417 ) ) ;
#4317 = CARTESIAN_POINT ( 'NONE',  ( 13.30312500061451786, -4.541064518000417216, -2.621784821875001281 ) ) ;
#4318 = CARTESIAN_POINT ( 'NONE',  ( 5.025000001229035895, -5.773502691896255534, -1.060575238724906372E-15 ) ) ;
#4319 = PRODUCT_DEFINITION_SHAPE ( 'NONE', 'NONE',  #73120 ) ;
#4320 = CARTESIAN_POINT ( 'NONE',  ( 7.584375000614516082, 6.421520780324663323E-16, -5.243569643749999010 ) ) ;
#4321 = CARTESIAN_POINT ( 'NONE',  ( 3.897990869167640149, 3.131492215201401308, -4.036780346077406989 ) ) ;
#4322 = CARTESIAN_POINT ( 'NONE',  ( 8.990625000614516082, 6.054752690667223547, 3.707466751127219781E-16 ) ) ;
#4323 = CARTESIAN_POINT ( 'NONE',  ( 13.69687500061451679, -3.027376345333614438, 5.243569643749998122 ) ) ;
#4324 = DIRECTION ( 'NONE',  ( 1.000000000000000000, 0.000000000000000000, 0.000000000000000000 ) ) ;
#4325 = CARTESIAN_POINT ( 'NONE',  ( 22.05000000122903714, -2.886751345948129988, 4.999999999999997335 ) ) ;
#4326 = CARTESIAN_POINT ( 'NONE',  ( 7.209375000614519635, 4.541064518000418104, -2.621784821874998173 ) ) ;
#4327 = CARTESIAN_POINT ( 'NONE',  ( 12.89062500061451821, -3.027376345333610441, -5.243569643749999898 ) ) ;
#4328 = ADVANCED_FACE ( 'NONE', ( #6732 ), #18150, .F. ) ;
#4329 = CARTESIAN_POINT ( 'NONE',  ( 25.44375000122903074, 5.773502691896255534, 3.535250795749688894E-16 ) ) ;
#4330 = CARTESIAN_POINT ( 'NONE',  ( 21.42187500061451644, -6.054752690667223547, -1.112240025338166033E-15 ) ) ;
#4331 = CARTESIAN_POINT ( 'NONE',  ( 1.592000809091587073E-14, 16.73750000000000071, 26.00000000000000000 ) ) ;
#4332 = CARTESIAN_POINT ( 'NONE',  ( -3.943440097865042571, 3.074283834720754172, 29.31637382434952954 ) ) ;
#4333 = CARTESIAN_POINT ( 'NONE',  ( 3.261697542054055710, 3.789670288106804730, -3.327321037948185012 ) ) ;
#4334 = CARTESIAN_POINT ( 'NONE',  ( -2.121784821874999949, 11.23437500061451821, -33.67503911421598417 ) ) ;
#4335 = CARTESIAN_POINT ( 'NONE',  ( 14.47500000122903430, -5.773502691896255534, -1.060575238724906372E-15 ) ) ;
#4336 = CARTESIAN_POINT ( 'NONE',  ( -2.121784821874996840, 16.27812500061451573, -26.32496088578401583 ) ) ;
#4337 = CARTESIAN_POINT ( 'NONE',  ( 16.95000000122903216, 5.773502691896255534, 3.535250795749688894E-16 ) ) ;
#4338 = CARTESIAN_POINT ( 'NONE',  ( 10.41562500061451679, 3.027376345333611329, 5.243569643749999010 ) ) ;
#4339 = EDGE_LOOP ( 'NONE', ( #44542, #11640, #13920, #65373 ) ) ;
#4340 = CARTESIAN_POINT ( 'NONE',  ( 14.10000000000000142, 4.330127018922192761, -2.499999999999997780 ) ) ;
#4341 = AXIS2_PLACEMENT_3D ( 'NONE', #21026, #14391, #60545 ) ;
#4342 = CARTESIAN_POINT ( 'NONE',  ( 23.42812500061451786, 4.541064518000418104, 2.621784821874999949 ) ) ;
#4343 = CARTESIAN_POINT ( 'NONE',  ( 11.29687500061451644, 6.054752690667223547, 3.707466751127219781E-16 ) ) ;
#4344 = CARTESIAN_POINT ( 'NONE',  ( 1.071796769724479237, 17.03615380933862866, 25.99999999999999645 ) ) ;
#4345 = CARTESIAN_POINT ( 'NONE',  ( 10.16250000122903252, 4.330127018922192761, -2.499999999999997780 ) ) ;
#4346 = CARTESIAN_POINT ( 'NONE',  ( 19.72500000122903074, 2.886751345948126879, 4.999999999999999112 ) ) ;
#4347 = CARTESIAN_POINT ( 'NONE',  ( 15.10312500061451502, -4.541064518000417216, -2.621784821875001281 ) ) ;
#4348 = CARTESIAN_POINT ( 'NONE',  ( 18.32812500061451644, 6.421520780324663323E-16, -5.243569643749999010 ) ) ;
#4349 = CARTESIAN_POINT ( 'NONE',  ( 25.57500000122903216, 2.886751345948126879, 4.999999999999999112 ) ) ;
#4350 = CARTESIAN_POINT ( 'NONE',  ( 4.415625000614518569, 3.027376345333613106, -5.243569643749998122 ) ) ;
#4351 = CARTESIAN_POINT ( 'NONE',  ( 26.17500000000000071, 6.123233995736764310E-16, -4.999999999999998224 ) ) ;
#4352 = CARTESIAN_POINT ( 'NONE',  ( 2.655984681222220721E-16, 14.55312499938548321, 25.66244784525396483 ) ) ;
#4353 = AXIS2_PLACEMENT_3D ( 'NONE', #28850, #34747, #68384 ) ;
#4354 = CARTESIAN_POINT ( 'NONE',  ( 25.54687500061451644, -3.027376345333610441, -5.243569643749999898 ) ) ;
#4355 = CARTESIAN_POINT ( 'NONE',  ( 9.528763966825557376E-15, 17.41249999999999787, 34.00000000000000000 ) ) ;
#4356 = CARTESIAN_POINT ( 'NONE',  ( 13.31250000122903288, 4.330127018922192761, -2.499999999999997780 ) ) ;
#4357 = CARTESIAN_POINT ( 'NONE',  ( 29.59687500061451715, -3.027376345333610441, -5.243569643749999898 ) ) ;
#4358 = CARTESIAN_POINT ( 'NONE',  ( 5.810221930991193690E-16, 18.40624999877096357, 26.00000000000000000 ) ) ;
#4359 = CARTESIAN_POINT ( 'NONE',  ( 6.271875000614517859, 3.027376345333613106, -5.243569643749998122 ) ) ;
#4360 = CARTESIAN_POINT ( 'NONE',  ( 26.57812500061451644, 4.541064518000418104, 2.621784821874999949 ) ) ;
#4361 = CARTESIAN_POINT ( 'NONE',  ( 3.756430356250000546, 12.79062499938548214, 27.83122392262697886 ) ) ;
#4362 = CARTESIAN_POINT ( 'NONE',  ( 1.626862140677534273E-15, 10.32500000122903572, 34.00000000000000000 ) ) ;
#4363 = CARTESIAN_POINT ( 'NONE',  ( 4.340613942912554535, -2.482170104787147835, 4.431799429985763261 ) ) ;
#4364 = CARTESIAN_POINT ( 'NONE',  ( 4.396875000614516971, -3.027376345333610441, -5.243569643749999898 ) ) ;
#4365 = CARTESIAN_POINT ( 'NONE',  ( 9.009375000614518569, 4.541064518000418104, -2.621784821874998173 ) ) ;
#4366 = CARTESIAN_POINT ( 'NONE',  ( 28.99687500061451573, -3.027376345333614438, 5.243569643749998122 ) ) ;
#4367 = CARTESIAN_POINT ( 'NONE',  ( 4.243569643749999898, 13.24062500061459602, 32.45002607614398471 ) ) ;
#4368 = CARTESIAN_POINT ( 'NONE',  ( 21.41250000000000497, 2.886751345948126879, 4.999999999999999112 ) ) ;
#4369 = ORIENTED_EDGE ( 'NONE', *, *, #57401, .T. ) ;
#4370 = CARTESIAN_POINT ( 'NONE',  ( -2.672702088255949472E-15, 13.51250000000000107, 26.00000000000000000 ) ) ;
#4371 = CARTESIAN_POINT ( 'NONE',  ( 4.087500000000001243, -2.886751345948125991, -5.000000000000000000 ) ) ;
#4372 = ADVANCED_FACE ( 'NONE', ( #117 ), #56259, .F. ) ;
#4373 = ORIENTED_EDGE ( 'NONE', *, *, #58181, .T. ) ;
#4374 = CARTESIAN_POINT ( 'NONE',  ( 18.77812500061451573, 6.421520780324663323E-16, -5.243569643749999010 ) ) ;
#4375 = CARTESIAN_POINT ( 'NONE',  ( 11.16562500061451679, 3.027376345333613106, -5.243569643749998122 ) ) ;
#4376 = CARTESIAN_POINT ( 'NONE',  ( 22.20937500061451786, -5.492252693125287522, -1.008910452111647106E-15 ) ) ;
#4377 = CARTESIAN_POINT ( 'NONE',  ( 6.984375000614516438, -4.541064518000419881, 2.621784821874995952 ) ) ;
#4378 = CARTESIAN_POINT ( 'NONE',  ( 19.53750000122903430, 6.123233995736764310E-16, -4.999999999999998224 ) ) ;
#4379 = CARTESIAN_POINT ( 'NONE',  ( 0.000000000000000000, 0.000000000000000000, -50.00000000000000000 ) ) ;
#4380 = CARTESIAN_POINT ( 'NONE',  ( 6.046875000614519102, -3.027376345333614438, 5.243569643749998122 ) ) ;
#4381 = CARTESIAN_POINT ( 'NONE',  ( 15.15937500061451715, -4.541064518000417216, -2.621784821875001281 ) ) ;
#4382 = CARTESIAN_POINT ( 'NONE',  ( 23.29687500061451644, -3.027376345333610441, -5.243569643749999898 ) ) ;
#4383 = CARTESIAN_POINT ( 'NONE',  ( 1.999999999999998668, 15.91250000122903430, -33.46410161513775705 ) ) ;
#4384 = ORIENTED_EDGE ( 'NONE', *, *, #50466, .F. ) ;
#4385 = CARTESIAN_POINT ( 'NONE',  ( 13.79999999999999893, 0.000000000000000000, 4.999999999999998224 ) ) ;
#4386 = CARTESIAN_POINT ( 'NONE',  ( 17.78437500061451715, -4.541064518000419881, 2.621784821874995952 ) ) ;
#4387 = CARTESIAN_POINT ( 'NONE',  ( 10.20937500061451786, -4.541064518000417216, -2.621784821875001281 ) ) ;
#4388 = CIRCLE ( 'NONE', #39822, 1.500000000000000444 ) ;
#4389 = CARTESIAN_POINT ( 'NONE',  ( 1.878215178125000495, 14.06562499938548250, 26.74683588394047007 ) ) ;
#4390 = CARTESIAN_POINT ( 'NONE',  ( 20.17499999999999716, -4.330127018922194537, 2.499999999999995559 ) ) ;
#4391 = CARTESIAN_POINT ( 'NONE',  ( -8.484601909799255319E-16, 16.88749999999999929, 34.61880215351700940 ) ) ;
#4392 = CARTESIAN_POINT ( 'NONE',  ( 2.121784821875001281, 10.55937500061451750, -26.32496088578401938 ) ) ;
#4393 = CARTESIAN_POINT ( 'NONE',  ( 21.30937500061451573, 0.000000000000000000, 4.756430356249998326 ) ) ;
#4394 = CARTESIAN_POINT ( 'NONE',  ( 13.64062500061451644, -3.027376345333614438, 5.243569643749998122 ) ) ;
#4395 = CARTESIAN_POINT ( 'NONE',  ( 29.03437500061451715, -4.541064518000419881, 2.621784821874995952 ) ) ;
#4396 = CARTESIAN_POINT ( 'NONE',  ( 22.40625000122903288, 0.000000000000000000, 4.999999999999998224 ) ) ;
#4397 = CARTESIAN_POINT ( 'NONE',  ( 29.55937500061451573, -4.541064518000417216, -2.621784821875001281 ) ) ;
#4398 = CARTESIAN_POINT ( 'NONE',  ( 12.56250000000000178, -5.773502691896255534, -1.060575238724906372E-15 ) ) ;
#4399 = CARTESIAN_POINT ( 'NONE',  ( 4.000000000000000000, 18.05000000122903359, 32.30940107675849049 ) ) ;
#4400 = CARTESIAN_POINT ( 'NONE',  ( 11.51250000122903216, 4.330127018922192761, -2.499999999999997780 ) ) ;
#4401 = CARTESIAN_POINT ( 'NONE',  ( 22.84687500061451715, -3.027376345333610441, -5.243569643749999898 ) ) ;
#4402 = CARTESIAN_POINT ( 'NONE',  ( 17.67187500061451644, 3.027376345333611329, 5.243569643749999010 ) ) ;
#4403 = CARTESIAN_POINT ( 'NONE',  ( 1.626862140677534273E-15, 12.46250000000000213, 34.00000000000000000 ) ) ;
#4404 = ORIENTED_EDGE ( 'NONE', *, *, #51739, .T. ) ;
#4405 = CARTESIAN_POINT ( 'NONE',  ( 16.45312500061451289, -4.541064518000417216, -2.621784821875001281 ) ) ;
#4406 = CARTESIAN_POINT ( 'NONE',  ( 28.95000000122903572, -2.886751345948125991, -5.000000000000000000 ) ) ;
#4407 = CARTESIAN_POINT ( 'NONE',  ( 15.94687500061451502, -3.027376345333614438, 5.243569643749998122 ) ) ;
#4408 = CARTESIAN_POINT ( 'NONE',  ( 5.918267800642006193, 8.060802005575231632, -28.99320351616295355 ) ) ;
#4409 = CARTESIAN_POINT ( 'NONE',  ( 18.70312500061451644, -4.541064518000417216, -2.621784821875001281 ) ) ;
#4410 = LINE ( 'NONE', #50917, #49252 ) ;
#4411 = CARTESIAN_POINT ( 'NONE',  ( 29.07187500061451502, -6.054752690667223547, -1.112240025338166033E-15 ) ) ;
#4412 = CARTESIAN_POINT ( 'NONE',  ( 4.243569643749999898, 11.89062500061451644, 32.45002607614398471 ) ) ;
#4413 = CARTESIAN_POINT ( 'NONE',  ( 18.19687500061451502, -3.027376345333614438, 5.243569643749998122 ) ) ;
#4414 = CARTESIAN_POINT ( 'NONE',  ( 13.72500000122903074, 2.886751345948129099, -4.999999999999998224 ) ) ;
#4415 = CARTESIAN_POINT ( 'NONE',  ( 9.271875000614519635, -5.492252693125287522, -1.008910452111647106E-15 ) ) ;
#4416 = CARTESIAN_POINT ( 'NONE',  ( -4.243569643749999898, 18.95937500061451431, -30.00000000000000000 ) ) ;
#4417 = CARTESIAN_POINT ( 'NONE',  ( 21.64687500061451786, 6.054752690667223547, 3.707466751127219781E-16 ) ) ;
#4418 = CARTESIAN_POINT ( 'NONE',  ( 21.41250000122903074, 4.330127018922192761, -2.499999999999997780 ) ) ;
#4419 = CARTESIAN_POINT ( 'NONE',  ( 17.14687500061451786, 6.054752690667223547, 3.707466751127219781E-16 ) ) ;
#4420 = CARTESIAN_POINT ( 'NONE',  ( 12.89062500061451821, -3.027376345333610441, -5.243569643749999898 ) ) ;
#4421 = CARTESIAN_POINT ( 'NONE',  ( 9.001249775931846008E-16, 15.47187500061451892, 34.90005215228797653 ) ) ;
#4422 = CARTESIAN_POINT ( 'NONE',  ( 16.30312500061451786, 0.000000000000000000, 5.243569643749999010 ) ) ;
#4423 = VERTEX_POINT ( 'NONE', #34068 ) ;
#4424 = VERTEX_POINT ( 'NONE', #56608 ) ;
#4425 = CARTESIAN_POINT ( 'NONE',  ( 21.97500000000000142, -4.330127018922194537, 2.499999999999995559 ) ) ;
#4426 = CARTESIAN_POINT ( 'NONE',  ( 4.243569643749999010, 19.22187500061452070, -32.45002607614398471 ) ) ;
#4427 = CARTESIAN_POINT ( 'NONE',  ( 24.14062500061451289, -3.027376345333610441, -5.243569643749999898 ) ) ;
#4428 = CARTESIAN_POINT ( 'NONE',  ( 5.390625000614518214, 6.054752690667223547, 3.707466751127219781E-16 ) ) ;
#4429 = CARTESIAN_POINT ( 'NONE',  ( 17.62500000122903288, -5.773502691896255534, -1.060575238724906372E-15 ) ) ;
#4430 = EDGE_CURVE ( 'NONE', #50794, #47796, #19291, .T. ) ;
#4431 = CARTESIAN_POINT ( 'NONE',  ( 22.26562500061451644, -6.054752690667223547, -1.112240025338166033E-15 ) ) ;
#4432 = CARTESIAN_POINT ( 'NONE',  ( 23.81250000000000000, -5.773502691896255534, -1.060575238724906372E-15 ) ) ;
#4433 = CARTESIAN_POINT ( 'NONE',  ( 26.12812500061451360, 4.541064518000418104, 2.621784821874999949 ) ) ;
#4434 = CARTESIAN_POINT ( 'NONE',  ( 5.165625000614518569, -6.054752690667223547, -1.112240025338166033E-15 ) ) ;
#4435 = ORIENTED_EDGE ( 'NONE', *, *, #34178, .F. ) ;
#4436 = CARTESIAN_POINT ( 'NONE',  ( 22.22812500061451502, -4.541064518000419881, 2.621784821874995952 ) ) ;
#4437 = CARTESIAN_POINT ( 'NONE',  ( 3.515625000614516882, 3.027376345333613106, -5.243569643749998122 ) ) ;
#4438 = CARTESIAN_POINT ( 'NONE',  ( 11.22187500061451892, 2.746126346562645981, -4.756430356249997438 ) ) ;
#4439 = FACE_OUTER_BOUND ( 'NONE', #49795, .T. ) ;
#4440 = CARTESIAN_POINT ( 'NONE',  ( 1.999999999999998668, 14.11250000122903359, -33.46410161513775705 ) ) ;
#4441 = CARTESIAN_POINT ( 'NONE',  ( -4.243569643749999898, 19.85937500061451644, -30.00000000000000000 ) ) ;
#4442 = CARTESIAN_POINT ( 'NONE',  ( 10.80000000000000071, -4.330127018922190985, -2.500000000000001332 ) ) ;
#4443 =( BOUNDED_CURVE ( )  B_SPLINE_CURVE ( 2, ( #43492, #42757, #43860, #59730, #21306, #37572, #20565, #66385, #15761 ),
 .UNSPECIFIED., .F., .F. ) 
 B_SPLINE_CURVE_WITH_KNOTS ( ( 3, 2, 2, 2, 3 ),
 ( 0.5108695652173913526, 0.5144927536231883591, 0.5217391304347825942, 0.5289855072463768293, 0.5326086956521739468 ),
 .UNSPECIFIED. ) 
 CURVE ( )  GEOMETRIC_REPRESENTATION_ITEM ( )  RATIONAL_B_SPLINE_CURVE ( ( 0.9330127018922192983, 0.9330127018922202975, 1.000000000000000000, 0.8660254037844387076, 1.000000000000000000, 0.8660254037844387076, 1.000000000000000000, 0.9330127018922194093, 0.9330127018922194093 ) ) 
 REPRESENTATION_ITEM ( '' )  );
#4444 = CARTESIAN_POINT ( 'NONE',  ( 12.30937500061451573, 0.000000000000000000, 5.243569643749999010 ) ) ;
#4445 = CARTESIAN_POINT ( 'NONE',  ( 7.162500001229032520, 0.000000000000000000, 4.999999999999998224 ) ) ;
#4446 = CARTESIAN_POINT ( 'NONE',  ( 13.99687500061451928, 6.054752690667223547, 3.707466751127219781E-16 ) ) ;
#4447 = CARTESIAN_POINT ( 'NONE',  ( 6.046875000614519102, -3.027376345333614438, 5.243569643749998122 ) ) ;
#4448 = CARTESIAN_POINT ( 'NONE',  ( 16.72500000000000142, 6.123233995736764310E-16, -4.999999999999998224 ) ) ;
#4449 = CARTESIAN_POINT ( 'NONE',  ( 3.429021053364167404, 3.639313985669003326, 3.429021053364167404 ) ) ;
#4450 = CARTESIAN_POINT ( 'NONE',  ( 11.85937500061451644, 0.000000000000000000, 5.243569643749999010 ) ) ;
#4451 = CARTESIAN_POINT ( 'NONE',  ( 6.112500001229034474, 4.330127018922192761, -2.499999999999997780 ) ) ;
#4452 = CARTESIAN_POINT ( 'NONE',  ( 22.75312500061451360, -4.541064518000417216, -2.621784821875001281 ) ) ;
#4453 = CARTESIAN_POINT ( 'NONE',  ( 16.57499999999999929, -4.330127018922194537, 2.499999999999995559 ) ) ;
#4454 = DIRECTION ( 'NONE',  ( 0.000000000000000000, 0.000000000000000000, 1.000000000000000000 ) ) ;
#4455 = CARTESIAN_POINT ( 'NONE',  ( 24.45937500061451786, 0.000000000000000000, 5.243569643749999010 ) ) ;
#4456 = CARTESIAN_POINT ( 'NONE',  ( 4.027635003466097707, 2.962795348797195416, -4.326299380533228600 ) ) ;
#4457 = CARTESIAN_POINT ( 'NONE',  ( 3.253125000614518036, 0.000000000000000000, 5.243569643749999010 ) ) ;
#4458 = CARTESIAN_POINT ( 'NONE',  ( 19.28437500061451715, 5.492252693125287522, 3.363034840372157021E-16 ) ) ;
#4459 = CARTESIAN_POINT ( 'NONE',  ( 24.74062500061451786, 6.054752690667223547, 3.707466751127219781E-16 ) ) ;
#4460 = CARTESIAN_POINT ( 'NONE',  ( 18.40312500061451573, 4.541064518000418104, -2.621784821874998173 ) ) ;
#4461 = CARTESIAN_POINT ( 'NONE',  ( 13.89375000122903536, -2.886751345948129988, 4.999999999999997335 ) ) ;
#4462 = CARTESIAN_POINT ( 'NONE',  ( 14.18437500061451750, -4.541064518000419881, 2.621784821874995952 ) ) ;
#4463 = FACE_OUTER_BOUND ( 'NONE', #25932, .T. ) ;
#4464 = CARTESIAN_POINT ( 'NONE',  ( 26.88750000122903216, 4.330127018922191873, 2.499999999999999556 ) ) ;
#4465 = CARTESIAN_POINT ( 'NONE',  ( 4.771875000614516971, -6.054752690667223547, -1.112240025338166033E-15 ) ) ;
#4466 = CARTESIAN_POINT ( 'NONE',  ( 15.83437500061451608, 4.541064518000418104, 2.621784821874999949 ) ) ;
#4467 = CARTESIAN_POINT ( 'NONE',  ( 4.838581423605995191, -1.260210223389511386, -5.089881413325959336 ) ) ;
#4468 = CARTESIAN_POINT ( 'NONE',  ( 4.762500001229033941, 4.330127018922192761, -2.499999999999997780 ) ) ;
#4469 = CARTESIAN_POINT ( 'NONE',  ( 23.89687500061451786, 6.054752690667223547, 3.707466751127219781E-16 ) ) ;
#4470 = CARTESIAN_POINT ( 'NONE',  ( 16.39687500061451786, -3.027376345333614438, 5.243569643749998122 ) ) ;
#4471 = CARTESIAN_POINT ( 'NONE',  ( -3.756430356249999214, 16.99062499938548143, 27.83122392262697531 ) ) ;
#4472 = CARTESIAN_POINT ( 'NONE',  ( 29.17500000000000071, -4.330127018922194537, 2.499999999999995559 ) ) ;
#4473 = CARTESIAN_POINT ( 'NONE',  ( 6.375000000000001776, 6.123233995736764310E-16, -4.999999999999998224 ) ) ;
#4474 = CARTESIAN_POINT ( 'NONE',  ( 29.03437500061451715, -4.119189519843968306, 2.378215178124996054 ) ) ;
#4475 = CARTESIAN_POINT ( 'NONE',  ( 19.56562500061451715, -6.054752690667223547, -1.112240025338166033E-15 ) ) ;
#4476 = CARTESIAN_POINT ( 'NONE',  ( 9.862500000000000711, -5.773502691896255534, -1.060575238724906372E-15 ) ) ;
#4477 = EDGE_CURVE ( 'NONE', #68418, #66075, #24840, .T. ) ;
#4478 = CARTESIAN_POINT ( 'NONE',  ( 5.128125000614516260, -4.541064518000419881, 2.621784821874995952 ) ) ;
#4479 = CARTESIAN_POINT ( 'NONE',  ( 20.62499999999999645, -4.330127018922194537, 2.499999999999995559 ) ) ;
#4480 = CARTESIAN_POINT ( 'NONE',  ( 4.000000000000000000, 16.49374999877096570, 30.00000000000000000 ) ) ;
#4481 = CARTESIAN_POINT ( 'NONE',  ( 22.68750000122903288, 6.123233995736764310E-16, -4.999999999999998224 ) ) ;
#4482 = CYLINDRICAL_SURFACE ( 'NONE', #38309, 4.999999999999998224 ) ;
#4483 = CARTESIAN_POINT ( 'NONE',  ( 28.84687500061452070, 6.054752690667223547, 3.707466751127219781E-16 ) ) ;
#4484 = ORIENTED_EDGE ( 'NONE', *, *, #7700, .F. ) ;
#4485 = CARTESIAN_POINT ( 'NONE',  ( 16.30312500061451786, 0.000000000000000000, 5.243569643749999010 ) ) ;
#4486 = CARTESIAN_POINT ( 'NONE',  ( 23.24062500061451786, -3.027376345333610441, -5.243569643749999898 ) ) ;
#4487 = CARTESIAN_POINT ( 'NONE',  ( 24.45937500061451786, 0.000000000000000000, 5.243569643749999010 ) ) ;
#4488 = CARTESIAN_POINT ( 'NONE',  ( 6.299999999999999822, -4.330127018922190985, -2.500000000000001332 ) ) ;
#4489 = CARTESIAN_POINT ( 'NONE',  ( 10.94062500061451537, -3.027376345333614438, 5.243569643749998122 ) ) ;
#4490 = CARTESIAN_POINT ( 'NONE',  ( 25.97812500061451502, 6.421520780324663323E-16, -5.243569643749999010 ) ) ;
#4491 = CARTESIAN_POINT ( 'NONE',  ( 15.42187500061451821, 3.027376345333611329, 5.243569643749999010 ) ) ;
#4492 = CARTESIAN_POINT ( 'NONE',  ( 18.94687500061451502, 6.054752690667223547, 3.707466751127219781E-16 ) ) ;
#4493 = CARTESIAN_POINT ( 'NONE',  ( 3.999999999999998668, 11.82500000122903394, -32.30940107675850470 ) ) ;
#4494 = CARTESIAN_POINT ( 'NONE',  ( -2.121784821874999949, 10.33437500061451786, 26.32496088578401938 ) ) ;
#4495 = AXIS2_PLACEMENT_3D ( 'NONE', #28384, #33555, #6215 ) ;
#4496 = CARTESIAN_POINT ( 'NONE',  ( 22.61250000122903003, -4.330127018922190985, -2.500000000000001332 ) ) ;
#4497 = CARTESIAN_POINT ( 'NONE',  ( 16.88437500061451502, -4.119189519843968306, 2.378215178124996054 ) ) ;
#4498 = CARTESIAN_POINT ( 'NONE',  ( 12.85312500061451502, -4.541064518000417216, -2.621784821875001281 ) ) ;
#4499 = CARTESIAN_POINT ( 'NONE',  ( 6.834375000614518747, 4.541064518000418104, 2.621784821874999949 ) ) ;
#4500 = CARTESIAN_POINT ( 'NONE',  ( 7.021875000614518747, -6.054752690667223547, -1.112240025338166033E-15 ) ) ;
#4501 = ORIENTED_EDGE ( 'NONE', *, *, #23875, .F. ) ;
#4502 = CARTESIAN_POINT ( 'NONE',  ( 27.79687500061451999, -3.027376345333610441, -5.243569643749999898 ) ) ;
#4503 = CARTESIAN_POINT ( 'NONE',  ( 18.74062500061451431, -3.027376345333610441, -5.243569643749999898 ) ) ;
#4504 = CARTESIAN_POINT ( 'NONE',  ( 3.778125000614519280, -4.541064518000419881, 2.621784821874995952 ) ) ;
#4505 = CARTESIAN_POINT ( 'NONE',  ( 3.984375000614517326, 6.421520780324663323E-16, -5.243569643749999010 ) ) ;
#4506 = CARTESIAN_POINT ( 'NONE',  ( 23.74687500061451573, -3.027376345333610441, -5.243569643749999898 ) ) ;
#4507 = CARTESIAN_POINT ( 'NONE',  ( 19.11562500061451431, -6.054752690667223547, -1.112240025338166033E-15 ) ) ;
#4508 = CARTESIAN_POINT ( 'NONE',  ( 2.000000000000001332, 12.05000000000000249, 33.46410161513774995 ) ) ;
#4509 = CARTESIAN_POINT ( 'NONE',  ( 25.52812500061451573, 6.421520780324663323E-16, -5.243569643749999010 ) ) ;
#4510 = CARTESIAN_POINT ( 'NONE',  ( 4.762500001229033941, 4.330127018922192761, -2.499999999999997780 ) ) ;
#4511 = ORIENTED_EDGE ( 'NONE', *, *, #41045, .F. ) ;
#4512 = CARTESIAN_POINT ( 'NONE',  ( 29.47499999999999787, 4.330127018922191873, 2.499999999999999556 ) ) ;
#4513 = CARTESIAN_POINT ( 'NONE',  ( 1.999999999999998668, 16.25000000000000000, -33.46410161513775705 ) ) ;
#4514 = CARTESIAN_POINT ( 'NONE',  ( 1.878215178125000495, 15.97812499938548392, 26.74683588394047007 ) ) ;
#4515 = CARTESIAN_POINT ( 'NONE',  ( 5.446875000614518569, 6.054752690667223547, 3.707466751127219781E-16 ) ) ;
#4516 = DIRECTION ( 'NONE',  ( 0.000000000000000000, 0.000000000000000000, 1.000000000000000000 ) ) ;
#4517 = CARTESIAN_POINT ( 'NONE',  ( 11.42812500061451608, -4.541064518000419881, 2.621784821874995952 ) ) ;
#4518 = CARTESIAN_POINT ( 'NONE',  ( 6.646875000614518747, -3.027376345333610441, -5.243569643749999898 ) ) ;
#4519 = CARTESIAN_POINT ( 'NONE',  ( 24.45000000122903572, -2.886751345948125991, -5.000000000000000000 ) ) ;
#4520 = CARTESIAN_POINT ( 'NONE',  ( 15.79687500061451644, 6.054752690667223547, 3.707466751127219781E-16 ) ) ;
#4521 = CARTESIAN_POINT ( 'NONE',  ( 3.834375000614519635, -4.541064518000419881, 2.621784821874995952 ) ) ;
#4522 = CARTESIAN_POINT ( 'NONE',  ( 9.528763966825557376E-15, 17.41249999999999787, -26.00000000000000000 ) ) ;
#4523 = CARTESIAN_POINT ( 'NONE',  ( -1.999999999999997113, 15.68750000122903465, -26.53589838486224295 ) ) ;
#4524 = CARTESIAN_POINT ( 'NONE',  ( 16.37812500061451715, -4.541064518000419881, 2.621784821874995952 ) ) ;
#4525 = VERTEX_POINT ( 'NONE', #25531 ) ;
#4526 = CARTESIAN_POINT ( 'NONE',  ( 10.52812500061451750, -4.541064518000419881, 2.621784821874995952 ) ) ;
#4527 = CARTESIAN_POINT ( 'NONE',  ( 9.028125000614517504, 4.541064518000418104, 2.621784821874999949 ) ) ;
#4528 = CARTESIAN_POINT ( 'NONE',  ( 18.90937500061451360, 4.119189519843966529, -2.378215178124998275 ) ) ;
#4529 = CARTESIAN_POINT ( 'NONE',  ( 9.337500000000000355, -2.886751345948129988, 4.999999999999997335 ) ) ;
#4530 = EDGE_CURVE ( 'NONE', #59687, #19922, #58042, .T. ) ;
#4531 = CARTESIAN_POINT ( 'NONE',  ( 5.287500001229035185, 4.330127018922191873, 2.499999999999999556 ) ) ;
#4532 = CARTESIAN_POINT ( 'NONE',  ( 18.26249999999999929, 2.886751345948126879, 4.999999999999999112 ) ) ;
#4533 = CARTESIAN_POINT ( 'NONE',  ( 18.64687500061451786, -3.027376345333614438, 5.243569643749998122 ) ) ;
#4534 = CARTESIAN_POINT ( 'NONE',  ( 14.85000000122903252, -2.886751345948129988, 4.999999999999997335 ) ) ;
#4535 = CARTESIAN_POINT ( 'NONE',  ( 20.66250000000000142, -5.773502691896255534, -1.060575238724906372E-15 ) ) ;
#4536 = CARTESIAN_POINT ( 'NONE',  ( 4.243569643749999010, 16.46562500061451573, -32.45002607614398471 ) ) ;
#4537 = CARTESIAN_POINT ( 'NONE',  ( -1.626862140677534273E-15, 20.03749999999999787, 34.00000000000000000 ) ) ;
#4538 = CARTESIAN_POINT ( 'NONE',  ( 17.62500000000000000, 6.123233995736764310E-16, -4.999999999999998224 ) ) ;
#4539 = CARTESIAN_POINT ( 'NONE',  ( 29.42812500061451431, -4.541064518000419881, 2.621784821874995952 ) ) ;
#4540 = CARTESIAN_POINT ( 'NONE',  ( 17.47499999999999787, -4.330127018922194537, 2.499999999999995559 ) ) ;
#4541 = CARTESIAN_POINT ( 'NONE',  ( 13.50937500061451679, 4.541064518000418104, -2.621784821874998173 ) ) ;
#4542 = CARTESIAN_POINT ( 'NONE',  ( 27.03750000000000142, -2.886751345948125991, -5.000000000000000000 ) ) ;
#4543 = CARTESIAN_POINT ( 'NONE',  ( 10.04062500061451502, -3.027376345333614438, 5.243569643749998122 ) ) ;
#4544 = CARTESIAN_POINT ( 'NONE',  ( 27.83437500061451075, 5.492252693125287522, 3.363034840372157021E-16 ) ) ;
#4545 = CARTESIAN_POINT ( 'NONE',  ( 22.54687500061451999, 6.054752690667223547, 3.707466751127219781E-16 ) ) ;
#4546 = CARTESIAN_POINT ( 'NONE',  ( 12.87187500061451750, 5.824947211148865298E-16, -4.756430356249998326 ) ) ;
#4547 = CARTESIAN_POINT ( 'NONE',  ( 7.940625000614518036, -3.027376345333610441, -5.243569643749999898 ) ) ;
#4548 = CARTESIAN_POINT ( 'NONE',  ( 13.20937500061451786, 0.000000000000000000, 5.243569643749999010 ) ) ;
#4549 = ORIENTED_EDGE ( 'NONE', *, *, #793, .F. ) ;
#4550 = CARTESIAN_POINT ( 'NONE',  ( 22.95937500061451431, 4.541064518000418104, -2.621784821874998173 ) ) ;
#4551 = CARTESIAN_POINT ( 'NONE',  ( 1.351293209486986502, 4.820886669536880831, -33.77432306116990901 ) ) ;
#4552 = CYLINDRICAL_SURFACE ( 'NONE', #62031, 9.000000000000000000 ) ;
#4553 = CARTESIAN_POINT ( 'NONE',  ( 6.000000000000001776, 4.330127018922192761, -2.499999999999997780 ) ) ;
#4554 = CARTESIAN_POINT ( 'NONE',  ( 17.51250000122903216, 0.000000000000000000, 4.999999999999998224 ) ) ;
#4555 = CARTESIAN_POINT ( 'NONE',  ( -2.000000000000001776, 19.94374999877096499, 33.46410161513775705 ) ) ;
#4556 = CARTESIAN_POINT ( 'NONE',  ( 17.21249999999999858, 2.886751345948095793, -5.000000000000055067 ) ) ;
#4557 = EDGE_LOOP ( 'NONE', ( #30061, #35969, #11210, #14169 ) ) ;
#4558 = EDGE_CURVE ( 'NONE', #47688, #38854, #26886, .T. ) ;
#4559 = CARTESIAN_POINT ( 'NONE',  ( 12.59999999999999964, -4.330127018922190985, -2.500000000000001332 ) ) ;
#4560 = CARTESIAN_POINT ( 'NONE',  ( 16.38749999999999929, 5.773502691896255534, 3.535250795749688894E-16 ) ) ;
#4561 = CARTESIAN_POINT ( 'NONE',  ( 13.83750000122903323, 4.330127018922191873, 2.499999999999999556 ) ) ;
#4562 = CARTESIAN_POINT ( 'NONE',  ( 10.71562500061451928, 3.027376345333613106, -5.243569643749998122 ) ) ;
#4563 = ORIENTED_EDGE ( 'NONE', *, *, #21957, .F. ) ;
#4564 = CARTESIAN_POINT ( 'NONE',  ( -4.243569643749997233, 13.59687500061451715, -27.54997392385601174 ) ) ;
#4565 = CARTESIAN_POINT ( 'NONE',  ( 4.640625000614518214, -3.027376345333614438, 5.243569643749998122 ) ) ;
#4566 = CARTESIAN_POINT ( 'NONE',  ( -1.878215178124999163, 15.49062499938548321, 26.74683588394047007 ) ) ;
#4567 = CARTESIAN_POINT ( 'NONE',  ( 9.937500000000001776, -2.886751345948125991, -5.000000000000000000 ) ) ;
#4568 = CARTESIAN_POINT ( 'NONE',  ( 3.073301885803186639, 3.943998191421653310, 3.145473502252839726 ) ) ;
#4569 = ORIENTED_EDGE ( 'NONE', *, *, #62104, .T. ) ;
#4570 = CARTESIAN_POINT ( 'NONE',  ( 24.81562500061451715, 3.027376345333611329, 5.243569643749999010 ) ) ;
#4571 = CARTESIAN_POINT ( 'NONE',  ( 29.47499999999999787, 4.330127018922191873, 2.499999999999999556 ) ) ;
#4572 = CARTESIAN_POINT ( 'NONE',  ( 1.878215178124997609, 19.31562499938548427, 33.25316411605952993 ) ) ;
#4573 = CARTESIAN_POINT ( 'NONE',  ( 20.78437500061451715, 4.541064518000418104, 2.621784821874999949 ) ) ;
#4574 = CARTESIAN_POINT ( 'NONE',  ( 18.70312500061451644, -4.541064518000417216, -2.621784821875001281 ) ) ;
#4575 = CARTESIAN_POINT ( 'NONE',  ( 2.121784821874999061, 14.70312500061459282, -33.67503911421598417 ) ) ;
#4576 = CARTESIAN_POINT ( 'NONE',  ( 7.190625000614518036, 6.054752690667223547, 3.707466751127219781E-16 ) ) ;
#4577 = CARTESIAN_POINT ( 'NONE',  ( 4.040625000614517681, 6.054752690667223547, 3.707466751127219781E-16 ) ) ;
#4578 = CARTESIAN_POINT ( 'NONE',  ( 24.87187500061451573, 2.746126346562643317, 4.756430356249998326 ) ) ;
#4579 = CARTESIAN_POINT ( 'NONE',  ( 21.10312500061451502, 4.541064518000418104, -2.621784821874998173 ) ) ;
#4580 = CARTESIAN_POINT ( 'NONE',  ( 8.896875000614517859, -2.746126346562642428, -4.756430356249999214 ) ) ;
#4581 = CARTESIAN_POINT ( 'NONE',  ( -7.967954043666661671E-16, 18.37812499938548427, 34.33755215474603517 ) ) ;
#4582 = CARTESIAN_POINT ( 'NONE',  ( 15.75937500061451857, 4.541064518000418104, -2.621784821874998173 ) ) ;
#4583 = CARTESIAN_POINT ( 'NONE',  ( 15.57187500061451679, -6.054752690667223547, -1.112240025338166033E-15 ) ) ;
#4584 = CARTESIAN_POINT ( 'NONE',  ( 22.09687500061451715, 6.054752690667223547, 3.707466751127219781E-16 ) ) ;
#4585 = ORIENTED_EDGE ( 'NONE', *, *, #28049, .F. ) ;
#4586 = CARTESIAN_POINT ( 'NONE',  ( 9.001249775931846008E-16, 11.87187500061451395, 34.90005215228797653 ) ) ;
#4587 = CARTESIAN_POINT ( 'NONE',  ( 27.18750000000000000, 5.773502691896255534, 3.535250795749688401E-16 ) ) ;
#4588 = CARTESIAN_POINT ( 'NONE',  ( 26.87812500061451360, 6.421520780324663323E-16, -5.243569643749999010 ) ) ;
#4589 = CARTESIAN_POINT ( 'NONE',  ( 26.72812500061451502, -4.541064518000419881, 2.621784821874995952 ) ) ;
#4590 = CARTESIAN_POINT ( 'NONE',  ( 8.325000001229033941, 2.886751345948129099, -4.999999999999997335 ) ) ;
#4591 = CARTESIAN_POINT ( 'NONE',  ( 2.000000000000001332, 18.80000000000000071, 33.46410161513774995 ) ) ;
#4592 = CARTESIAN_POINT ( 'NONE',  ( 4.884375000614518569, 6.421520780324663323E-16, -5.243569643749999010 ) ) ;
#4593 = CARTESIAN_POINT ( 'NONE',  ( 14.02500000122903323, -5.773502691896255534, -1.060575238724906372E-15 ) ) ;
#4594 = CARTESIAN_POINT ( 'NONE',  ( 10.31250000122903288, 0.000000000000000000, 4.999999999999998224 ) ) ;
#4595 = CARTESIAN_POINT ( 'NONE',  ( 3.778125000614519280, -4.541064518000419881, 2.621784821874995952 ) ) ;
#4596 = CARTESIAN_POINT ( 'NONE',  ( 2.000000000000000444, 15.21874999877096535, 26.53589838486224650 ) ) ;
#4597 = CARTESIAN_POINT ( 'NONE',  ( 19.66875000122903216, 2.886751345948126879, 4.999999999999999112 ) ) ;
#4598 = CARTESIAN_POINT ( 'NONE',  ( 12.75937500061451857, 0.000000000000000000, 5.243569643749999010 ) ) ;
#4599 = CARTESIAN_POINT ( 'NONE',  ( 13.63125000122903252, 6.123233995736764310E-16, -4.999999999999998224 ) ) ;
#4600 = ORIENTED_EDGE ( 'NONE', *, *, #24790, .T. ) ;
#4601 = CARTESIAN_POINT ( 'NONE',  ( 19.60312500061451502, -4.541064518000417216, -2.621784821875001281 ) ) ;
#4602 = CARTESIAN_POINT ( 'NONE',  ( 12.49687500061451573, -3.027376345333610441, -5.243569643749999898 ) ) ;
#4603 = CARTESIAN_POINT ( 'NONE',  ( 5.203125000614518214, -4.541064518000417216, -2.621784821875001281 ) ) ;
#4604 = CARTESIAN_POINT ( 'NONE',  ( 22.84687500061451715, -3.027376345333610441, -5.243569643749999898 ) ) ;
#4605 = CARTESIAN_POINT ( 'NONE',  ( 5.015625000614518214, 3.027376345333611329, 5.243569643749999010 ) ) ;
#4606 = CARTESIAN_POINT ( 'NONE',  ( 1.138803498474273873E-14, 16.38124999877096499, 34.00000000000000000 ) ) ;
#4607 =( BOUNDED_CURVE ( )  B_SPLINE_CURVE ( 2, ( #21318, #70838, #32049, #20951, #60107, #43134, #42768, #66029, #4355 ),
 .UNSPECIFIED., .F., .F. ) 
 B_SPLINE_CURVE_WITH_KNOTS ( ( 3, 2, 2, 2, 3 ),
 ( 0.2282608695652174058, 0.2318840579710144956, 0.2391304347826087029, 0.2463768115942029102, 0.2500000000000000000 ),
 .UNSPECIFIED. ) 
 CURVE ( )  GEOMETRIC_REPRESENTATION_ITEM ( )  RATIONAL_B_SPLINE_CURVE ( ( 0.9330127018922194093, 0.9330127018922196314, 1.000000000000000000, 0.8660254037844387076, 1.000000000000000000, 0.8660254037844387076, 1.000000000000000000, 0.9330127018922196314, 0.9330127018922194093 ) ) 
 REPRESENTATION_ITEM ( '' )  );
#4608 = CARTESIAN_POINT ( 'NONE',  ( 9.075000001229033941, -5.773502691896255534, -1.060575238724906372E-15 ) ) ;
#4609 = CARTESIAN_POINT ( 'NONE',  ( 21.77812500061451928, -4.541064518000419881, 2.621784821874995952 ) ) ;
#4610 = CARTESIAN_POINT ( 'NONE',  ( -2.000000000000000000, 19.13750000122903216, -33.46410161513775705 ) ) ;
#4611 = CARTESIAN_POINT ( 'NONE',  ( 8.625000001229034652, -5.773502691896255534, -1.060575238724906372E-15 ) ) ;
#4612 = CARTESIAN_POINT ( 'NONE',  ( 18.02812500061451573, 4.541064518000418104, 2.621784821874999949 ) ) ;
#4613 = CARTESIAN_POINT ( 'NONE',  ( 15.62812500061451537, 6.421520780324663323E-16, -5.243569643749999010 ) ) ;
#4614 = CARTESIAN_POINT ( 'NONE',  ( 25.84687500061451360, -2.746126346562646425, 4.756430356249996549 ) ) ;
#4615 = CARTESIAN_POINT ( 'NONE',  ( 14.96250000000000036, 2.886751345948129099, -4.999999999999998224 ) ) ;
#4616 = CARTESIAN_POINT ( 'NONE',  ( 11.55000000122903181, 5.773502691896255534, 3.535250795749688894E-16 ) ) ;
#4617 = CARTESIAN_POINT ( 'NONE',  ( 8.203125000614518214, 0.000000000000000000, 5.243569643749999010 ) ) ;
#4618 = CARTESIAN_POINT ( 'NONE',  ( 10.67812500061451608, 6.421520780324663323E-16, -5.243569643749999010 ) ) ;
#4619 = EDGE_CURVE ( 'NONE', #2237, #3790, #57073, .T. ) ;
#4620 = CARTESIAN_POINT ( 'NONE',  ( 20.58750000122903145, 4.330127018922191873, 2.499999999999999556 ) ) ;
#4621 = CARTESIAN_POINT ( 'NONE',  ( 2.121784821875001281, 13.25937500061451857, -26.32496088578401938 ) ) ;
#4622 = CARTESIAN_POINT ( 'NONE',  ( 20.03437500061451715, -4.541064518000419881, 2.621784821874995952 ) ) ;
#4623 = CYLINDRICAL_SURFACE ( 'NONE', #61922, 4.999999999999998224 ) ;
#4624 = CARTESIAN_POINT ( 'NONE',  ( 4.875000001229034652, 2.886751345948126879, 4.999999999999999112 ) ) ;
#4625 = CARTESIAN_POINT ( 'NONE',  ( 4.734375000614518214, -4.541064518000419881, 2.621784821874995952 ) ) ;
#4626 = CARTESIAN_POINT ( 'NONE',  ( 20.52187500061451786, -6.054752690667223547, -1.112240025338166033E-15 ) ) ;
#4627 = CARTESIAN_POINT ( 'NONE',  ( 27.75000000000000000, 0.000000000000000000, 4.999999999999998224 ) ) ;
#4628 = CARTESIAN_POINT ( 'NONE',  ( 18.06562500061451715, 3.027376345333611329, 5.243569643749999010 ) ) ;
#4629 = CARTESIAN_POINT ( 'NONE',  ( 11.19375000122903252, -2.886751345948129988, 4.999999999999997335 ) ) ;
#4630 = CARTESIAN_POINT ( 'NONE',  ( 23.17500000000000071, 4.330127018922191873, 2.499999999999999556 ) ) ;
#4631 = CARTESIAN_POINT ( 'NONE',  ( -1.626862140677534273E-15, 14.63749999999999929, 34.00000000000000000 ) ) ;
#4632 = CARTESIAN_POINT ( 'NONE',  ( 27.57187500061451857, 3.027376345333611329, 5.243569643749999010 ) ) ;
#4633 = CARTESIAN_POINT ( 'NONE',  ( 20.29687500061451289, 0.000000000000000000, 4.756430356249998326 ) ) ;
#4634 = CARTESIAN_POINT ( 'NONE',  ( 14.84062500061451750, 6.054752690667223547, 3.707466751127219781E-16 ) ) ;
#4635 = CARTESIAN_POINT ( 'NONE',  ( 12.30937500061451573, 0.000000000000000000, 5.243569643749999010 ) ) ;
#4636 = ORIENTED_EDGE ( 'NONE', *, *, #47275, .F. ) ;
#4637 = CARTESIAN_POINT ( 'NONE',  ( 45.00000000000000000, 0.000000000000000000, 4.999999999999998224 ) ) ;
#4638 = CARTESIAN_POINT ( 'NONE',  ( 23.27812500061451573, 6.421520780324663323E-16, -5.243569643749999010 ) ) ;
#4639 = CYLINDRICAL_SURFACE ( 'NONE', #68731, 4.999999999999998224 ) ;
#4640 = CARTESIAN_POINT ( 'NONE',  ( -1.487416814333745711E-14, 15.72500000122903430, 34.00000000000000000 ) ) ;
#4641 = CARTESIAN_POINT ( 'NONE',  ( 11.77500000000000036, 6.123233995736764310E-16, -4.999999999999998224 ) ) ;
#4642 = CARTESIAN_POINT ( 'NONE',  ( 23.66250000122903430, 4.330127018922192761, -2.499999999999997780 ) ) ;
#4643 = CARTESIAN_POINT ( 'NONE',  ( 19.75312500061451360, 4.541064518000418104, -2.621784821874998173 ) ) ;
#4644 = ORIENTED_EDGE ( 'NONE', *, *, #7878, .F. ) ;
#4645 = CARTESIAN_POINT ( 'NONE',  ( 23.47499999999999787, 6.123233995736764310E-16, -4.999999999999998224 ) ) ;
#4646 =( BOUNDED_CURVE ( )  B_SPLINE_CURVE ( 2, ( #24593, #3172, #69672, #36047, #19038, #70030, #41596, #13500, #52676 ),
 .UNSPECIFIED., .F., .F. ) 
 B_SPLINE_CURVE_WITH_KNOTS ( ( 3, 2, 2, 2, 3 ),
 ( 0.3804347826086956763, 0.3840579710144927383, 0.3913043478260869734, 0.3985507246376811530, 0.4021739130434782705 ),
 .UNSPECIFIED. ) 
 CURVE ( )  GEOMETRIC_REPRESENTATION_ITEM ( )  RATIONAL_B_SPLINE_CURVE ( ( 0.9330127018922194093, 0.9330127018922198534, 1.000000000000000000, 0.8660254037844387076, 1.000000000000000000, 0.8660254037844387076, 1.000000000000000000, 0.9330127018922194093, 0.9330127018922194093 ) ) 
 REPRESENTATION_ITEM ( '' )  );
#4647 = CARTESIAN_POINT ( 'NONE',  ( 21.79687500061451644, -3.027376345333614438, 5.243569643749998122 ) ) ;
#4648 = EDGE_CURVE ( 'NONE', #70526, #25563, #43936, .T. ) ;
#4649 = ORIENTED_EDGE ( 'NONE', *, *, #20885, .F. ) ;
#4650 = CARTESIAN_POINT ( 'NONE',  ( 11.16562500061451679, 3.027376345333613106, -5.243569643749998122 ) ) ;
#4651 = CARTESIAN_POINT ( 'NONE',  ( 3.368666508416885197, 3.694988906523804406, 3.424053828803762745 ) ) ;
#4652 = CARTESIAN_POINT ( 'NONE',  ( 14.22187500061451537, 5.824947211148865298E-16, -4.756430356249998326 ) ) ;
#4653 = CARTESIAN_POINT ( 'NONE',  ( 17.13749999999999929, -2.886751345948125991, -5.000000000000000000 ) ) ;
#4654 = CARTESIAN_POINT ( 'NONE',  ( 25.38749999999999929, 5.773502691896255534, 3.535250795749688894E-16 ) ) ;
#4655 = CARTESIAN_POINT ( 'NONE',  ( -4.243569643749999898, 18.86562500061451431, 27.54997392385601529 ) ) ;
#4656 = CARTESIAN_POINT ( 'NONE',  ( 5.184375000614516615, -4.541064518000419881, 2.621784821874995952 ) ) ;
#4657 = CARTESIAN_POINT ( 'NONE',  ( 28.17187500061451644, -6.054752690667223547, -1.112240025338166033E-15 ) ) ;
#4658 = ORIENTED_EDGE ( 'NONE', *, *, #64328, .T. ) ;
#4659 = CARTESIAN_POINT ( 'NONE',  ( 26.95312500061451644, 4.541064518000418104, -2.621784821874998173 ) ) ;
#4660 = CARTESIAN_POINT ( 'NONE',  ( 27.38437500061451857, 6.421520780324663323E-16, -5.243569643749999010 ) ) ;
#4661 = CARTESIAN_POINT ( 'NONE',  ( 13.53749999999999964, -2.886751345948125991, -5.000000000000000000 ) ) ;
#4662 = CARTESIAN_POINT ( 'NONE',  ( 10.71562500061451928, 3.027376345333613106, -5.243569643749998122 ) ) ;
#4663 = CARTESIAN_POINT ( 'NONE',  ( 13.18125000122903323, 6.123233995736764310E-16, -4.999999999999998224 ) ) ;
#4664 = CARTESIAN_POINT ( 'NONE',  ( 2.411242101361345515E-14, 20.88124999877096499, 34.00000000000000000 ) ) ;
#4665 = CARTESIAN_POINT ( 'NONE',  ( 29.16562500061451502, 3.027376345333612662, -5.243569643749998122 ) ) ;
#4666 = CARTESIAN_POINT ( 'NONE',  ( 15.56250000122903465, 4.330127018922192761, -2.499999999999997780 ) ) ;
#4667 = CARTESIAN_POINT ( 'NONE',  ( 29.22187500061451360, 4.119189519843966529, 2.378215178124999607 ) ) ;
#4668 = CARTESIAN_POINT ( 'NONE',  ( 15.30937500061451750, 4.119189519843966529, -2.378215178124998275 ) ) ;
#4669 = CARTESIAN_POINT ( 'NONE',  ( 5.465625000614517504, 3.027376345333611329, 5.243569643749999010 ) ) ;
#4670 = CARTESIAN_POINT ( 'NONE',  ( 22.43437500061451573, 6.421520780324663323E-16, -5.243569643749999010 ) ) ;
#4671 = CARTESIAN_POINT ( 'NONE',  ( 9.001249775931846008E-16, 15.02187500061451608, 34.90005215228797653 ) ) ;
#4672 = CARTESIAN_POINT ( 'NONE',  ( 21.87187500061451573, -6.054752690667223547, -1.112240025338166033E-15 ) ) ;
#4673 = CARTESIAN_POINT ( 'NONE',  ( 3.787500000000002753, 5.773502691896255534, 3.535250795749688894E-16 ) ) ;
#4674 = CARTESIAN_POINT ( 'NONE',  ( 4.243569643749999898, 19.63437500061451857, 30.00000000000000000 ) ) ;
#4675 = CARTESIAN_POINT ( 'NONE',  ( 8.953125000614518214, 4.541064518000418104, -2.621784821874998173 ) ) ;
#4676 = CARTESIAN_POINT ( 'NONE',  ( 3.075000001229035718, 2.886751345948126879, 4.999999999999999112 ) ) ;
#4677 = CARTESIAN_POINT ( 'NONE',  ( 7.021875000614518747, -6.054752690667223547, -1.112240025338166033E-15 ) ) ;
#4678 = DIRECTION ( 'NONE',  ( 0.000000000000000000, 0.000000000000000000, -1.000000000000000000 ) ) ;
#4679 = CARTESIAN_POINT ( 'NONE',  ( 9.478125000614515017, 4.541064518000418104, 2.621784821874999949 ) ) ;
#4680 = CARTESIAN_POINT ( 'NONE',  ( 15.38437500061451679, 4.541064518000418104, 2.621784821874999949 ) ) ;
#4681 = CARTESIAN_POINT ( 'NONE',  ( -2.000000000000001776, 19.09999999999999787, 33.46410161513775705 ) ) ;
#4682 = CARTESIAN_POINT ( 'NONE',  ( 21.11250000122903359, 0.000000000000000000, 4.999999999999998224 ) ) ;
#4683 = CARTESIAN_POINT ( 'NONE',  ( 6.909375000614518036, 0.000000000000000000, 5.243569643749999010 ) ) ;
#4684 = CARTESIAN_POINT ( 'NONE',  ( 9.740625000614516082, -3.027376345333610441, -5.243569643749999898 ) ) ;
#4685 = CARTESIAN_POINT ( 'NONE',  ( 26.34375000122903288, 5.773502691896255534, 3.535250795749688894E-16 ) ) ;
#4686 = CARTESIAN_POINT ( 'NONE',  ( 18.90937500061451360, 4.541064518000418104, -2.621784821874998173 ) ) ;
#4687 = CYLINDRICAL_SURFACE ( 'NONE', #26646, 5.000000000000000000 ) ;
#4688 = CARTESIAN_POINT ( 'NONE',  ( 0.6840108831340462325, 20.53567971139829496, 33.87926509921195617 ) ) ;
#4689 = CARTESIAN_POINT ( 'NONE',  ( 28.43437500061451573, 4.541064518000418104, 2.621784821874999949 ) ) ;
#4690 = CARTESIAN_POINT ( 'NONE',  ( 9.001249775931846008E-16, 11.42187500061451644, -25.09994784771203058 ) ) ;
#4691 = CARTESIAN_POINT ( 'NONE',  ( 15.00000000122903465, -2.886751345948125991, -5.000000000000000000 ) ) ;
#4692 = CARTESIAN_POINT ( 'NONE',  ( -3.000416591977282496E-16, 15.64062500061451644, -34.90005215228797653 ) ) ;
#4693 = CARTESIAN_POINT ( 'NONE',  ( 15.00000000122903465, -2.886751345948125991, -5.000000000000000000 ) ) ;
#4694 = CARTESIAN_POINT ( 'NONE',  ( 9.740625000614516082, -3.027376345333610441, -5.243569643749999898 ) ) ;
#4695 = ORIENTED_EDGE ( 'NONE', *, *, #29492, .F. ) ;
#4696 = CARTESIAN_POINT ( 'NONE',  ( 14.36249999999999893, -5.773502691896255534, -1.060575238724906372E-15 ) ) ;
#4697 = LINE ( 'NONE', #9864, #23334 ) ;
#4698 = CARTESIAN_POINT ( 'NONE',  ( 21.92812500061451431, 6.421520780324663323E-16, -5.243569643749999010 ) ) ;
#4699 = CARTESIAN_POINT ( 'NONE',  ( 10.58437500061451964, -4.541064518000419881, 2.621784821874995952 ) ) ;
#4700 = CARTESIAN_POINT ( 'NONE',  ( 4.000000000000000000, 16.98124999877096641, 27.69059892324149885 ) ) ;
#4701 = CARTESIAN_POINT ( 'NONE',  ( 9.150000001229033231, -2.886751345948125991, -5.000000000000000000 ) ) ;
#4702 = CARTESIAN_POINT ( 'NONE',  ( 18.07500000122903216, -5.773502691896255534, -1.060575238724906372E-15 ) ) ;
#4703 = CARTESIAN_POINT ( 'NONE',  ( 15.32812500061451644, 4.541064518000418104, 2.621784821874999949 ) ) ;
#4704 = CARTESIAN_POINT ( 'NONE',  ( 19.11562500061451431, -6.054752690667223547, -1.112240025338166033E-15 ) ) ;
#4705 = CARTESIAN_POINT ( 'NONE',  ( 25.08750000122903145, 4.330127018922191873, 2.499999999999999556 ) ) ;
#4706 = CARTESIAN_POINT ( 'NONE',  ( 28.38750000122903216, -4.330127018922194537, 2.499999999999995559 ) ) ;
#4707 = CARTESIAN_POINT ( 'NONE',  ( 23.32499999999999929, -4.330127018922194537, 2.499999999999995559 ) ) ;
#4708 = CARTESIAN_POINT ( 'NONE',  ( -1.878215178124999163, 13.24062499938548321, 26.74683588394047007 ) ) ;
#4709 = CARTESIAN_POINT ( 'NONE',  ( 26.33437500061451431, -4.541064518000419881, 2.621784821874995952 ) ) ;
#4710 = CARTESIAN_POINT ( 'NONE',  ( 18.37500000122903288, 2.886751345948161074, 4.999999999999941380 ) ) ;
#4711 = CARTESIAN_POINT ( 'NONE',  ( 11.55000000122903181, 5.773502691896255534, 3.535250795749688894E-16 ) ) ;
#4712 = CARTESIAN_POINT ( 'NONE',  ( 27.19687500061451857, -3.027376345333614438, 5.243569643749998122 ) ) ;
#4713 = CARTESIAN_POINT ( 'NONE',  ( 12.52500000000000213, -4.330127018922194537, 2.499999999999995559 ) ) ;
#4714 = CARTESIAN_POINT ( 'NONE',  ( 5.409375000614516260, 4.541064518000418104, -2.621784821874998173 ) ) ;
#4715 = CARTESIAN_POINT ( 'NONE',  ( 26.27812500061451573, -4.541064518000419881, 2.621784821874995952 ) ) ;
#4716 = CARTESIAN_POINT ( 'NONE',  ( -3.756430356249999214, 13.84062499938548463, 27.83122392262697176 ) ) ;
#4717 = CARTESIAN_POINT ( 'NONE',  ( 26.00625000122903074, 0.000000000000000000, 4.999999999999998224 ) ) ;
#4718 = CARTESIAN_POINT ( 'NONE',  ( 10.95937500061451964, 0.000000000000000000, 5.243569643749999010 ) ) ;
#4719 = CARTESIAN_POINT ( 'NONE',  ( 22.08750000122903501, -4.330127018922194537, 2.499999999999995559 ) ) ;
#4720 = CARTESIAN_POINT ( 'NONE',  ( 3.571875000614517237, 3.027376345333613106, -5.243569643749998122 ) ) ;
#4721 = CARTESIAN_POINT ( 'NONE',  ( 8.184375000614515727, 4.541064518000418104, 2.621784821874999949 ) ) ;
#4722 = CARTESIAN_POINT ( 'NONE',  ( 29.70937500061451431, 4.541064518000418104, -2.621784821874998173 ) ) ;
#4723 = CARTESIAN_POINT ( 'NONE',  ( 2.121784821875001281, 12.30312500061459424, 33.67503911421598417 ) ) ;
#4724 = CARTESIAN_POINT ( 'NONE',  ( 19.83750000000000213, -2.886751345948125991, -5.000000000000000000 ) ) ;
#4725 = ORIENTED_EDGE ( 'NONE', *, *, #34392, .F. ) ;
#4726 = CARTESIAN_POINT ( 'NONE',  ( 20.88750000122903572, 6.123233995736764310E-16, -4.999999999999998224 ) ) ;
#4727 = CARTESIAN_POINT ( 'NONE',  ( 4.312500000000000000, 2.886751345948126879, 4.999999999999999112 ) ) ;
#4728 = EDGE_CURVE ( 'NONE', #16013, #64135, #51484, .T. ) ;
#4729 = EDGE_LOOP ( 'NONE', ( #3827, #37731, #11039, #19045 ) ) ;
#4730 = CARTESIAN_POINT ( 'NONE',  ( 17.61562500061451786, 3.027376345333611329, 5.243569643749999010 ) ) ;
#4731 = CARTESIAN_POINT ( 'NONE',  ( 8.503125000614515372, 4.541064518000418104, -2.621784821874998173 ) ) ;
#4732 = CARTESIAN_POINT ( 'NONE',  ( 21.38437500061451502, -2.746126346562642428, -4.756430356249999214 ) ) ;
#4733 = CARTESIAN_POINT ( 'NONE',  ( 7.096875000614517148, -3.027376345333610441, -5.243569643749999898 ) ) ;
#4734 = CARTESIAN_POINT ( 'NONE',  ( 16.68750000122903288, -4.330127018922194537, 2.499999999999995559 ) ) ;
#4735 = CARTESIAN_POINT ( 'NONE',  ( 3.160880256176461511, -3.874123901750303300, -3.160880256176591185 ) ) ;
#4736 = CARTESIAN_POINT ( 'NONE',  ( 7.246875000614518392, 6.054752690667223547, 3.707466751127219781E-16 ) ) ;
#4737 = CARTESIAN_POINT ( 'NONE',  ( 12.83437500061451786, -4.541064518000419881, 2.621784821874995952 ) ) ;
#4738 = CARTESIAN_POINT ( 'NONE',  ( 25.35937500061451644, 0.000000000000000000, 5.243569643749999010 ) ) ;
#4739 = CARTESIAN_POINT ( 'NONE',  ( 26.66250000000000142, 2.886751345948129099, -4.999999999999997335 ) ) ;
#4740 = ORIENTED_EDGE ( 'NONE', *, *, #71606, .T. ) ;
#4741 = CARTESIAN_POINT ( 'NONE',  ( 11.10000000000000142, 0.000000000000000000, 4.999999999999998224 ) ) ;
#4742 = CARTESIAN_POINT ( 'NONE',  ( 18.19687500061451502, -3.027376345333614438, 5.243569643749998122 ) ) ;
#4743 = CARTESIAN_POINT ( 'NONE',  ( 10.50937500061451679, 0.000000000000000000, 5.243569643749999010 ) ) ;
#4744 = CARTESIAN_POINT ( 'NONE',  ( -3.756430356250001434, 16.05312499938548143, 32.16877607737301048 ) ) ;
#4745 = CARTESIAN_POINT ( 'NONE',  ( 19.83750000000000213, -2.886751345948125991, -5.000000000000000000 ) ) ;
#4746 = CARTESIAN_POINT ( 'NONE',  ( 2.828200636599751609E-16, 18.01249999999999929, 25.38119784648299415 ) ) ;
#4747 = CARTESIAN_POINT ( 'NONE',  ( -1.626862140677534273E-15, 17.33749999999999858, 34.00000000000000000 ) ) ;
#4748 = CARTESIAN_POINT ( 'NONE',  ( 21.34687500061451715, -2.746126346562646425, 4.756430356249996549 ) ) ;
#4749 = CARTESIAN_POINT ( 'NONE',  ( 13.49062500061451608, 6.054752690667223547, 3.707466751127219781E-16 ) ) ;
#4750 = CARTESIAN_POINT ( 'NONE',  ( 3.300000000000000711, 4.330127018922192761, -2.499999999999997780 ) ) ;
#4751 = CARTESIAN_POINT ( 'NONE',  ( 0.000000000000000000, 20.00000000000000000, 30.00000000000000000 ) ) ;
#4752 = CARTESIAN_POINT ( 'NONE',  ( 29.10937500061451644, -4.541064518000417216, -2.621784821875001281 ) ) ;
#4753 = CARTESIAN_POINT ( 'NONE',  ( 10.27499999999999858, -4.330127018922194537, 2.499999999999995559 ) ) ;
#4754 = CARTESIAN_POINT ( 'NONE',  ( 3.999999999999999112, 15.38750000122903394, 30.00000000000000000 ) ) ;
#4755 = CARTESIAN_POINT ( 'NONE',  ( 8.025000001229035007, 2.886751345948126879, 4.999999999999999112 ) ) ;
#4756 = CARTESIAN_POINT ( 'NONE',  ( 19.77187500061451786, 3.027376345333613106, -5.243569643749998122 ) ) ;
#4757 = CARTESIAN_POINT ( 'NONE',  ( 14.10937500061451644, 0.000000000000000000, 5.243569643749999010 ) ) ;
#4758 = CARTESIAN_POINT ( 'NONE',  ( 1.999999999999998668, 16.81250000122903643, 26.53589838486224650 ) ) ;
#4759 = ORIENTED_EDGE ( 'NONE', *, *, #12791, .T. ) ;
#4760 = CARTESIAN_POINT ( 'NONE',  ( 16.22812500061451857, 4.541064518000418104, 2.621784821874999949 ) ) ;
#4761 = CARTESIAN_POINT ( 'NONE',  ( 29.28750000122903074, -4.330127018922194537, 2.499999999999995559 ) ) ;
#4762 = CARTESIAN_POINT ( 'NONE',  ( 15.04687500061451644, -3.027376345333614438, 5.243569643749998122 ) ) ;
#4763 = CARTESIAN_POINT ( 'NONE',  ( 6.000084452983059258, 7.999936660264888921, -30.40169366477969604 ) ) ;
#4764 = CARTESIAN_POINT ( 'NONE',  ( 17.84062500061451573, -3.027376345333610441, -5.243569643749999898 ) ) ;
#4765 = CARTESIAN_POINT ( 'NONE',  ( 3.999999999999999112, 16.62500000000000000, -30.00000000000000000 ) ) ;
#4766 = CARTESIAN_POINT ( 'NONE',  ( 29.18437500061451573, 6.421520780324663323E-16, -5.243569643749999010 ) ) ;
#4767 = CARTESIAN_POINT ( 'NONE',  ( -4.243569643749997233, 11.74062500061451786, 32.45002607614398471 ) ) ;
#4768 = CARTESIAN_POINT ( 'NONE',  ( 14.40937500061451715, 4.541064518000418104, -2.621784821874998173 ) ) ;
#4769 = CARTESIAN_POINT ( 'NONE',  ( 13.38750000122903394, 4.330127018922191873, 2.499999999999999556 ) ) ;
#4770 = CARTESIAN_POINT ( 'NONE',  ( 11.07187500061451679, -5.492252693125287522, -1.008910452111647106E-15 ) ) ;
#4771 = CARTESIAN_POINT ( 'NONE',  ( -4.243569643749999898, 18.92187500061451644, -32.45002607614398471 ) ) ;
#4772 = CARTESIAN_POINT ( 'NONE',  ( 20.59687500061451360, -3.027376345333610441, -5.243569643749999898 ) ) ;
#4773 = CARTESIAN_POINT ( 'NONE',  ( 22.46250000122903501, 0.000000000000000000, 4.999999999999998224 ) ) ;
#4774 = CARTESIAN_POINT ( 'NONE',  ( 17.85937500061451999, -4.541064518000417216, -2.621784821875001281 ) ) ;
#4775 = CARTESIAN_POINT ( 'NONE',  ( 13.22812500061451502, -4.541064518000419881, 2.621784821874995952 ) ) ;
#4776 = CARTESIAN_POINT ( 'NONE',  ( -2.121784821874999949, 12.58437500061451786, 26.32496088578401938 ) ) ;
#4777 = CARTESIAN_POINT ( 'NONE',  ( 18.14062500061451644, -3.027376345333614438, 5.243569643749998122 ) ) ;
#4778 = VERTEX_POINT ( 'NONE', #31071 ) ;
#4779 = ORIENTED_EDGE ( 'NONE', *, *, #48851, .F. ) ;
#4780 = CARTESIAN_POINT ( 'NONE',  ( 19.65000000000000213, 0.000000000000000000, 4.999999999999998224 ) ) ;
#4781 = CARTESIAN_POINT ( 'NONE',  ( 17.58749999999999858, -2.886751345948092684, -5.000000000000057732 ) ) ;
#4782 = CARTESIAN_POINT ( 'NONE',  ( 24.17812500061451786, 6.421520780324663323E-16, -5.243569643749999010 ) ) ;
#4783 = CARTESIAN_POINT ( 'NONE',  ( 5.465625000614517504, 3.027376345333611329, 5.243569643749999010 ) ) ;
#4784 = CARTESIAN_POINT ( 'NONE',  ( 17.13750000122903216, -4.330127018922194537, 2.499999999999995559 ) ) ;
#4785 = CARTESIAN_POINT ( 'NONE',  ( 22.86562500061451431, 3.027376345333613106, -5.243569643749998122 ) ) ;
#4786 = CARTESIAN_POINT ( 'NONE',  ( 22.34999999999999787, 0.000000000000000000, 4.999999999999998224 ) ) ;
#4787 = CARTESIAN_POINT ( 'NONE',  ( 26.42812500061451431, 6.421520780324663323E-16, -5.243569643749999010 ) ) ;
#4788 = CARTESIAN_POINT ( 'NONE',  ( 6.403125000614517504, 0.000000000000000000, 5.243569643749999010 ) ) ;
#4789 = ORIENTED_EDGE ( 'NONE', *, *, #35474, .T. ) ;
#4790 = EDGE_CURVE ( 'NONE', #37881, #49981, #59003, .T. ) ;
#4791 = CARTESIAN_POINT ( 'NONE',  ( 29.77499999999999858, 6.123233995736764310E-16, -4.999999999999998224 ) ) ;
#4792 = CARTESIAN_POINT ( 'NONE',  ( 2.990625000614519191, -3.027376345333610441, -5.243569643749999898 ) ) ;
#4793 = EDGE_CURVE ( 'NONE', #60642, #33795, #3002, .T. ) ;
#4794 = CARTESIAN_POINT ( 'NONE',  ( 10.58437500061451964, -4.119189519843968306, 2.378215178124996054 ) ) ;
#4795 = CARTESIAN_POINT ( 'NONE',  ( 3.242103837493086330E-14, 11.00000000122903288, 26.00000000000000711 ) ) ;
#4796 = CARTESIAN_POINT ( 'NONE',  ( 3.999999999999998668, 14.07500000122903572, -32.30940107675850470 ) ) ;
#4797 = CARTESIAN_POINT ( 'NONE',  ( -3.000416591977282496E-16, 19.29687500061451644, -34.90005215228797653 ) ) ;
#4798 = CARTESIAN_POINT ( 'NONE',  ( 9.562500000000001776, 2.886751345948129099, -4.999999999999998224 ) ) ;
#4799 = ADVANCED_FACE ( 'NONE', ( #69871 ), #65053, .F. ) ;
#4800 = CARTESIAN_POINT ( 'NONE',  ( 11.93437500061451573, -4.541064518000419881, 2.621784821874995952 ) ) ;
#4801 = CARTESIAN_POINT ( 'NONE',  ( 6.487500001229034474, 6.123233995736764310E-16, -4.999999999999998224 ) ) ;
#4802 = CARTESIAN_POINT ( 'NONE',  ( 12.72187500061451537, 3.027376345333611329, 5.243569643749999010 ) ) ;
#4803 = CARTESIAN_POINT ( 'NONE',  ( 4.921875000614518214, 3.027376345333613106, -5.243569643749998122 ) ) ;
#4804 = CARTESIAN_POINT ( 'NONE',  ( -4.243569643749999898, 10.31562500061451715, -32.45002607614398471 ) ) ;
#4805 = CARTESIAN_POINT ( 'NONE',  ( -2.556497649636125342E-15, 19.21250000000000213, 34.00000000000000000 ) ) ;
#4806 = EDGE_CURVE ( 'NONE', #28753, #71866, #32053, .T. ) ;
#4807 = CARTESIAN_POINT ( 'NONE',  ( 11.25937500061451679, 4.541064518000418104, -2.621784821874998173 ) ) ;
#4808 = CARTESIAN_POINT ( 'NONE',  ( 4.276577733362700862, 2.590537181842085257, -4.276577733362700862 ) ) ;
#4809 = CARTESIAN_POINT ( 'NONE',  ( 19.49062500061451431, -3.027376345333614438, 5.243569643749998122 ) ) ;
#4810 = CARTESIAN_POINT ( 'NONE',  ( -2.000000000000000000, 12.38750000122903394, -33.46410161513775705 ) ) ;
#4811 = CARTESIAN_POINT ( 'NONE',  ( 4.243569643749999898, 19.12812500061459531, 30.00000000000000000 ) ) ;
#4812 = CARTESIAN_POINT ( 'NONE',  ( 23.63437500061451502, -4.541064518000419881, 2.621784821874995952 ) ) ;
#4813 = CARTESIAN_POINT ( 'NONE',  ( 28.31250000122903288, 0.000000000000000000, 4.999999999999998224 ) ) ;
#4814 = CARTESIAN_POINT ( 'NONE',  ( 19.09687500061451360, -4.119189519843965641, -2.378215178125001383 ) ) ;
#4815 = CARTESIAN_POINT ( 'NONE',  ( 24.85312500061451502, 0.000000000000000000, 5.243569643749999010 ) ) ;
#4816 = CARTESIAN_POINT ( 'NONE',  ( 16.86562500061451786, -6.054752690667223547, -1.112240025338166033E-15 ) ) ;
#4817 = CARTESIAN_POINT ( 'NONE',  ( 13.48125000122903394, -4.330127018922194537, 2.499999999999995559 ) ) ;
#4818 = CARTESIAN_POINT ( 'NONE',  ( 15.38437500061451679, 4.541064518000418104, 2.621784821874999949 ) ) ;
#4819 = CARTESIAN_POINT ( 'NONE',  ( 27.11250000122903359, -4.330127018922190985, -2.500000000000001332 ) ) ;
#4820 = CARTESIAN_POINT ( 'NONE',  ( 3.609375000614516882, 4.541064518000418104, -2.621784821874998173 ) ) ;
#4821 = CARTESIAN_POINT ( 'NONE',  ( 15.38437500061451679, 4.541064518000418104, 2.621784821874999949 ) ) ;
#4822 = CARTESIAN_POINT ( 'NONE',  ( 3.999999999999998668, 17.80624999877096570, 32.30940107675850470 ) ) ;
#4823 = CARTESIAN_POINT ( 'NONE',  ( 14.81250000122903288, 0.000000000000000000, 4.999999999999998224 ) ) ;
#4824 = CARTESIAN_POINT ( 'NONE',  ( 3.000000001229032875, 5.773502691896255534, 3.535250795749688894E-16 ) ) ;
#4825 = CARTESIAN_POINT ( 'NONE',  ( 23.67187500061451999, -6.054752690667223547, -1.112240025338166033E-15 ) ) ;
#4826 = CARTESIAN_POINT ( 'NONE',  ( 16.84687500061451715, -3.027376345333614438, 5.243569643749998122 ) ) ;
#4827 = CARTESIAN_POINT ( 'NONE',  ( 1.878215178124997609, 15.37812499938548427, 33.25316411605952993 ) ) ;
#4828 = CARTESIAN_POINT ( 'NONE',  ( 27.63749999999999929, 5.773502691896255534, 3.535250795749688894E-16 ) ) ;
#4829 = CARTESIAN_POINT ( 'NONE',  ( -5.810221930991193690E-16, 10.43750000000000000, 26.00000000000000355 ) ) ;
#4830 = CARTESIAN_POINT ( 'NONE',  ( 5.549999999999998934, 4.330127018922192761, -2.499999999999997780 ) ) ;
#4831 = CARTESIAN_POINT ( 'NONE',  ( 29.40937500061451715, 0.000000000000000000, 4.756430356249998326 ) ) ;
#4832 = CARTESIAN_POINT ( 'NONE',  ( 20.05312500061451431, -4.541064518000417216, -2.621784821875001281 ) ) ;
#4833 = CARTESIAN_POINT ( 'NONE',  ( 9.225000000000001421, 4.330127018922191873, 2.499999999999999556 ) ) ;
#4834 = CARTESIAN_POINT ( 'NONE',  ( 3.778125000614519280, -4.541064518000419881, 2.621784821874995952 ) ) ;
#4835 = CARTESIAN_POINT ( 'NONE',  ( 18.18750000000000000, 5.773502691896255534, 3.535250795749688894E-16 ) ) ;
#4836 = CARTESIAN_POINT ( 'NONE',  ( 15.48750000122903359, 6.123233995736764310E-16, -4.999999999999998224 ) ) ;
#4837 = CARTESIAN_POINT ( 'NONE',  ( 21.03750000122903074, 4.330127018922191873, 2.499999999999999556 ) ) ;
#4838 = CARTESIAN_POINT ( 'NONE',  ( 5.918267800642001752, 8.060802005575231632, 31.00679648383703935 ) ) ;
#4839 = CARTESIAN_POINT ( 'NONE',  ( 3.262500000000001510, 2.886751345948129099, -4.999999999999998224 ) ) ;
#4840 = ORIENTED_EDGE ( 'NONE', *, *, #1055, .F. ) ;
#4841 = CARTESIAN_POINT ( 'NONE',  ( 18.14062500061451644, -3.027376345333614438, 5.243569643749998122 ) ) ;
#4842 = CARTESIAN_POINT ( 'NONE',  ( 24.89062500061451644, -3.027376345333614438, 5.243569643749998122 ) ) ;
#4843 = CARTESIAN_POINT ( 'NONE',  ( 23.03437500061451715, 4.541064518000418104, 2.621784821874999949 ) ) ;
#4844 = CARTESIAN_POINT ( 'NONE',  ( 6.262500000000000178, -5.773502691896255534, -1.060575238724906372E-15 ) ) ;
#4845 = CARTESIAN_POINT ( 'NONE',  ( 8.465625000614515727, 3.027376345333613106, -5.243569643749998122 ) ) ;
#4846 = CARTESIAN_POINT ( 'NONE',  ( 27.40312500061451573, 4.541064518000418104, -2.621784821874998173 ) ) ;
#4847 = CARTESIAN_POINT ( 'NONE',  ( 15.38437500061451679, 4.541064518000418104, 2.621784821874999949 ) ) ;
#4848 = CARTESIAN_POINT ( 'NONE',  ( 20.25937500061451857, 4.541064518000418104, -2.621784821874998173 ) ) ;
#4849 = CYLINDRICAL_SURFACE ( 'NONE', #17960, 4.999999999999998224 ) ;
#4850 = CARTESIAN_POINT ( 'NONE',  ( 9.001249775931846008E-16, 10.52187500061451964, 34.90005215228797653 ) ) ;
#4851 = CARTESIAN_POINT ( 'NONE',  ( 20.92500000122903714, 2.886751345948129099, -4.999999999999998224 ) ) ;
#4852 = CARTESIAN_POINT ( 'NONE',  ( 17.85937500061451999, -4.119189519843965641, -2.378215178125001383 ) ) ;
#4853 = CARTESIAN_POINT ( 'NONE',  ( 12.06562500061451537, 3.027376345333612662, -5.243569643749998122 ) ) ;
#4854 = CARTESIAN_POINT ( 'NONE',  ( 8.334375000614516082, -4.541064518000419881, 2.621784821874995952 ) ) ;
#4855 = CARTESIAN_POINT ( 'NONE',  ( 8.109375000614518214, 4.541064518000418104, -2.621784821874998173 ) ) ;
#4856 = ORIENTED_EDGE ( 'NONE', *, *, #35798, .T. ) ;
#4857 = CARTESIAN_POINT ( 'NONE',  ( 27.75937500061451502, -4.541064518000417216, -2.621784821875001281 ) ) ;
#4858 = CARTESIAN_POINT ( 'NONE',  ( 19.26562500061451644, 3.027376345333613106, -5.243569643749998122 ) ) ;
#4859 = CARTESIAN_POINT ( 'NONE',  ( 28.50000000122903288, -2.886751345948125991, -5.000000000000000000 ) ) ;
#4860 = CARTESIAN_POINT ( 'NONE',  ( 4.396875000614516971, -3.027376345333610441, -5.243569643749999898 ) ) ;
#4861 = CARTESIAN_POINT ( 'NONE',  ( 25.35937500061451644, 0.000000000000000000, 5.243569643749999010 ) ) ;
#4862 = CARTESIAN_POINT ( 'NONE',  ( 19.79062500061451502, 6.054752690667223547, 3.707466751127219781E-16 ) ) ;
#4863 = CARTESIAN_POINT ( 'NONE',  ( 3.999999999999998668, 10.36250000000000071, 27.69059892324149175 ) ) ;
#4864 = CARTESIAN_POINT ( 'NONE',  ( 23.42812500061451786, 4.541064518000418104, 2.621784821874999949 ) ) ;
#4865 = CARTESIAN_POINT ( 'NONE',  ( 4.125000001229034652, -5.773502691896255534, -1.060575238724906372E-15 ) ) ;
#4866 = ORIENTED_EDGE ( 'NONE', *, *, #14038, .F. ) ;
#4867 = CARTESIAN_POINT ( 'NONE',  ( 26.69999999999999929, 4.330127018922192761, -2.499999999999997780 ) ) ;
#4868 = CARTESIAN_POINT ( 'NONE',  ( 3.999999999999999112, 15.72500000000000320, -30.00000000000000000 ) ) ;
#4869 = CARTESIAN_POINT ( 'NONE',  ( -3.756430356250001434, 17.96562499938548285, 32.16877607737301048 ) ) ;
#4870 = CARTESIAN_POINT ( 'NONE',  ( 4.846875000614519813, -3.027376345333610441, -5.243569643749999898 ) ) ;
#4871 = CARTESIAN_POINT ( 'NONE',  ( 12.96562500061451750, 3.027376345333613106, -5.243569643749998122 ) ) ;
#4872 = CARTESIAN_POINT ( 'NONE',  ( 6.421875000614519102, 3.027376345333611329, 5.243569643749999010 ) ) ;
#4873 = CARTESIAN_POINT ( 'NONE',  ( 25.80000000122903714, -2.886751345948125991, -5.000000000000000000 ) ) ;
#4874 = CARTESIAN_POINT ( 'NONE',  ( 16.02187500061451786, -6.054752690667223547, -1.112240025338166033E-15 ) ) ;
#4875 = CARTESIAN_POINT ( 'NONE',  ( 3.121875000614518836, 3.027376345333613106, -5.243569643749998122 ) ) ;
#4876 = CARTESIAN_POINT ( 'NONE',  ( 29.06250000000000000, 2.886751345948126879, 4.999999999999999112 ) ) ;
#4877 = CARTESIAN_POINT ( 'NONE',  ( 25.58437500061451431, 6.421520780324663323E-16, -5.243569643749999010 ) ) ;
#4878 = CARTESIAN_POINT ( 'NONE',  ( 3.778125000614519280, -4.541064518000419881, 2.621784821874995952 ) ) ;
#4879 = CARTESIAN_POINT ( 'NONE',  ( 12.51562500061451821, 3.027376345333613106, -5.243569643749998122 ) ) ;
#4880 =( BOUNDED_CURVE ( )  B_SPLINE_CURVE ( 2, ( #21372, #43926, #66452, #15829, #4765, #57890, #29829, #1406, #7299 ),
 .UNSPECIFIED., .F., .F. ) 
 B_SPLINE_CURVE_WITH_KNOTS ( ( 3, 2, 2, 2, 3 ),
 ( 0.3152173913043478382, 0.3188405797101449002, 0.3260869565217391353, 0.3333333333333333148, 0.3369565217391304324 ),
 .UNSPECIFIED. ) 
 CURVE ( )  GEOMETRIC_REPRESENTATION_ITEM ( )  RATIONAL_B_SPLINE_CURVE ( ( 0.9330127018922194093, 0.9330127018922198534, 1.000000000000000000, 0.8660254037844387076, 1.000000000000000000, 0.8660254037844387076, 1.000000000000000000, 0.9330127018922194093, 0.9330127018922194093 ) ) 
 REPRESENTATION_ITEM ( '' )  );
#4881 = ORIENTED_EDGE ( 'NONE', *, *, #35090, .T. ) ;
#4882 = CARTESIAN_POINT ( 'NONE',  ( 10.26562500061451644, 3.027376345333613106, -5.243569643749998122 ) ) ;
#4883 = CARTESIAN_POINT ( 'NONE',  ( 9.253125000614517148, -4.541064518000417216, -2.621784821875001281 ) ) ;
#4884 = CARTESIAN_POINT ( 'NONE',  ( 19.54687500061451644, -2.746126346562646425, 4.756430356249996549 ) ) ;
#4885 = CARTESIAN_POINT ( 'NONE',  ( 8.212500000000000355, 2.886751345948129099, -4.999999999999998224 ) ) ;
#4886 = CARTESIAN_POINT ( 'NONE',  ( 13.98750000122903359, -4.330127018922194537, 2.499999999999995559 ) ) ;
#4887 = CARTESIAN_POINT ( 'NONE',  ( 17.10000000000000142, -4.330127018922190985, -2.500000000000001332 ) ) ;
#4888 = EDGE_CURVE ( 'NONE', #59956, #7528, #23624, .T. ) ;
#4889 = CARTESIAN_POINT ( 'NONE',  ( 19.62187500061451573, -6.054752690667223547, -1.112240025338166033E-15 ) ) ;
#4890 = CARTESIAN_POINT ( 'NONE',  ( 13.05000000122903536, -2.886751345948129988, 4.999999999999997335 ) ) ;
#4891 = CARTESIAN_POINT ( 'NONE',  ( 20.69999999999999929, -4.330127018922190985, -2.500000000000001332 ) ) ;
#4892 = CARTESIAN_POINT ( 'NONE',  ( 2.121784821875001281, 15.90312500061451573, -26.32496088578401938 ) ) ;
#4893 = CARTESIAN_POINT ( 'NONE',  ( -3.486133158594716510E-16, 12.61250000000000426, 26.00000000000000355 ) ) ;
#4894 = CARTESIAN_POINT ( 'NONE',  ( 26.67187500061451289, -4.119189519843968306, 2.378215178124996054 ) ) ;
#4895 = CARTESIAN_POINT ( 'NONE',  ( 24.16875000122903216, 2.886751345948112668, 5.000000000000023981 ) ) ;
#4896 = CARTESIAN_POINT ( 'NONE',  ( 26.01562500061451289, 3.027376345333613106, -5.243569643749998122 ) ) ;
#4897 = CARTESIAN_POINT ( 'NONE',  ( 28.42499999999999716, 6.123233995736764310E-16, -4.999999999999998224 ) ) ;
#4898 = CARTESIAN_POINT ( 'NONE',  ( 24.18750000000000355, -2.886751345948102898, 5.000000000000044409 ) ) ;
#4899 = CARTESIAN_POINT ( 'NONE',  ( 12.94687500061451857, -3.027376345333610441, -5.243569643749999898 ) ) ;
#4900 = CARTESIAN_POINT ( 'NONE',  ( 25.83749999999999858, 5.773502691896255534, 3.535250795749688894E-16 ) ) ;
#4901 = CARTESIAN_POINT ( 'NONE',  ( 9.215625000614515727, -6.054752690667223547, -1.112240025338166033E-15 ) ) ;
#4902 = CARTESIAN_POINT ( 'NONE',  ( 28.20937500061451075, 2.746126346562645981, -4.756430356249997438 ) ) ;
#4903 = CARTESIAN_POINT ( 'NONE',  ( 22.09687500061451715, 6.054752690667223547, 3.707466751127219781E-16 ) ) ;
#4904 = CARTESIAN_POINT ( 'NONE',  ( 14.55937500061451573, -5.492252693125287522, -1.008910452111647106E-15 ) ) ;
#4905 = CARTESIAN_POINT ( 'NONE',  ( 7.040625000614517681, -3.027376345333610441, -5.243569643749999898 ) ) ;
#4906 = CARTESIAN_POINT ( 'NONE',  ( 10.84687500061451892, 6.054752690667223547, 3.707466751127219781E-16 ) ) ;
#4907 = VERTEX_POINT ( 'NONE', #27009 ) ;
#4908 = CARTESIAN_POINT ( 'NONE',  ( 22.50937500061451857, 4.541064518000418104, -2.621784821874998173 ) ) ;
#4909 = CARTESIAN_POINT ( 'NONE',  ( 0.6891293861215588290, 4.954145703890282526, -26.05743059574101395 ) ) ;
#4910 = CARTESIAN_POINT ( 'NONE',  ( 45.00000000000000000, 0.000000000000000000, 0.000000000000000000 ) ) ;
#4912 = EDGE_CURVE ( 'NONE', #71132, #41920, #9412, .T. ) ;
#4911 = CARTESIAN_POINT ( 'NONE',  ( 4.237500000000001599, 5.773502691896255534, 3.535250795749688894E-16 ) ) ;
#4913 = CARTESIAN_POINT ( 'NONE',  ( 15.07500000122903394, 2.886751345948129099, -4.999999999999998224 ) ) ;
#4914 = DIRECTION ( 'NONE',  ( 0.000000000000000000, 0.000000000000000000, 1.000000000000000000 ) ) ;
#4915 = FACE_BOUND ( 'NONE', #44003, .T. ) ;
#4916 = VERTEX_POINT ( 'NONE', #43999 ) ;
#4917 = CARTESIAN_POINT ( 'NONE',  ( 11.81250000000000000, 2.886751345948129099, -4.999999999999998224 ) ) ;
#4918 = CARTESIAN_POINT ( 'NONE',  ( 15.52500000000000036, 4.330127018922191873, 2.499999999999999556 ) ) ;
#4919 = CARTESIAN_POINT ( 'NONE',  ( 12.45000000122903394, 5.773502691896255534, 3.535250795749688894E-16 ) ) ;
#4920 = CARTESIAN_POINT ( 'NONE',  ( 12.40312500061451573, -4.541064518000417216, -2.621784821875001281 ) ) ;
#4921 = ORIENTED_EDGE ( 'NONE', *, *, #55404, .T. ) ;
#4922 = CARTESIAN_POINT ( 'NONE',  ( 9.337500000000000355, -2.886751345948129988, 4.999999999999997335 ) ) ;
#4923 = CARTESIAN_POINT ( 'NONE',  ( -1.999999999999997113, 15.68750000122903465, 33.46410161513775705 ) ) ;
#4924 = CARTESIAN_POINT ( 'NONE',  ( 9.001249775931846008E-16, 15.02187500061451608, -25.09994784771203058 ) ) ;
#4925 = CARTESIAN_POINT ( 'NONE',  ( 4.153125000614515727, 0.000000000000000000, 5.243569643749999010 ) ) ;
#4926 = CARTESIAN_POINT ( 'NONE',  ( -3.756430356249999214, 15.52812499938548108, 27.83122392262697176 ) ) ;
#4927 = CARTESIAN_POINT ( 'NONE',  ( 9.074999999999999289, 6.123233995736764310E-16, -4.999999999999998224 ) ) ;
#4928 = CARTESIAN_POINT ( 'NONE',  ( 3.087067283321337730, 3.933194069486794842, 3.194874766990889903 ) ) ;
#4929 = EDGE_LOOP ( 'NONE', ( #11274, #18502, #65883, #67077 ) ) ;
#4930 = CARTESIAN_POINT ( 'NONE',  ( 24.62812500061451715, 6.421520780324663323E-16, -5.243569643749999010 ) ) ;
#4931 = CARTESIAN_POINT ( 'NONE',  ( 25.66875000122903216, -5.773502691896255534, -1.060575238724906372E-15 ) ) ;
#4932 = CARTESIAN_POINT ( 'NONE',  ( 29.44687500061451857, -3.027376345333614438, 5.243569643749998122 ) ) ;
#4933 = CARTESIAN_POINT ( 'NONE',  ( 22.58437500061451431, 4.541064518000418104, 2.621784821874999949 ) ) ;
#4934 = CARTESIAN_POINT ( 'NONE',  ( 16.64062500061451289, 6.054752690667223547, 3.707466751127219781E-16 ) ) ;
#4935 = EDGE_CURVE ( 'NONE', #51755, #8633, #30167, .T. ) ;
#4936 = CARTESIAN_POINT ( 'NONE',  ( -2.121784821874996840, 12.22812500061459495, -26.32496088578401583 ) ) ;
#4937 = CARTESIAN_POINT ( 'NONE',  ( 5.953125000614519102, 0.000000000000000000, 5.243569643749999010 ) ) ;
#4938 = CARTESIAN_POINT ( 'NONE',  ( 28.16250000122903074, 4.330127018922192761, -2.499999999999997780 ) ) ;
#4939 = CARTESIAN_POINT ( 'NONE',  ( 24.83437500061451431, 4.119189519843966529, 2.378215178124999607 ) ) ;
#4940 = CARTESIAN_POINT ( 'NONE',  ( 20.12812500061451715, 6.421520780324663323E-16, -5.243569643749999010 ) ) ;
#4941 = CARTESIAN_POINT ( 'NONE',  ( 8.634375000614518569, 4.119189519843966529, 2.378215178124999607 ) ) ;
#4942 = CARTESIAN_POINT ( 'NONE',  ( -3.756430356250000102, 17.36562499938548498, 30.00000000000000000 ) ) ;
#4943 = CARTESIAN_POINT ( 'NONE',  ( 14.10937500061451644, 0.000000000000000000, 5.243569643749999010 ) ) ;
#4944 = CARTESIAN_POINT ( 'NONE',  ( 14.70937500061451786, -4.541064518000417216, -2.621784821875001281 ) ) ;
#4945 = CARTESIAN_POINT ( 'NONE',  ( 23.25937500061451857, -4.541064518000417216, -2.621784821875001281 ) ) ;
#4946 = ORIENTED_EDGE ( 'NONE', *, *, #24217, .F. ) ;
#4947 = CARTESIAN_POINT ( 'NONE',  ( 2.121784821874999061, 12.05937500061451750, 26.32496088578401583 ) ) ;
#4948 = CARTESIAN_POINT ( 'NONE',  ( 3.065625000614517592, 3.027376345333613106, -5.243569643749998122 ) ) ;
#4949 = CARTESIAN_POINT ( 'NONE',  ( 26.50312500061451360, 4.541064518000418104, -2.621784821874998173 ) ) ;
#4950 = CARTESIAN_POINT ( 'NONE',  ( 27.81562500061452070, 3.027376345333613106, -5.243569643749998122 ) ) ;
#4951 = DIRECTION ( 'NONE',  ( -1.000000000000000000, -0.000000000000000000, -0.000000000000000000 ) ) ;
#4952 = CARTESIAN_POINT ( 'NONE',  ( 2.000000000000001332, 19.69999999999999929, 33.46410161513774995 ) ) ;
#4953 = CARTESIAN_POINT ( 'NONE',  ( 5.934375000614517504, 4.541064518000418104, 2.621784821874999949 ) ) ;
#4954 = CARTESIAN_POINT ( 'NONE',  ( 12.52500000122903145, 2.886751345948126879, 4.999999999999999112 ) ) ;
#4955 = CARTESIAN_POINT ( 'NONE',  ( 9.187500001229034652, 6.123233995736764310E-16, -4.999999999999998224 ) ) ;
#4956 = CARTESIAN_POINT ( 'NONE',  ( 28.72500000122903074, 2.886751345948126879, 4.999999999999999112 ) ) ;
#4957 = CARTESIAN_POINT ( 'NONE',  ( -4.000000000000000000, 14.91874999877096641, 30.00000000000000000 ) ) ;
#4958 = CARTESIAN_POINT ( 'NONE',  ( 19.33125000122903359, -4.330127018922194537, 2.499999999999995559 ) ) ;
#4959 = CARTESIAN_POINT ( 'NONE',  ( 11.85937500061451644, 0.000000000000000000, 5.243569643749999010 ) ) ;
#4960 = CARTESIAN_POINT ( 'NONE',  ( 29.60625000122903216, 0.000000000000000000, 4.999999999999998224 ) ) ;
#4961 = ORIENTED_EDGE ( 'NONE', *, *, #66576, .T. ) ;
#4962 = CARTESIAN_POINT ( 'NONE',  ( 20.91562500061451502, -6.054752690667223547, -1.112240025338166033E-15 ) ) ;
#4963 = CARTESIAN_POINT ( 'NONE',  ( 12.19687500061451679, 6.054752690667223547, 3.707466751127219781E-16 ) ) ;
#4964 = CARTESIAN_POINT ( 'NONE',  ( 5.990625000614517859, -3.027376345333614438, 5.243569643749998122 ) ) ;
#4965 = CARTESIAN_POINT ( 'NONE',  ( 21.30937500061451573, 0.000000000000000000, 5.243569643749999010 ) ) ;
#4966 = CARTESIAN_POINT ( 'NONE',  ( 4.828125000614518214, 6.421520780324663323E-16, -5.243569643749999010 ) ) ;
#4967 = DIRECTION ( 'NONE',  ( 0.000000000000000000, 0.000000000000000000, 1.000000000000000000 ) ) ;
#4968 = CARTESIAN_POINT ( 'NONE',  ( 6.862500001229034474, -4.330127018922190985, -2.500000000000001332 ) ) ;
#4969 = CARTESIAN_POINT ( 'NONE',  ( 20.46562500061451928, -6.054752690667223547, -1.112240025338166033E-15 ) ) ;
#4970 = CARTESIAN_POINT ( 'NONE',  ( 8.062500001229034652, 0.000000000000000000, 4.999999999999998224 ) ) ;
#4971 = CARTESIAN_POINT ( 'NONE',  ( 16.26562500061451289, 3.027376345333611329, 5.243569643749999010 ) ) ;
#4972 = CARTESIAN_POINT ( 'NONE',  ( 16.52812500061451573, 6.421520780324663323E-16, -5.243569643749999010 ) ) ;
#4973 = CARTESIAN_POINT ( 'NONE',  ( 25.58437500061451431, 5.824947211148865298E-16, -4.756430356249998326 ) ) ;
#4974 = CARTESIAN_POINT ( 'NONE',  ( 15.52500000000000036, 4.330127018922191873, 2.499999999999999556 ) ) ;
#4975 = CARTESIAN_POINT ( 'NONE',  ( 11.28750000122903252, -4.330127018922194537, 2.499999999999995559 ) ) ;
#4976 = CARTESIAN_POINT ( 'NONE',  ( 6.928125000614516082, -4.541064518000419881, 2.621784821874995952 ) ) ;
#4977 = APPLICATION_CONTEXT ( 'automotive_design' ) ;
#4978 = CARTESIAN_POINT ( 'NONE',  ( 10.60312500061451679, -4.541064518000417216, -2.621784821875001281 ) ) ;
#4979 = AXIS2_PLACEMENT_3D ( 'NONE', #66658, #72559, #10505 ) ;
#4980 = CARTESIAN_POINT ( 'NONE',  ( 21.82500000122903572, 2.886751345948129099, -4.999999999999998224 ) ) ;
#4981 = CARTESIAN_POINT ( 'NONE',  ( -4.243569643749999898, 12.62187500061451928, -32.45002607614398471 ) ) ;
#4982 = CARTESIAN_POINT ( 'NONE',  ( 4.629056002857023344, -1.889931353889065413, 4.891133006415133266 ) ) ;
#4983 = CARTESIAN_POINT ( 'NONE',  ( 4.462500001229035007, 0.000000000000000000, 4.999999999999998224 ) ) ;
#4984 = CARTESIAN_POINT ( 'NONE',  ( 2.934375000614518392, -4.541064518000419881, 2.621784821874995952 ) ) ;
#4985 = CARTESIAN_POINT ( 'NONE',  ( 21.98437500061451644, 6.421520780324663323E-16, -5.243569643749999010 ) ) ;
#4986 = CARTESIAN_POINT ( 'NONE',  ( 12.22499999999999964, 6.123233995736764310E-16, -4.999999999999998224 ) ) ;
#4987 = CARTESIAN_POINT ( 'NONE',  ( 16.52812500061451573, 6.421520780324663323E-16, -5.243569643749999010 ) ) ;
#4988 = CARTESIAN_POINT ( 'NONE',  ( 12.80625000122903323, 4.330127018922192761, -2.499999999999997780 ) ) ;
#4989 = CARTESIAN_POINT ( 'NONE',  ( 10.98750000000000071, 5.773502691896255534, 3.535250795749688401E-16 ) ) ;
#4990 = CARTESIAN_POINT ( 'NONE',  ( 34.99999999999999289, 0.000000000000000000, 0.000000000000000000 ) ) ;
#4991 = CARTESIAN_POINT ( 'NONE',  ( 28.80937500061451573, 4.541064518000418104, -2.621784821874998173 ) ) ;
#4992 = CARTESIAN_POINT ( 'NONE',  ( 21.49687500061451573, 4.119189519843966529, -2.378215178124998275 ) ) ;
#4993 = CARTESIAN_POINT ( 'NONE',  ( 15.02812500061451750, -4.541064518000419881, 2.621784821874995952 ) ) ;
#4994 = CARTESIAN_POINT ( 'NONE',  ( 13.84687500061451537, -3.027376345333610441, -5.243569643749999898 ) ) ;
#4995 = VERTEX_POINT ( 'NONE', #71335 ) ;
#4996 = CARTESIAN_POINT ( 'NONE',  ( 22.46250000122903501, 0.000000000000000000, 4.999999999999998224 ) ) ;
#4997 = CARTESIAN_POINT ( 'NONE',  ( 21.66562500061451502, 3.027376345333611329, 5.243569643749999010 ) ) ;
#4998 = CARTESIAN_POINT ( 'NONE',  ( 45.00000000000000000, 0.000000000000000000, 0.000000000000000000 ) ) ;
#4999 = CARTESIAN_POINT ( 'NONE',  ( 14.51250000000000107, 2.886751345948129099, -4.999999999999997335 ) ) ;
#5000 = CARTESIAN_POINT ( 'NONE',  ( 12.59999999999999964, -4.330127018922190985, -2.500000000000001332 ) ) ;
#5001 = CARTESIAN_POINT ( 'NONE',  ( 20.58750000122903145, 4.330127018922191873, 2.499999999999999556 ) ) ;
#5002 = CARTESIAN_POINT ( 'NONE',  ( 15.92812500061451608, -4.541064518000419881, 2.621784821874995952 ) ) ;
#5003 = CARTESIAN_POINT ( 'NONE',  ( 13.62187500061451750, -4.119189519843968306, 2.378215178124996054 ) ) ;
#5004 = ORIENTED_EDGE ( 'NONE', *, *, #39247, .F. ) ;
#5005 = CARTESIAN_POINT ( 'NONE',  ( 18.89999999999999858, -4.330127018922190985, -2.500000000000001332 ) ) ;
#5006 = CARTESIAN_POINT ( 'NONE',  ( 21.00937500061451857, -4.541064518000417216, -2.621784821875001281 ) ) ;
#5007 = CARTESIAN_POINT ( 'NONE',  ( 28.67812500061451431, 6.421520780324663323E-16, -5.243569643749999010 ) ) ;
#5008 = VERTEX_POINT ( 'NONE', #49902 ) ;
#5009 = CARTESIAN_POINT ( 'NONE',  ( 19.91250000000000142, 2.886751345948129099, -4.999999999999997335 ) ) ;
#5010 = CARTESIAN_POINT ( 'NONE',  ( 9.703125000614514661, -4.541064518000417216, -2.621784821875001281 ) ) ;
#5011 = LINE ( 'NONE', #28271, #13668 ) ;
#5012 = CARTESIAN_POINT ( 'NONE',  ( 14.70937500061451431, 2.746126346562645981, -4.756430356249997438 ) ) ;
#5013 = CARTESIAN_POINT ( 'NONE',  ( 16.64999999999999858, -4.330127018922190985, -2.500000000000001332 ) ) ;
#5014 = CARTESIAN_POINT ( 'NONE',  ( 23.51249999999999574, 2.886751345948129099, -4.999999999999998224 ) ) ;
#5015 = CARTESIAN_POINT ( 'NONE',  ( -4.243569643749999898, 19.76562500061451644, 27.54997392385601529 ) ) ;
#5016 = CARTESIAN_POINT ( 'NONE',  ( 3.384375000614517237, -4.541064518000419881, 2.621784821874995952 ) ) ;
#5017 = CARTESIAN_POINT ( 'NONE',  ( 29.33437500061451431, 4.541064518000418104, 2.621784821874999949 ) ) ;
#5018 = ORIENTED_EDGE ( 'NONE', *, *, #56586, .F. ) ;
#5019 = CARTESIAN_POINT ( 'NONE',  ( 24.21562500061451573, 3.027376345333613106, -5.243569643749998122 ) ) ;
#5020 = CARTESIAN_POINT ( 'NONE',  ( 25.92187500061451999, -6.054752690667223547, -1.112240025338166033E-15 ) ) ;
#5021 = CARTESIAN_POINT ( 'NONE',  ( 2.121784821875001281, 19.05312500061459247, -26.32496088578401938 ) ) ;
#5022 = CARTESIAN_POINT ( 'NONE',  ( 13.95000000000000107, -4.330127018922190985, -2.500000000000001332 ) ) ;
#5023 = CARTESIAN_POINT ( 'NONE',  ( 12.36562500061451608, -6.054752690667223547, -1.112240025338166033E-15 ) ) ;
#5024 = CARTESIAN_POINT ( 'NONE',  ( 25.82812500061451644, -4.541064518000419881, 2.621784821874995952 ) ) ;
#5025 = CARTESIAN_POINT ( 'NONE',  ( 16.80000000122903359, -2.886751345948125991, -5.000000000000000000 ) ) ;
#5026 = CARTESIAN_POINT ( 'NONE',  ( 14.70937500061451786, -4.119189519843965641, -2.378215178125001383 ) ) ;
#5027 = CARTESIAN_POINT ( 'NONE',  ( 2.840625000614518392, -3.027376345333614438, 5.243569643749998122 ) ) ;
#5028 = CARTESIAN_POINT ( 'NONE',  ( 21.79687500061451644, -3.027376345333614438, 5.243569643749998122 ) ) ;
#5030 = CARTESIAN_POINT ( 'NONE',  ( -4.243569643749999898, 15.35937500061451644, 30.00000000000000000 ) ) ;
#5029 =( BOUNDED_CURVE ( )  B_SPLINE_CURVE ( 2, ( #64835, #20119, #59278, #43777, #15317, #71852, #66304 ),
 .UNSPECIFIED., .F., .F. ) 
 B_SPLINE_CURVE_WITH_KNOTS ( ( 3, 2, 2, 3 ),
 ( 0.9799999999999999822, 0.9833333333333333925, 0.9866666666666668029, 0.9900000000000002132 ),
 .UNSPECIFIED. ) 
 CURVE ( )  GEOMETRIC_REPRESENTATION_ITEM ( )  RATIONAL_B_SPLINE_CURVE ( ( 1.000000000000000000, 0.8660254037844387076, 1.000000000000000000, 0.8660254037844387076, 1.000000000000000000, 0.8660254037844298258, 1.000000000000008882 ) ) 
 REPRESENTATION_ITEM ( '' )  );
#5031 = CARTESIAN_POINT ( 'NONE',  ( 22.05937500061451573, 4.541064518000418104, -2.621784821874998173 ) ) ;
#5032 = CARTESIAN_POINT ( 'NONE',  ( 29.10937500061451644, -4.541064518000417216, -2.621784821875001281 ) ) ;
#5033 = CARTESIAN_POINT ( 'NONE',  ( 10.61250000000000071, 2.886751345948238789, 4.999999999999807265 ) ) ;
#5034 = CARTESIAN_POINT ( 'NONE',  ( 9.065625000614517148, 3.027376345333611329, 5.243569643749999010 ) ) ;
#5035 = CARTESIAN_POINT ( 'NONE',  ( 30.00000000000000000, 0.000000000000000000, 0.000000000000000000 ) ) ;
#5036 = AXIS2_PLACEMENT_3D ( 'NONE', #55619, #21994, #32722 ) ;
#5037 = CARTESIAN_POINT ( 'NONE',  ( 7.284375000614518036, 4.541064518000418104, 2.621784821874999949 ) ) ;
#5038 = CARTESIAN_POINT ( 'NONE',  ( 14.13750000122903394, 6.123233995736764310E-16, -4.999999999999998224 ) ) ;
#5039 = CARTESIAN_POINT ( 'NONE',  ( 7.790625000614518569, -3.027376345333614438, 5.243569643749998122 ) ) ;
#5040 = CARTESIAN_POINT ( 'NONE',  ( 12.98437500061451821, 6.421520780324663323E-16, -5.243569643749999010 ) ) ;
#5041 = LINE ( 'NONE', #37187, #56939 ) ;
#5042 = CARTESIAN_POINT ( 'NONE',  ( 19.46250000122903145, -4.330127018922190985, -2.500000000000001332 ) ) ;
#5043 = CARTESIAN_POINT ( 'NONE',  ( 6.871875000614517504, 3.027376345333611329, 5.243569643749999010 ) ) ;
#5044 = CARTESIAN_POINT ( 'NONE',  ( 10.41562500061451679, 3.027376345333611329, 5.243569643749999010 ) ) ;
#5045 = CARTESIAN_POINT ( 'NONE',  ( 7.040625000614517681, -3.027376345333610441, -5.243569643749999898 ) ) ;
#5046 = CARTESIAN_POINT ( 'NONE',  ( 26.15625000122903288, -4.330127018922190985, -2.500000000000001332 ) ) ;
#5047 = CARTESIAN_POINT ( 'NONE',  ( 18.49687500061452283, 6.054752690667223547, 3.707466751127219781E-16 ) ) ;
#5048 = CARTESIAN_POINT ( 'NONE',  ( 4.575260086717170438, 2.016679235498957112, 4.840250765194281435 ) ) ;
#5049 = CARTESIAN_POINT ( 'NONE',  ( 12.59062500061451573, 6.054752690667223547, 3.707466751127219781E-16 ) ) ;
#5050 = CARTESIAN_POINT ( 'NONE',  ( 29.63437500061451502, 6.421520780324663323E-16, -5.243569643749999010 ) ) ;
#5051 = CARTESIAN_POINT ( 'NONE',  ( 4.243569643749999010, 12.92187500061451999, -32.45002607614398471 ) ) ;
#5052 = CARTESIAN_POINT ( 'NONE',  ( 13.76250000122903394, 4.330127018922192761, -2.499999999999997780 ) ) ;
#5053 = CARTESIAN_POINT ( 'NONE',  ( -4.243569643749997233, 15.34062500061451750, -27.54997392385601174 ) ) ;
#5054 = CARTESIAN_POINT ( 'NONE',  ( 15.48750000122903359, 6.123233995736764310E-16, -4.999999999999998224 ) ) ;
#5055 = CARTESIAN_POINT ( 'NONE',  ( 11.31562500061451892, 3.027376345333611329, 5.243569643749999010 ) ) ;
#5056 = ORIENTED_EDGE ( 'NONE', *, *, #30947, .F. ) ;
#5057 = CARTESIAN_POINT ( 'NONE',  ( 14.13750000000000107, 5.773502691896255534, 3.535250795749688894E-16 ) ) ;
#5058 = DIRECTION ( 'NONE',  ( -0.000000000000000000, -1.000000000000000000, -0.000000000000000000 ) ) ;
#5059 = CARTESIAN_POINT ( 'NONE',  ( 22.86562500061451431, 3.027376345333613106, -5.243569643749998122 ) ) ;
#5060 = CARTESIAN_POINT ( 'NONE',  ( 6.946875000614517681, -3.027376345333614438, 5.243569643749998122 ) ) ;
#5061 = CARTESIAN_POINT ( 'NONE',  ( 11.36250000122903536, -4.330127018922190985, -2.500000000000001332 ) ) ;
#5062 = ADVANCED_FACE ( 'NONE', ( #15901 ), #72426, .T. ) ;
#5063 = CARTESIAN_POINT ( 'NONE',  ( 19.08750000122903145, 6.123233995736764310E-16, -4.999999999999998224 ) ) ;
#5064 = CARTESIAN_POINT ( 'NONE',  ( 14.84062500061451750, 6.054752690667223547, 3.707466751127219781E-16 ) ) ;
#5065 = CARTESIAN_POINT ( 'NONE',  ( 17.61562500061451786, 3.027376345333611329, 5.243569643749999010 ) ) ;
#5066 = CARTESIAN_POINT ( 'NONE',  ( 25.42500000122903359, 2.886751345948129099, -4.999999999999998224 ) ) ;
#5067 = EDGE_CURVE ( 'NONE', #33154, #22800, #15171, .T. ) ;
#5068 = CARTESIAN_POINT ( 'NONE',  ( 28.80000000122903003, -2.886751345948129988, 4.999999999999997335 ) ) ;
#5069 = CARTESIAN_POINT ( 'NONE',  ( 23.92499999999999716, 6.123233995736764310E-16, -4.999999999999998224 ) ) ;
#5070 = CARTESIAN_POINT ( 'NONE',  ( -1.878215178124999163, 14.14062499938548356, 26.74683588394047007 ) ) ;
#5071 = CARTESIAN_POINT ( 'NONE',  ( 25.47187500061451715, -6.054752690667223547, -1.112240025338166033E-15 ) ) ;
#5072 = CARTESIAN_POINT ( 'NONE',  ( 18.30000000122903359, 5.773502691896255534, 3.535250795749688401E-16 ) ) ;
#5073 = CARTESIAN_POINT ( 'NONE',  ( 13.57500000122903572, -5.773502691896255534, -1.060575238724906372E-15 ) ) ;
#5074 = CARTESIAN_POINT ( 'NONE',  ( 28.35937500061451289, 4.541064518000418104, -2.621784821874998173 ) ) ;
#5075 =( BOUNDED_CURVE ( )  B_SPLINE_CURVE ( 2, ( #52866, #42515, #65039, #24419, #18864, #35508, #14430 ),
 .UNSPECIFIED., .F., .F. ) 
 B_SPLINE_CURVE_WITH_KNOTS ( ( 3, 2, 2, 3 ),
 ( 0.3083333333333333481, 0.3111111111111111160, 0.3138888888888888840, 0.3166666666666666519 ),
 .UNSPECIFIED. ) 
 CURVE ( )  GEOMETRIC_REPRESENTATION_ITEM ( )  RATIONAL_B_SPLINE_CURVE ( ( 1.000000000000000000, 0.8660254037844387076, 1.000000000000000000, 0.8660254037844387076, 1.000000000000000000, 0.8660254037844387076, 1.000000000000000000 ) ) 
 REPRESENTATION_ITEM ( '' )  );
#5076 = DIRECTION ( 'NONE',  ( 0.000000000000000000, -1.000000000000000000, 8.673617379884035472E-17 ) ) ;
#5077 = CARTESIAN_POINT ( 'NONE',  ( 5.109375000614518214, 0.000000000000000000, 5.243569643749999010 ) ) ;
#5078 = CARTESIAN_POINT ( 'NONE',  ( 23.65312500061451573, -4.541064518000417216, -2.621784821875001281 ) ) ;
#5079 = CARTESIAN_POINT ( 'NONE',  ( 1.878215178124997609, 14.02812499938548285, 33.25316411605952993 ) ) ;
#5080 = CARTESIAN_POINT ( 'NONE',  ( 10.17187500061451999, -6.054752690667223547, -1.112240025338166033E-15 ) ) ;
#5081 = DIRECTION ( 'NONE',  ( -1.000000000000000000, -0.000000000000000000, -0.000000000000000000 ) ) ;
#5082 = CARTESIAN_POINT ( 'NONE',  ( 29.65312500061451573, 4.541064518000418104, -2.621784821874998173 ) ) ;
#5083 = CARTESIAN_POINT ( 'NONE',  ( 5.859375000614519102, 4.541064518000418104, -2.621784821874998173 ) ) ;
#5084 = CARTESIAN_POINT ( 'NONE',  ( 28.84687500061452070, 6.054752690667223547, 3.707466751127219781E-16 ) ) ;
#5085 = DIRECTION ( 'NONE',  ( -1.000000000000000000, -0.000000000000000000, -0.000000000000000000 ) ) ;
#5086 = CARTESIAN_POINT ( 'NONE',  ( 18.78749999999999432, -2.886751345948129988, 4.999999999999997335 ) ) ;
#5087 = ORIENTED_EDGE ( 'NONE', *, *, #33984, .T. ) ;
#5088 = CARTESIAN_POINT ( 'NONE',  ( 28.08749999999999858, 5.773502691896255534, 3.535250795749688894E-16 ) ) ;
#5089 = CARTESIAN_POINT ( 'NONE',  ( 28.17187500061451644, -6.054752690667223547, -1.112240025338166033E-15 ) ) ;
#5090 = ORIENTED_EDGE ( 'NONE', *, *, #66497, .F. ) ;
#5091 = CARTESIAN_POINT ( 'NONE',  ( 18.44062500061451715, 6.054752690667223547, 3.707466751127219781E-16 ) ) ;
#5092 = CARTESIAN_POINT ( 'NONE',  ( 8.428125000614517859, 6.421520780324663323E-16, -5.243569643749999010 ) ) ;
#5093 = CARTESIAN_POINT ( 'NONE',  ( 22.02187500061451431, 4.119189519843966529, 2.378215178124999607 ) ) ;
#5094 = CARTESIAN_POINT ( 'NONE',  ( 4.096875000614518925, 6.054752690667223547, 3.707466751127219781E-16 ) ) ;
#5095 = CARTESIAN_POINT ( 'NONE',  ( 17.70000000122903216, -2.886751345948125991, -5.000000000000000000 ) ) ;
#5096 = CARTESIAN_POINT ( 'NONE',  ( 4.000000000000000000, 13.88750000000000107, -27.69059892324149885 ) ) ;
#5097 = CARTESIAN_POINT ( 'NONE',  ( 6.384375000614516793, 4.541064518000418104, 2.621784821874999949 ) ) ;
#5098 = CARTESIAN_POINT ( 'NONE',  ( 11.03437500061451715, -4.541064518000419881, 2.621784821874995952 ) ) ;
#5099 = CARTESIAN_POINT ( 'NONE',  ( 20.70937500061451786, 4.541064518000418104, -2.621784821874998173 ) ) ;
#5100 = FACE_OUTER_BOUND ( 'NONE', #43855, .T. ) ;
#5101 = VERTEX_POINT ( 'NONE', #66900 ) ;
#5102 = CARTESIAN_POINT ( 'NONE',  ( 11.40000000000000036, 4.330127018922192761, -2.499999999999997780 ) ) ;
#5103 = CARTESIAN_POINT ( 'NONE',  ( 18.60937500061451644, 0.000000000000000000, 5.243569643749999010 ) ) ;
#5104 = CARTESIAN_POINT ( 'NONE',  ( 10.32187500061451679, 3.027376345333613106, -5.243569643749998122 ) ) ;
#5105 = CARTESIAN_POINT ( 'NONE',  ( -1.878215178125001827, 15.19062499938548427, 33.25316411605952283 ) ) ;
#5106 = CARTESIAN_POINT ( 'NONE',  ( 20.66250000000000142, -5.773502691896255534, -1.060575238724906372E-15 ) ) ;
#5107 = CARTESIAN_POINT ( 'NONE',  ( 18.21562500061451573, -6.054752690667223547, -1.112240025338166033E-15 ) ) ;
#5108 = CARTESIAN_POINT ( 'NONE',  ( 2.828200636599751609E-16, 17.56250000000000000, 25.38119784648299415 ) ) ;
#5109 = CARTESIAN_POINT ( 'NONE',  ( -0.7368805616696193495, 9.859898480082234684, -34.17910162106521454 ) ) ;
#5110 = CARTESIAN_POINT ( 'NONE',  ( 22.43437500061451573, 5.824947211148865298E-16, -4.756430356249998326 ) ) ;
#5111 = CARTESIAN_POINT ( 'NONE',  ( 12.92812500061451786, 6.421520780324663323E-16, -5.243569643749999010 ) ) ;
#5112 = CARTESIAN_POINT ( 'NONE',  ( 29.07187500061451502, -6.054752690667223547, -1.112240025338166033E-15 ) ) ;
#5113 = CYLINDRICAL_SURFACE ( 'NONE', #5401, 3.999999999999996447 ) ;
#5114 = CARTESIAN_POINT ( 'NONE',  ( 28.84687500061452070, 6.054752690667223547, 3.707466751127219781E-16 ) ) ;
#5115 = CARTESIAN_POINT ( 'NONE',  ( 9.449999999999999289, -4.330127018922190985, -2.500000000000001332 ) ) ;
#5116 = CARTESIAN_POINT ( 'NONE',  ( 3.999999999999998668, 14.97500000122903430, 27.69059892324149175 ) ) ;
#5117 = CARTESIAN_POINT ( 'NONE',  ( 9.937500001229032875, -4.330127018922194537, 2.499999999999995559 ) ) ;
#5118 = CARTESIAN_POINT ( 'NONE',  ( 19.58437500061451786, -4.541064518000419881, 2.621784821874995952 ) ) ;
#5119 = CARTESIAN_POINT ( 'NONE',  ( 15.23437500061451644, 6.421520780324663323E-16, -5.243569643749999010 ) ) ;
#5120 = FACE_OUTER_BOUND ( 'NONE', #62854, .T. ) ;
#5121 = ORIENTED_EDGE ( 'NONE', *, *, #30962, .T. ) ;
#5122 = CARTESIAN_POINT ( 'NONE',  ( 14.87812500061451537, 4.541064518000418104, 2.621784821874999949 ) ) ;
#5123 = CARTESIAN_POINT ( 'NONE',  ( 28.91250000122903074, -4.330127018922190985, -2.500000000000001332 ) ) ;
#5124 = CARTESIAN_POINT ( 'NONE',  ( 14.48437500061451821, 4.541064518000418104, 2.621784821874999949 ) ) ;
#5125 = CARTESIAN_POINT ( 'NONE',  ( 3.028125000614518392, 6.421520780324663323E-16, -5.243569643749999010 ) ) ;
#5126 = CARTESIAN_POINT ( 'NONE',  ( 16.26562500061451289, 3.027376345333611329, 5.243569643749999010 ) ) ;
#5127 = FACE_OUTER_BOUND ( 'NONE', #9234, .T. ) ;
#5128 = CARTESIAN_POINT ( 'NONE',  ( 26.97187500061451360, 3.027376345333613106, -5.243569643749998122 ) ) ;
#5129 = FACE_OUTER_BOUND ( 'NONE', #7076, .T. ) ;
#5130 = CARTESIAN_POINT ( 'NONE',  ( 15.34687500061451537, 6.054752690667223547, 3.707466751127219781E-16 ) ) ;
#5131 = CARTESIAN_POINT ( 'NONE',  ( 13.23750000122903359, 6.123233995736764310E-16, -4.999999999999998224 ) ) ;
#5132 = CARTESIAN_POINT ( 'NONE',  ( 9.084375000614517859, 4.119189519843966529, 2.378215178124999607 ) ) ;
#5133 = CARTESIAN_POINT ( 'NONE',  ( -4.243569643749999898, 19.82187500061451857, -32.45002607614398471 ) ) ;
#5134 = CARTESIAN_POINT ( 'NONE',  ( 21.23437500061451644, 4.541064518000418104, 2.621784821874999949 ) ) ;
#5135 = CARTESIAN_POINT ( 'NONE',  ( 21.71250000122903501, -4.330127018922190985, -2.500000000000001332 ) ) ;
#5136 = CARTESIAN_POINT ( 'NONE',  ( 18.23437500061451999, -4.541064518000419881, 2.621784821874995952 ) ) ;
#5137 = CARTESIAN_POINT ( 'NONE',  ( 4.243569643749999010, 11.57187500061451679, 27.54997392385601174 ) ) ;
#5138 = CARTESIAN_POINT ( 'NONE',  ( 17.84062500061451573, -3.027376345333610441, -5.243569643749999898 ) ) ;
#5139 = ORIENTED_EDGE ( 'NONE', *, *, #28806, .F. ) ;
#5140 = VERTEX_POINT ( 'NONE', #55806 ) ;
#5141 = CARTESIAN_POINT ( 'NONE',  ( 20.66250000000000142, -5.773502691896255534, -1.060575238724906372E-15 ) ) ;
#5142 = CARTESIAN_POINT ( 'NONE',  ( 28.16250000122903074, 4.330127018922192761, -2.499999999999997780 ) ) ;
#5143 = CARTESIAN_POINT ( 'NONE',  ( 23.72812500061451502, 6.421520780324663323E-16, -5.243569643749999010 ) ) ;
#5144 = CARTESIAN_POINT ( 'NONE',  ( 4.415625000614518569, 3.027376345333613106, -5.243569643749998122 ) ) ;
#5145 = CARTESIAN_POINT ( 'NONE',  ( 16.35000000122903430, -2.886751345948125991, -5.000000000000000000 ) ) ;
#5146 = CARTESIAN_POINT ( 'NONE',  ( 22.30312500061451431, -4.541064518000417216, -2.621784821875001281 ) ) ;
#5147 = CARTESIAN_POINT ( 'NONE',  ( 21.37499999999999645, 4.330127018922191873, 2.499999999999999556 ) ) ;
#5148 = CARTESIAN_POINT ( 'NONE',  ( 26.31562500061451715, -6.054752690667223547, -1.112240025338166033E-15 ) ) ;
#5149 = CARTESIAN_POINT ( 'NONE',  ( 4.903125000614516615, 4.541064518000418104, -2.621784821874998173 ) ) ;
#5150 = ORIENTED_EDGE ( 'NONE', *, *, #7878, .T. ) ;
#5151 = EDGE_CURVE ( 'NONE', #21883, #44291, #71709, .T. ) ;
#5152 = CARTESIAN_POINT ( 'NONE',  ( 29.62500000000000000, -4.330127018922194537, 2.499999999999995559 ) ) ;
#5153 = CARTESIAN_POINT ( 'NONE',  ( 3.703125000614516882, 0.000000000000000000, 5.243569643749999010 ) ) ;
#5154 = CARTESIAN_POINT ( 'NONE',  ( 12.38437500061451857, -4.119189519843968306, 2.378215178124996054 ) ) ;
#5155 = CARTESIAN_POINT ( 'NONE',  ( 3.999999999999998668, 18.91249999999999787, 27.69059892324149530 ) ) ;
#5156 = CARTESIAN_POINT ( 'NONE',  ( 3.999999999999998668, 11.82500000122903572, -32.30940107675850470 ) ) ;
#5157 = CARTESIAN_POINT ( 'NONE',  ( 9.001249775931846008E-16, 17.72187500061451715, -25.09994784771203058 ) ) ;
#5158 = CARTESIAN_POINT ( 'NONE',  ( 9.337500000000000355, -2.886751345948129988, 4.999999999999997335 ) ) ;
#5159 = CARTESIAN_POINT ( 'NONE',  ( 9.984375000614518214, 4.541064518000418104, 2.621784821874999949 ) ) ;
#5160 = CARTESIAN_POINT ( 'NONE',  ( 7.537500001229033408, 4.330127018922191873, 2.499999999999999556 ) ) ;
#5161 = CARTESIAN_POINT ( 'NONE',  ( 12.57187500061451857, 3.027376345333613106, -5.243569643749998122 ) ) ;
#5162 = LINE ( 'NONE', #8236, #11193 ) ;
#5163 = CARTESIAN_POINT ( 'NONE',  ( 3.196875000614516793, 6.054752690667223547, 3.707466751127219781E-16 ) ) ;
#5164 = CARTESIAN_POINT ( 'NONE',  ( 45.00000000000000000, 6.123233995736764310E-16, -4.999999999999998224 ) ) ;
#5165 = CARTESIAN_POINT ( 'NONE',  ( 45.00000000000000000, 0.000000000000000000, 0.000000000000000000 ) ) ;
#5166 = CARTESIAN_POINT ( 'NONE',  ( 9.084375000614517859, 4.541064518000418104, 2.621784821874999949 ) ) ;
#5167 = CARTESIAN_POINT ( 'NONE',  ( 1.626862140677534273E-15, 13.92500000122903181, -26.00000000000000355 ) ) ;
#5168 = CARTESIAN_POINT ( 'NONE',  ( 19.07812500061451644, -4.541064518000419881, 2.621784821874995952 ) ) ;
#5169 = DIRECTION ( 'NONE',  ( -1.000000000000000000, -0.000000000000000000, -0.000000000000000000 ) ) ;
#5170 = CARTESIAN_POINT ( 'NONE',  ( 9.001249775931846008E-16, 18.11562500061459602, 34.90005215228797653 ) ) ;
#5171 = CARTESIAN_POINT ( 'NONE',  ( 23.82187500061451502, 3.027376345333613106, -5.243569643749998122 ) ) ;
#5172 = LINE ( 'NONE', #34318, #31635 ) ;
#5173 = CARTESIAN_POINT ( 'NONE',  ( 2.878125000614517592, -4.541064518000419881, 2.621784821874995952 ) ) ;
#5174 = CARTESIAN_POINT ( 'NONE',  ( 20.63437500061451502, 5.492252693125287522, 3.363034840372157021E-16 ) ) ;
#5175 = CARTESIAN_POINT ( 'NONE',  ( 24.92812500061451431, -4.541064518000419881, 2.621784821874995952 ) ) ;
#5176 = CARTESIAN_POINT ( 'NONE',  ( 15.81562500061451537, 3.027376345333611329, 5.243569643749999010 ) ) ;
#5177 = CARTESIAN_POINT ( 'NONE',  ( 13.33125000122903359, 4.330127018922191873, 2.499999999999999556 ) ) ;
#5178 = CARTESIAN_POINT ( 'NONE',  ( 13.28437500061451715, -4.541064518000419881, 2.621784821874995952 ) ) ;
#5179 = CARTESIAN_POINT ( 'NONE',  ( 25.01250000122903216, 4.330127018922192761, -2.499999999999997780 ) ) ;
#5180 = CARTESIAN_POINT ( 'NONE',  ( 3.946875000614517681, -3.027376345333610441, -5.243569643749999898 ) ) ;
#5181 = CARTESIAN_POINT ( 'NONE',  ( 13.32187500061451502, -6.054752690667223547, -1.112240025338166033E-15 ) ) ;
#5182 = CARTESIAN_POINT ( 'NONE',  ( -1.071796769724488563, 11.99240381056766758, 34.00000000000000000 ) ) ;
#5183 = DIRECTION ( 'NONE',  ( -1.000000000000000000, -0.000000000000000000, -0.000000000000000000 ) ) ;
#5184 = CARTESIAN_POINT ( 'NONE',  ( -2.000000000000000000, 11.93750000122903465, 26.53589838486224650 ) ) ;
#5185 = CARTESIAN_POINT ( 'NONE',  ( 24.90937500061451715, 0.000000000000000000, 5.243569643749999010 ) ) ;
#5186 = CARTESIAN_POINT ( 'NONE',  ( 16.32187500061451502, 3.027376345333611329, 5.243569643749999010 ) ) ;
#5187 = CARTESIAN_POINT ( 'NONE',  ( -1.878215178124999163, 15.60312499938548392, 26.74683588394047007 ) ) ;
#5188 = CARTESIAN_POINT ( 'NONE',  ( 28.57499999999999929, 4.330127018922191873, 2.499999999999999556 ) ) ;
#5189 = CARTESIAN_POINT ( 'NONE',  ( 4.462500001229035007, 0.000000000000000000, 4.999999999999998224 ) ) ;
#5190 = CARTESIAN_POINT ( 'NONE',  ( 5.212500000000002132, 2.886751345948126879, 4.999999999999999112 ) ) ;
#5191 = CARTESIAN_POINT ( 'NONE',  ( 29.48437500061451644, -4.119189519843968306, 2.378215178124996054 ) ) ;
#5192 = CARTESIAN_POINT ( 'NONE',  ( 18.62812500061451715, -4.541064518000419881, 2.621784821874995952 ) ) ;
#5193 = CARTESIAN_POINT ( 'NONE',  ( 9.712500000000002132, 2.886751345948126879, 4.999999999999999112 ) ) ;
#5194 = CARTESIAN_POINT ( 'NONE',  ( 17.62500000000000000, 6.123233995736764310E-16, -4.999999999999998224 ) ) ;
#5195 = CARTESIAN_POINT ( 'NONE',  ( 19.87500000122903288, -5.773502691896255534, -1.060575238724906372E-15 ) ) ;
#5196 = CARTESIAN_POINT ( 'NONE',  ( -3.999999999999997335, 10.13750000000000284, -27.69059892324149530 ) ) ;
#5197 = CARTESIAN_POINT ( 'NONE',  ( 27.90937500061451715, 4.541064518000418104, -2.621784821874998173 ) ) ;
#5198 = ORIENTED_EDGE ( 'NONE', *, *, #3972, .F. ) ;
#5199 = CARTESIAN_POINT ( 'NONE',  ( 18.02812500061451573, 4.541064518000418104, 2.621784821874999949 ) ) ;
#5200 = CARTESIAN_POINT ( 'NONE',  ( 21.06562500061451715, 3.027376345333613106, -5.243569643749998122 ) ) ;
#5201 = CARTESIAN_POINT ( 'NONE',  ( 22.77187500061451786, -6.054752690667223547, -1.112240025338166033E-15 ) ) ;
#5202 = CARTESIAN_POINT ( 'NONE',  ( 5.512499999999999289, 2.886751345948129099, -4.999999999999998224 ) ) ;
#5203 = CARTESIAN_POINT ( 'NONE',  ( 9.253125000614517148, -4.541064518000417216, -2.621784821875001281 ) ) ;
#5204 = CARTESIAN_POINT ( 'NONE',  ( 23.76562500061451644, 3.027376345333613106, -5.243569643749998122 ) ) ;
#5205 = CARTESIAN_POINT ( 'NONE',  ( 14.78437500061451715, 6.421520780324663323E-16, -5.243569643749999010 ) ) ;
#5206 = CARTESIAN_POINT ( 'NONE',  ( 19.80937500061451573, 4.541064518000418104, -2.621784821874998173 ) ) ;
#5207 = DIRECTION ( 'NONE',  ( 0.000000000000000000, 0.000000000000000000, 1.000000000000000000 ) ) ;
#5208 = CARTESIAN_POINT ( 'NONE',  ( 2.121784821874999061, 19.20312500061451644, 26.32496088578401583 ) ) ;
#5209 = CARTESIAN_POINT ( 'NONE',  ( 21.71250000122903501, -4.330127018922190985, -2.500000000000001332 ) ) ;
#5210 = CARTESIAN_POINT ( 'NONE',  ( 16.32187500061451502, 2.746126346562643317, 4.756430356249998326 ) ) ;
#5211 = CARTESIAN_POINT ( 'NONE',  ( 12.96562500061451928, 3.027376345333612662, -5.243569643749998122 ) ) ;
#5212 = CARTESIAN_POINT ( 'NONE',  ( 4.396875000614516971, -3.027376345333610441, -5.243569643749999898 ) ) ;
#5213 = CARTESIAN_POINT ( 'NONE',  ( 6.309375000614517504, 4.541064518000418104, -2.621784821874998173 ) ) ;
#5214 = ORIENTED_EDGE ( 'NONE', *, *, #71351, .F. ) ;
#5215 = CARTESIAN_POINT ( 'NONE',  ( 27.15937500061451360, 0.000000000000000000, 5.243569643749999010 ) ) ;
#5216 = CARTESIAN_POINT ( 'NONE',  ( 19.75312500061451360, 4.541064518000418104, -2.621784821874998173 ) ) ;
#5217 = CARTESIAN_POINT ( 'NONE',  ( 29.58750000122903501, 4.330127018922191873, 2.499999999999999556 ) ) ;
#5218 = CARTESIAN_POINT ( 'NONE',  ( 28.34062500061451928, 6.054752690667223547, 3.707466751127219781E-16 ) ) ;
#5219 = CARTESIAN_POINT ( 'NONE',  ( 23.59687500061451715, -3.027376345333614438, 5.243569643749998122 ) ) ;
#5220 = CARTESIAN_POINT ( 'NONE',  ( 19.71562500061451928, 3.027376345333613106, -5.243569643749998122 ) ) ;
#5221 = CARTESIAN_POINT ( 'NONE',  ( -1.999999999999997113, 10.17500000000000249, 33.46410161513775705 ) ) ;
#5222 = CARTESIAN_POINT ( 'NONE',  ( 25.37812500061451715, -4.541064518000419881, 2.621784821874995952 ) ) ;
#5223 = CARTESIAN_POINT ( 'NONE',  ( 5.850000001229035185, -2.886751345948129988, 4.999999999999997335 ) ) ;
#5224 = EDGE_LOOP ( 'NONE', ( #29968, #17834, #57777, #70360 ) ) ;
#5225 = CARTESIAN_POINT ( 'NONE',  ( 28.04999999999999716, 4.330127018922192761, -2.499999999999997780 ) ) ;
#5226 = CARTESIAN_POINT ( 'NONE',  ( -2.000000000000000000, 15.87500000000000000, -33.46410161513775705 ) ) ;
#5227 = CARTESIAN_POINT ( 'NONE',  ( -7.967954043666661671E-16, 17.59062499938548285, 34.33755215474603517 ) ) ;
#5228 = EDGE_CURVE ( 'NONE', #63939, #71801, #31182, .T. ) ;
#5229 = CARTESIAN_POINT ( 'NONE',  ( 5.296875000614518214, -3.027376345333610441, -5.243569643749999898 ) ) ;
#5230 = CARTESIAN_POINT ( 'NONE',  ( 13.45312500061451466, 4.541064518000418104, -2.621784821874998173 ) ) ;
#5231 = CARTESIAN_POINT ( 'NONE',  ( 6.196875000614515905, -3.027376345333610441, -5.243569643749999898 ) ) ;
#5232 = CARTESIAN_POINT ( 'NONE',  ( 23.58750000122903145, 6.123233995736764310E-16, -4.999999999999998224 ) ) ;
#5233 = CARTESIAN_POINT ( 'NONE',  ( 14.10937500061451644, 0.000000000000000000, 5.243569643749999010 ) ) ;
#5234 = CARTESIAN_POINT ( 'NONE',  ( 2.896875000614518747, -3.027376345333614438, 5.243569643749998122 ) ) ;
#5235 = CARTESIAN_POINT ( 'NONE',  ( 27.15000000000000213, 4.330127018922192761, -2.499999999999997780 ) ) ;
#5236 =( BOUNDED_CURVE ( )  B_SPLINE_CURVE ( 2, ( #29825, #70446, #19448, #52360, #1764, #35725, #41285 ),
 .UNSPECIFIED., .F., .F. ) 
 B_SPLINE_CURVE_WITH_KNOTS ( ( 3, 2, 2, 3 ),
 ( 0.01666666666666663174, 0.01944444444444440312, 0.02222222222222217797, 0.02499999999999994935 ),
 .UNSPECIFIED. ) 
 CURVE ( )  GEOMETRIC_REPRESENTATION_ITEM ( )  RATIONAL_B_SPLINE_CURVE ( ( 1.000000000000001554, 0.8660254037844370423, 1.000000000000000000, 0.8660254037844387076, 1.000000000000000000, 0.8660254037844412611, 0.9999999999999974465 ) ) 
 REPRESENTATION_ITEM ( '' )  );
#5237 = CARTESIAN_POINT ( 'NONE',  ( 25.54687500061451644, -3.027376345333610441, -5.243569643749999898 ) ) ;
#5238 = CARTESIAN_POINT ( 'NONE',  ( 2.878125000614517592, -4.541064518000419881, 2.621784821874995952 ) ) ;
#5239 = CARTESIAN_POINT ( 'NONE',  ( 13.41562500061451502, 3.027376345333613106, -5.243569643749998122 ) ) ;
#5240 = ORIENTED_EDGE ( 'NONE', *, *, #14959, .F. ) ;
#5241 = CARTESIAN_POINT ( 'NONE',  ( 9.815625000614518925, 3.027376345333613106, -5.243569643749998122 ) ) ;
#5242 = VECTOR ( 'NONE', #12140, 1000.000000000000000 ) ;
#5243 = CARTESIAN_POINT ( 'NONE',  ( 7.190625000614518036, 6.054752690667223547, 3.707466751127219781E-16 ) ) ;
#5244 = CARTESIAN_POINT ( 'NONE',  ( 18.75937500061451857, -4.119189519843965641, -2.378215178125001383 ) ) ;
#5245 = CARTESIAN_POINT ( 'NONE',  ( 14.60625000122903216, 4.330127018922192761, -2.499999999999997780 ) ) ;
#5246 = CARTESIAN_POINT ( 'NONE',  ( 15.18750000000000000, -2.886751345948129988, 4.999999999999997335 ) ) ;
#5247 = CARTESIAN_POINT ( 'NONE',  ( 16.17187500061451644, 3.027376345333613106, -5.243569643749998122 ) ) ;
#5248 = CARTESIAN_POINT ( 'NONE',  ( 13.80000000122903181, 5.773502691896255534, 3.535250795749688894E-16 ) ) ;
#5249 = CARTESIAN_POINT ( 'NONE',  ( 19.53749999999999432, 5.773502691896255534, 3.535250795749688894E-16 ) ) ;
#5250 = CARTESIAN_POINT ( 'NONE',  ( 20.44687500061451857, -3.027376345333614438, 5.243569643749998122 ) ) ;
#5251 = CARTESIAN_POINT ( 'NONE',  ( -4.243569643749997233, 13.09062500061451750, -27.54997392385601174 ) ) ;
#5252 = CARTESIAN_POINT ( 'NONE',  ( 20.60625000122902861, 0.000000000000000000, 4.999999999999998224 ) ) ;
#5253 = CARTESIAN_POINT ( 'NONE',  ( 25.54687500061451644, 4.119189519843966529, -2.378215178124998275 ) ) ;
#5254 = CARTESIAN_POINT ( 'NONE',  ( 24.05625000122903145, 4.330127018922192761, -2.499999999999997780 ) ) ;
#5255 = CARTESIAN_POINT ( 'NONE',  ( 26.35312500061451857, -4.541064518000417216, -2.621784821875001281 ) ) ;
#5256 = CARTESIAN_POINT ( 'NONE',  ( 0.000000000000000000, 20.00000000000000000, -30.00000000000000000 ) ) ;
#5257 = CARTESIAN_POINT ( 'NONE',  ( 26.13749999999999929, -2.886751345948125991, -5.000000000000000000 ) ) ;
#5258 = CARTESIAN_POINT ( 'NONE',  ( 9.928125000614517859, 4.541064518000418104, 2.621784821874999949 ) ) ;
#5259 = CARTESIAN_POINT ( 'NONE',  ( 27.87187500061451217, 4.119189519843966529, 2.378215178124999607 ) ) ;
#5260 = CARTESIAN_POINT ( 'NONE',  ( 20.70937500061451786, 4.541064518000418104, -2.621784821874998173 ) ) ;
#5261 = CARTESIAN_POINT ( 'NONE',  ( 13.09687500061451715, 0.000000000000000000, 4.756430356249998326 ) ) ;
#5262 = CARTESIAN_POINT ( 'NONE',  ( 5.015625000614518214, 3.027376345333611329, 5.243569643749999010 ) ) ;
#5263 = CARTESIAN_POINT ( 'NONE',  ( 10.88437500061451679, 4.541064518000418104, 2.621784821874999949 ) ) ;
#5264 = EDGE_LOOP ( 'NONE', ( #109, #35021, #31232, #31401 ) ) ;
#5265 = CARTESIAN_POINT ( 'NONE',  ( 20.67187500061451289, 3.027376345333613106, -5.243569643749998122 ) ) ;
#5266 = DIRECTION ( 'NONE',  ( -1.000000000000000000, -0.000000000000000000, -0.000000000000000000 ) ) ;
#5267 = FACE_OUTER_BOUND ( 'NONE', #61046, .T. ) ;
#5268 =( BOUNDED_CURVE ( )  B_SPLINE_CURVE ( 2, ( #30, #381, #62067, #45808, #6278, #22888, #28807 ),
 .UNSPECIFIED., .F., .F. ) 
 B_SPLINE_CURVE_WITH_KNOTS ( ( 3, 2, 2, 3 ),
 ( 0.5916666666666667851, 0.5944444444444445530, 0.5972222222222222099, 0.5999999999999999778 ),
 .UNSPECIFIED. ) 
 CURVE ( )  GEOMETRIC_REPRESENTATION_ITEM ( )  RATIONAL_B_SPLINE_CURVE ( ( 0.9999999999999946709, 0.8660254037844440367, 1.000000000000000000, 0.8660254037844387076, 1.000000000000000000, 0.8660254037844387076, 1.000000000000000000 ) ) 
 REPRESENTATION_ITEM ( '' )  );
#5269 = CARTESIAN_POINT ( 'NONE',  ( 4.200000000000001954, 4.330127018922192761, -2.499999999999997780 ) ) ;
#5270 = CARTESIAN_POINT ( 'NONE',  ( 13.76250000122903394, 4.330127018922192761, -2.499999999999997780 ) ) ;
#5271 = CARTESIAN_POINT ( 'NONE',  ( 45.00000000000000000, 6.123233995736764310E-16, -4.999999999999998224 ) ) ;
#5272 = CARTESIAN_POINT ( 'NONE',  ( 3.760358691118133034, -3.295428057128597210, 4.078640785394780366 ) ) ;
#5273 = ORIENTED_EDGE ( 'NONE', *, *, #29804, .T. ) ;
#5274 = CARTESIAN_POINT ( 'NONE',  ( 13.16249999999999964, 2.886751345948129099, -4.999999999999998224 ) ) ;
#5275 = CARTESIAN_POINT ( 'NONE',  ( 15.82499999999999929, 6.123233995736764310E-16, -4.999999999999998224 ) ) ;
#5276 = CARTESIAN_POINT ( 'NONE',  ( 12.11250000122903181, 0.000000000000000000, 4.999999999999998224 ) ) ;
#5277 = CARTESIAN_POINT ( 'NONE',  ( 11.16562500061451679, 3.027376345333613106, -5.243569643749998122 ) ) ;
#5278 = EDGE_CURVE ( 'NONE', #59530, #39431, #54709, .T. ) ;
#5279 = CARTESIAN_POINT ( 'NONE',  ( 9.412499999999999645, -5.773502691896255534, -1.060575238724906372E-15 ) ) ;
#5280 = CARTESIAN_POINT ( 'NONE',  ( -1.071796769724491005, 15.52009619066136814, 26.00000000000000355 ) ) ;
#5281 = CARTESIAN_POINT ( 'NONE',  ( -4.243569643749999898, 14.42187500061451644, -32.45002607614398471 ) ) ;
#5282 = CARTESIAN_POINT ( 'NONE',  ( 29.10000000122903074, 5.773502691896255534, 3.535250795749688894E-16 ) ) ;
#5283 = CARTESIAN_POINT ( 'NONE',  ( 3.756430356250000102, 13.99062499938548498, 30.00000000000000000 ) ) ;
#5284 = CARTESIAN_POINT ( 'NONE',  ( 7.462500000000001243, 2.886751345948126879, 4.999999999999999112 ) ) ;
#5285 = CARTESIAN_POINT ( 'NONE',  ( 16.21875000122903643, -5.773502691896255534, -1.060575238724906372E-15 ) ) ;
#5286 = VECTOR ( 'NONE', #42221, 1000.000000000000000 ) ;
#5287 = VERTEX_POINT ( 'NONE', #57239 ) ;
#5288 = CARTESIAN_POINT ( 'NONE',  ( 25.49062500061451786, -3.027376345333610441, -5.243569643749999898 ) ) ;
#5289 = CARTESIAN_POINT ( 'NONE',  ( 2.000000000000001332, 13.40000000000000213, -26.53589838486224650 ) ) ;
#5290 = CARTESIAN_POINT ( 'NONE',  ( 18.97500000122903430, -5.773502691896255534, -1.060575238724906372E-15 ) ) ;
#5291 = CARTESIAN_POINT ( 'NONE',  ( 21.90937500061451715, -4.541064518000417216, -2.621784821875001281 ) ) ;
#5292 = EDGE_CURVE ( 'NONE', #59817, #30697, #28451, .T. ) ;
#5293 = CARTESIAN_POINT ( 'NONE',  ( 15.81562500061451537, 3.027376345333611329, 5.243569643749999010 ) ) ;
#5294 = CARTESIAN_POINT ( 'NONE',  ( -2.121784821874996840, 11.32812500061459282, -26.32496088578401583 ) ) ;
#5295 = CARTESIAN_POINT ( 'NONE',  ( 6.665625000614515905, 3.027376345333613106, -5.243569643749998122 ) ) ;
#5296 = CARTESIAN_POINT ( 'NONE',  ( 28.50000000122903288, -2.886751345948125991, -5.000000000000000000 ) ) ;
#5297 = CARTESIAN_POINT ( 'NONE',  ( 24.79687500061452354, 5.492252693125287522, 3.363034840372157021E-16 ) ) ;
#5298 = CARTESIAN_POINT ( 'NONE',  ( 20.16562500061451502, 3.027376345333612662, -5.243569643749998122 ) ) ;
#5299 = DIRECTION ( 'NONE',  ( 1.000000000000000000, 0.000000000000000000, 0.000000000000000000 ) ) ;
#5300 = CARTESIAN_POINT ( 'NONE',  ( -1.878215178124999163, 18.19062499938548427, 26.74683588394047007 ) ) ;
#5302 = EDGE_CURVE ( 'NONE', #61284, #68160, #23261, .T. ) ;
#5301 = CARTESIAN_POINT ( 'NONE',  ( 14.93437500061451750, 4.541064518000418104, 2.621784821874999949 ) ) ;
#5303 = CARTESIAN_POINT ( 'NONE',  ( 13.88437500061451679, 6.421520780324663323E-16, -5.243569643749999010 ) ) ;
#5304 = CARTESIAN_POINT ( 'NONE',  ( 22.17187500061451644, 3.027376345333611329, 5.243569643749999010 ) ) ;
#5305 = ORIENTED_EDGE ( 'NONE', *, *, #10249, .T. ) ;
#5306 = CARTESIAN_POINT ( 'NONE',  ( -3.999999999999999112, 14.71250000122903501, -30.00000000000000000 ) ) ;
#5307 = CARTESIAN_POINT ( 'NONE',  ( 27.32812500061451644, 6.421520780324663323E-16, -5.243569643749999010 ) ) ;
#5308 =( BOUNDED_CURVE ( )  B_SPLINE_CURVE ( 2, ( #5748, #61523, #67092, #38642, #61166, #33089, #39008, #15723, #55628 ),
 .UNSPECIFIED., .F., .F. ) 
 B_SPLINE_CURVE_WITH_KNOTS ( ( 3, 2, 2, 2, 3 ),
 ( 0.5416666666666667407, 0.5462962962962962798, 0.5555555555555555802, 0.5648148148148147696, 0.5694444444444444198 ),
 .UNSPECIFIED. ) 
 CURVE ( )  GEOMETRIC_REPRESENTATION_ITEM ( )  RATIONAL_B_SPLINE_CURVE ( ( 0.9330127018922192983, 0.9330127018922200755, 1.000000000000000000, 0.8660254037844387076, 1.000000000000000000, 0.8660254037844387076, 1.000000000000000000, 0.9330127018922194093, 0.9330127018922194093 ) ) 
 REPRESENTATION_ITEM ( '' )  );
#5309 = AXIS2_PLACEMENT_3D ( 'NONE', #15363, #60423, #9834 ) ;
#5310 = CARTESIAN_POINT ( 'NONE',  ( 25.90312500061451573, -4.541064518000417216, -2.621784821875001281 ) ) ;
#5311 = CARTESIAN_POINT ( 'NONE',  ( 1.071796769724491893, 12.03259618943233455, -26.00000000000000355 ) ) ;
#5312 = CARTESIAN_POINT ( 'NONE',  ( -3.999999999999997335, 17.78750000000000142, 32.30940107675850470 ) ) ;
#5313 = CARTESIAN_POINT ( 'NONE',  ( 5.784375000614517148, 6.421520780324663323E-16, -5.243569643749999010 ) ) ;
#5314 = CARTESIAN_POINT ( 'NONE',  ( 11.06250000122903288, 4.330127018922192761, -2.499999999999997780 ) ) ;
#5315 = VECTOR ( 'NONE', #27794, 1000.000000000000000 ) ;
#5316 = CARTESIAN_POINT ( 'NONE',  ( 7.087500001229034119, 4.330127018922191873, 2.499999999999999556 ) ) ;
#5317 = CARTESIAN_POINT ( 'NONE',  ( 3.403125000614518836, -4.541064518000417216, -2.621784821875001281 ) ) ;
#5318 = CARTESIAN_POINT ( 'NONE',  ( 4.000000000000000000, 19.68124999877096570, 27.69059892324149530 ) ) ;
#5319 = CARTESIAN_POINT ( 'NONE',  ( 17.64375000122903003, -2.886751345948125991, -5.000000000000000000 ) ) ;
#5320 = CARTESIAN_POINT ( 'NONE',  ( 12.83437500061451786, -4.541064518000419881, 2.621784821874995952 ) ) ;
#5321 = CARTESIAN_POINT ( 'NONE',  ( -5.810221930991193690E-16, 12.23750000000000071, 26.00000000000000355 ) ) ;
#5322 = EDGE_LOOP ( 'NONE', ( #46801, #7370, #39720, #23204 ) ) ;
#5323 = CARTESIAN_POINT ( 'NONE',  ( 19.19062500061452070, -3.027376345333610441, -5.243569643749999898 ) ) ;
#5324 = CARTESIAN_POINT ( 'NONE',  ( 12.94687500061451857, -3.027376345333610441, -5.243569643749999898 ) ) ;
#5325 = CARTESIAN_POINT ( 'NONE',  ( 5.803125000614517859, 4.541064518000418104, -2.621784821874998173 ) ) ;
#5326 = CARTESIAN_POINT ( 'NONE',  ( 21.12187500061451573, 3.027376345333612662, -5.243569643749998122 ) ) ;
#5327 = CARTESIAN_POINT ( 'NONE',  ( 9.459375000614517859, 4.541064518000418104, -2.621784821874998173 ) ) ;
#5328 = CARTESIAN_POINT ( 'NONE',  ( 4.640625000614518214, -3.027376345333614438, 5.243569643749998122 ) ) ;
#5329 = CARTESIAN_POINT ( 'NONE',  ( 0.000000000000000000, 20.00000000000000000, 30.00000000000000000 ) ) ;
#5330 = CARTESIAN_POINT ( 'NONE',  ( 5.212500001229032343, 4.330127018922192761, -2.499999999999997780 ) ) ;
#5331 = CARTESIAN_POINT ( 'NONE',  ( 19.04062500061451146, -3.027376345333614438, 5.243569643749998122 ) ) ;
#5332 = CARTESIAN_POINT ( 'NONE',  ( 7.237500001229035362, -4.330127018922194537, 2.499999999999995559 ) ) ;
#5333 =( BOUNDED_CURVE ( )  B_SPLINE_CURVE ( 2, ( #21141, #49600, #38136, #16329, #32604, #61037, #67330, #72127, #72859 ),
 .UNSPECIFIED., .F., .F. ) 
 B_SPLINE_CURVE_WITH_KNOTS ( ( 3, 2, 2, 2, 3 ),
 ( 0.3586956521739130821, 0.3623188405797101441, 0.3695652173913043237, 0.3768115942028985588, 0.3804347826086956763 ),
 .UNSPECIFIED. ) 
 CURVE ( )  GEOMETRIC_REPRESENTATION_ITEM ( )  RATIONAL_B_SPLINE_CURVE ( ( 0.9330127018922194093, 0.9330127018922198534, 1.000000000000000000, 0.8660254037844387076, 1.000000000000000000, 0.8660254037844387076, 1.000000000000000000, 0.9330127018922188542, 0.9330127018922194093 ) ) 
 REPRESENTATION_ITEM ( '' )  );
#5334 = CARTESIAN_POINT ( 'NONE',  ( 18.36562500061451431, 3.027376345333613106, -5.243569643749998122 ) ) ;
#5335 = CARTESIAN_POINT ( 'NONE',  ( 15.32812500061451644, 4.541064518000418104, 2.621784821874999949 ) ) ;
#5336 = CARTESIAN_POINT ( 'NONE',  ( 24.98437500061451644, -4.119189519843968306, 2.378215178124996054 ) ) ;
#5337 = CARTESIAN_POINT ( 'NONE',  ( 15.93750000000000000, 5.773502691896255534, 3.535250795749688894E-16 ) ) ;
#5338 = CARTESIAN_POINT ( 'NONE',  ( 9.487500001229033586, -4.330127018922194537, 2.499999999999995559 ) ) ;
#5339 = ADVANCED_FACE ( 'NONE', ( #33987 ), #12182, .F. ) ;
#5340 = CARTESIAN_POINT ( 'NONE',  ( 4.640625000614518214, -3.027376345333614438, 5.243569643749998122 ) ) ;
#5341 = CARTESIAN_POINT ( 'NONE',  ( 21.97500000122903074, 2.886751345948126879, 4.999999999999999112 ) ) ;
#5342 = CARTESIAN_POINT ( 'NONE',  ( 26.36249999999999716, 2.886751345948126879, 4.999999999999999112 ) ) ;
#5343 = CARTESIAN_POINT ( 'NONE',  ( -2.121784821874996840, 13.63437500061451857, -26.32496088578401583 ) ) ;
#5344 = CARTESIAN_POINT ( 'NONE',  ( 21.22500000000000142, 6.123233995736764310E-16, -4.999999999999998224 ) ) ;
#5345 = CARTESIAN_POINT ( 'NONE',  ( 3.525000001229034119, 2.886751345948126879, 4.999999999999999112 ) ) ;
#5346 = CARTESIAN_POINT ( 'NONE',  ( 5.109375000614518214, 0.000000000000000000, 5.243569643749999010 ) ) ;
#5347 = CARTESIAN_POINT ( 'NONE',  ( 20.44687500061451857, -3.027376345333614438, 5.243569643749998122 ) ) ;
#5348 = CARTESIAN_POINT ( 'NONE',  ( -1.071796769724491005, 14.95759618943233527, 26.00000000000000355 ) ) ;
#5349 = CARTESIAN_POINT ( 'NONE',  ( 17.39062500061451644, -3.027376345333610441, -5.243569643749999898 ) ) ;
#5350 = CARTESIAN_POINT ( 'NONE',  ( 10.89375000122903003, -2.886751345948125991, -5.000000000000000000 ) ) ;
#5351 = CARTESIAN_POINT ( 'NONE',  ( -2.000000000000000000, 15.42500000000000071, -33.46410161513775705 ) ) ;
#5352 = CARTESIAN_POINT ( 'NONE',  ( 1.592000809091587073E-14, 15.38750000000000284, 26.00000000000000000 ) ) ;
#5353 = CARTESIAN_POINT ( 'NONE',  ( 28.24687500061451573, -3.027376345333610441, -5.243569643749999898 ) ) ;
#5354 = CARTESIAN_POINT ( 'NONE',  ( 21.79687500061451644, -4.119189519843965641, -2.378215178125001383 ) ) ;
#5355 = CARTESIAN_POINT ( 'NONE',  ( 13.49062500061451608, 6.054752690667223547, 3.707466751127219781E-16 ) ) ;
#5356 = CARTESIAN_POINT ( 'NONE',  ( 11.78437500061451892, 4.541064518000418104, 2.621784821874999949 ) ) ;
#5357 = VERTEX_POINT ( 'NONE', #33 ) ;
#5358 = CARTESIAN_POINT ( 'NONE',  ( 28.79062500061451502, 6.054752690667223547, 3.707466751127219781E-16 ) ) ;
#5359 = CARTESIAN_POINT ( 'NONE',  ( 22.90312500061451573, 4.541064518000418104, -2.621784821874998173 ) ) ;
#5360 = DIRECTION ( 'NONE',  ( 0.000000000000000000, 0.000000000000000000, 1.000000000000000000 ) ) ;
#5361 = CARTESIAN_POINT ( 'NONE',  ( -1.999999999999997113, 12.98750000122903359, 33.46410161513775705 ) ) ;
#5362 = CARTESIAN_POINT ( 'NONE',  ( 11.51250000000000107, 2.886751345948126879, 4.999999999999999112 ) ) ;
#5363 = CARTESIAN_POINT ( 'NONE',  ( 21.63750000122903572, -4.330127018922194537, 2.499999999999995559 ) ) ;
#5364 = CARTESIAN_POINT ( 'NONE',  ( 16.86562500061451786, -6.054752690667223547, -1.112240025338166033E-15 ) ) ;
#5365 = CARTESIAN_POINT ( 'NONE',  ( 12.45937500061451608, 2.746126346562645981, -4.756430356249997438 ) ) ;
#5366 = ORIENTED_EDGE ( 'NONE', *, *, #21219, .T. ) ;
#5367 = CARTESIAN_POINT ( 'NONE',  ( 19.72499999999999787, -4.330127018922194537, 2.499999999999995559 ) ) ;
#5368 = CARTESIAN_POINT ( 'NONE',  ( 24.56250000000000000, 2.886751345948126879, 4.999999999999999112 ) ) ;
#5369 = CARTESIAN_POINT ( 'NONE',  ( 22.02187500061452141, 3.027376345333613106, -5.243569643749998122 ) ) ;
#5370 = CARTESIAN_POINT ( 'NONE',  ( 28.75312500061451715, 4.541064518000418104, -2.621784821874998173 ) ) ;
#5371 = ORIENTED_EDGE ( 'NONE', *, *, #28737, .F. ) ;
#5372 = CARTESIAN_POINT ( 'NONE',  ( 0.000000000000000000, 4.999999999999998224, 0.000000000000000000 ) ) ;
#5373 = CARTESIAN_POINT ( 'NONE',  ( 8.015625000614518214, 3.027376345333613106, -5.243569643749998122 ) ) ;
#5374 = CARTESIAN_POINT ( 'NONE',  ( 34.99999999999999289, 4.500000000000000888, -3.500000000000000000 ) ) ;
#5375 = CARTESIAN_POINT ( 'NONE',  ( 18.11250000000000071, 2.886751345948129099, -4.999999999999998224 ) ) ;
#5376 = CARTESIAN_POINT ( 'NONE',  ( 24.60000000000000142, 0.000000000000000000, 4.999999999999998224 ) ) ;
#5377 = CARTESIAN_POINT ( 'NONE',  ( 5.146875000614517859, -3.027376345333614438, 5.243569643749998122 ) ) ;
#5378 = CARTESIAN_POINT ( 'NONE',  ( 29.10937500061451644, -4.541064518000417216, -2.621784821875001281 ) ) ;
#5379 = ORIENTED_EDGE ( 'NONE', *, *, #70256, .F. ) ;
#5380 = CARTESIAN_POINT ( 'NONE',  ( 24.51562500061451289, -6.054752690667223547, -1.112240025338166033E-15 ) ) ;
#5381 = CARTESIAN_POINT ( 'NONE',  ( 26.07187500061451857, 3.027376345333613106, -5.243569643749998122 ) ) ;
#5382 = CARTESIAN_POINT ( 'NONE',  ( 2.121784821874999061, 18.75312500061459886, -33.67503911421598417 ) ) ;
#5383 = CARTESIAN_POINT ( 'NONE',  ( 11.73750000000000249, -2.886751345948125991, -5.000000000000000000 ) ) ;
#5384 = CARTESIAN_POINT ( 'NONE',  ( 8.803125000614517859, -4.541064518000417216, -2.621784821875001281 ) ) ;
#5385 = CARTESIAN_POINT ( 'NONE',  ( -4.243569643749999898, 19.85937500061451644, 30.00000000000000000 ) ) ;
#5386 = CARTESIAN_POINT ( 'NONE',  ( 17.06250000000000000, -5.773502691896255534, -1.060575238724906372E-15 ) ) ;
#5387 = CARTESIAN_POINT ( 'NONE',  ( 25.19062500061451715, 6.054752690667223547, 3.707466751127219781E-16 ) ) ;
#5388 = CARTESIAN_POINT ( 'NONE',  ( -3.999999999999999112, 18.16250000000000142, 27.69059892324149885 ) ) ;
#5389 = CARTESIAN_POINT ( 'NONE',  ( 15.34687500061451537, 5.492252693125287522, 3.363034840372157021E-16 ) ) ;
#5390 = CARTESIAN_POINT ( 'NONE',  ( 3.403125000614518836, -4.541064518000417216, -2.621784821875001281 ) ) ;
#5391 = CARTESIAN_POINT ( 'NONE',  ( 19.50937500061451857, 0.000000000000000000, 5.243569643749999010 ) ) ;
#5392 = CARTESIAN_POINT ( 'NONE',  ( -2.121784821874996840, 14.98437500061451644, 33.67503911421598417 ) ) ;
#5393 = EDGE_CURVE ( 'NONE', #50344, #27832, #69810, .T. ) ;
#5394 = CARTESIAN_POINT ( 'NONE',  ( 22.50937500061451857, 4.541064518000418104, -2.621784821874998173 ) ) ;
#5395 = CARTESIAN_POINT ( 'NONE',  ( 3.675000000000001155, 6.123233995736764310E-16, -4.999999999999998224 ) ) ;
#5396 = CARTESIAN_POINT ( 'NONE',  ( 10.57500000000000107, 4.330127018922191873, 2.499999999999999556 ) ) ;
#5397 = CARTESIAN_POINT ( 'NONE',  ( 11.09062500061451573, -3.027376345333610441, -5.243569643749999898 ) ) ;
#5398 = CARTESIAN_POINT ( 'NONE',  ( -1.071796769724483234, 15.07009619066136885, 25.99999999999999645 ) ) ;
#5399 = CARTESIAN_POINT ( 'NONE',  ( 6.121875000614517504, -6.054752690667223547, -1.112240025338166033E-15 ) ) ;
#5400 = CARTESIAN_POINT ( 'NONE',  ( 7.500000001229033764, 5.773502691896255534, 3.535250795749688401E-16 ) ) ;
#5401 = AXIS2_PLACEMENT_3D ( 'NONE', #29095, #73072, #56443 ) ;
#5402 = CARTESIAN_POINT ( 'NONE',  ( 8.278125000614515727, -4.541064518000419881, 2.621784821874995952 ) ) ;
#5403 = CARTESIAN_POINT ( 'NONE',  ( 13.05937500061451750, 4.541064518000418104, -2.621784821874998173 ) ) ;
#5404 = CARTESIAN_POINT ( 'NONE',  ( 18.71250000122903145, 4.330127018922192761, -2.499999999999997780 ) ) ;
#5405 = CARTESIAN_POINT ( 'NONE',  ( 9.121875000614517504, 3.027376345333611329, 5.243569643749999010 ) ) ;
#5406 = CARTESIAN_POINT ( 'NONE',  ( 9.403125000614517504, 4.541064518000418104, -2.621784821874998173 ) ) ;
#5407 = DIRECTION ( 'NONE',  ( 1.000000000000000000, 0.000000000000000000, 0.000000000000000000 ) ) ;
#5408 = CARTESIAN_POINT ( 'NONE',  ( 27.01875000122903359, -5.773502691896255534, -1.060575238724906372E-15 ) ) ;
#5409 = CARTESIAN_POINT ( 'NONE',  ( 18.23437500061451999, -4.541064518000419881, 2.621784821874995952 ) ) ;
#5410 = CARTESIAN_POINT ( 'NONE',  ( 26.35312500061451857, -4.541064518000417216, -2.621784821875001281 ) ) ;
#5411 = CARTESIAN_POINT ( 'NONE',  ( 11.16562500061451679, 3.027376345333613106, -5.243569643749998122 ) ) ;
#5412 = DIRECTION ( 'NONE',  ( 0.000000000000000000, 0.000000000000000000, 1.000000000000000000 ) ) ;
#5413 = CARTESIAN_POINT ( 'NONE',  ( -2.121784821874996840, 13.18437500061451750, -26.32496088578401583 ) ) ;
#5414 = CARTESIAN_POINT ( 'NONE',  ( 12.41250000122903430, 4.330127018922192761, -2.499999999999997780 ) ) ;
#5415 = CARTESIAN_POINT ( 'NONE',  ( 28.00312500061451715, 0.000000000000000000, 5.243569643749999010 ) ) ;
#5416 = CIRCLE ( 'NONE', #33712, 1.500000000000000444 ) ;
#5417 = CARTESIAN_POINT ( 'NONE',  ( 2.121784821874999061, 16.50312500061451715, -33.67503911421598417 ) ) ;
#5418 = CARTESIAN_POINT ( 'NONE',  ( 15.75000000122902932, -2.886751345948129988, 4.999999999999997335 ) ) ;
#5419 = AXIS2_PLACEMENT_3D ( 'NONE', #61337, #56521, #68344 ) ;
#5420 = CARTESIAN_POINT ( 'NONE',  ( 12.67499999999999893, 6.123233995736764310E-16, -4.999999999999998224 ) ) ;
#5421 = CARTESIAN_POINT ( 'NONE',  ( 23.94375000122903074, -2.886751345948112224, -5.000000000000023981 ) ) ;
#5422 = CARTESIAN_POINT ( 'NONE',  ( 22.82812500061451644, 6.421520780324663323E-16, -5.243569643749999010 ) ) ;
#5423 = CARTESIAN_POINT ( 'NONE',  ( 6.721875000614518925, 3.027376345333612662, -5.243569643749998122 ) ) ;
#5424 = CARTESIAN_POINT ( 'NONE',  ( 8.812500001229034652, 4.330127018922192761, -2.499999999999997780 ) ) ;
#5425 = CARTESIAN_POINT ( 'NONE',  ( 15.03750000122903252, 6.123233995736764310E-16, -4.999999999999998224 ) ) ;
#5426 = CARTESIAN_POINT ( 'NONE',  ( 14.20312500061451644, -4.541064518000417216, -2.621784821875001281 ) ) ;
#5427 = CARTESIAN_POINT ( 'NONE',  ( 18.77812500061451573, 6.421520780324663323E-16, -5.243569643749999010 ) ) ;
#5428 = CARTESIAN_POINT ( 'NONE',  ( 26.17500000122903359, -5.773502691896255534, -1.060575238724906372E-15 ) ) ;
#5429 = CARTESIAN_POINT ( 'NONE',  ( 27.41250000122903430, 0.000000000000000000, 4.999999999999998224 ) ) ;
#5430 = CARTESIAN_POINT ( 'NONE',  ( 23.02499999999999858, 6.123233995736764310E-16, -4.999999999999998224 ) ) ;
#5431 = CARTESIAN_POINT ( 'NONE',  ( 25.58437500061451431, 6.421520780324663323E-16, -5.243569643749999010 ) ) ;
#5432 = CARTESIAN_POINT ( 'NONE',  ( 45.00000000000000000, 8.874999999999998224, -1.494782592887687667 ) ) ;
#5433 = EDGE_CURVE ( 'NONE', #7083, #19771, #8098, .T. ) ;
#5434 = CARTESIAN_POINT ( 'NONE',  ( 9.862500001229033586, 0.000000000000000000, 4.999999999999998224 ) ) ;
#5435 = CARTESIAN_POINT ( 'NONE',  ( 26.97187500061451360, 3.027376345333613106, -5.243569643749998122 ) ) ;
#5436 = CYLINDRICAL_SURFACE ( 'NONE', #58515, 4.999999999999998224 ) ;
#5437 = CARTESIAN_POINT ( 'NONE',  ( 4.846875000614519813, -3.027376345333610441, -5.243569643749999898 ) ) ;
#5438 = CARTESIAN_POINT ( 'NONE',  ( 24.21562500061451573, 3.027376345333613106, -5.243569643749998122 ) ) ;
#5439 = CARTESIAN_POINT ( 'NONE',  ( -1.878215178125001827, 15.30312499938548321, 33.25316411605952283 ) ) ;
#5440 = CARTESIAN_POINT ( 'NONE',  ( -1.999999999999999112, 15.29374999877096641, 26.53589838486224650 ) ) ;
#5441 = CARTESIAN_POINT ( 'NONE',  ( 9.946875000614516793, 6.054752690667223547, 3.707466751127219781E-16 ) ) ;
#5442 = CARTESIAN_POINT ( 'NONE',  ( 24.37500000000000000, 6.123233995736764310E-16, -4.999999999999998224 ) ) ;
#5443 = CARTESIAN_POINT ( 'NONE',  ( 29.50312500061451360, -4.541064518000417216, -2.621784821875001281 ) ) ;
#5444 = CARTESIAN_POINT ( 'NONE',  ( 6.609375000614519102, -4.541064518000417216, -2.621784821875001281 ) ) ;
#5445 = CARTESIAN_POINT ( 'NONE',  ( 27.64687500061452141, -3.027376345333614438, 5.243569643749998122 ) ) ;
#5446 = DIRECTION ( 'NONE',  ( 0.000000000000000000, 0.000000000000000000, -1.000000000000000000 ) ) ;
#5447 = CARTESIAN_POINT ( 'NONE',  ( 19.50000000000000000, 4.330127018922192761, -2.499999999999997780 ) ) ;
#5448 = ORIENTED_EDGE ( 'NONE', *, *, #59933, .F. ) ;
#5449 = CARTESIAN_POINT ( 'NONE',  ( 28.38749999999999929, -2.886751345948125991, -5.000000000000000000 ) ) ;
#5450 =( BOUNDED_CURVE ( )  B_SPLINE_CURVE ( 2, ( #58196, #41588, #30138, #36039, #57483, #46410, #58559 ),
 .UNSPECIFIED., .F., .F. ) 
 B_SPLINE_CURVE_WITH_KNOTS ( ( 3, 2, 2, 3 ),
 ( 0.4500000000000000111, 0.4533333333333333104, 0.4566666666666666652, 0.4600000000000000200 ),
 .UNSPECIFIED. ) 
 CURVE ( )  GEOMETRIC_REPRESENTATION_ITEM ( )  RATIONAL_B_SPLINE_CURVE ( ( 1.000000000000000000, 0.8660254037844387076, 1.000000000000000000, 0.8660254037844387076, 1.000000000000000000, 0.8660254037844387076, 1.000000000000000000 ) ) 
 REPRESENTATION_ITEM ( '' )  );
#5451 = CARTESIAN_POINT ( 'NONE',  ( 27.57187500061451857, 3.027376345333611329, 5.243569643749999010 ) ) ;
#5452 = ORIENTED_EDGE ( 'NONE', *, *, #57133, .F. ) ;
#5453 = CARTESIAN_POINT ( 'NONE',  ( 17.27812500061451217, -4.541064518000419881, 2.621784821874995952 ) ) ;
#5454 = CARTESIAN_POINT ( 'NONE',  ( 8.690625000614515372, -3.027376345333614438, 5.243569643749998122 ) ) ;
#5455 = CARTESIAN_POINT ( 'NONE',  ( 21.34687500061451715, -4.119189519843965641, -2.378215178125001383 ) ) ;
#5456 = CARTESIAN_POINT ( 'NONE',  ( 3.721875000614518036, 3.027376345333611329, 5.243569643749999010 ) ) ;
#5457 = CARTESIAN_POINT ( 'NONE',  ( 18.22500000122903430, 2.886751345948129099, -4.999999999999998224 ) ) ;
#5458 = CARTESIAN_POINT ( 'NONE',  ( 24.63749999999999574, -2.886751345948129988, 4.999999999999997335 ) ) ;
#5459 = CARTESIAN_POINT ( 'NONE',  ( 2.000000000000000444, 19.77500000000000213, 26.53589838486224650 ) ) ;
#5460 = CARTESIAN_POINT ( 'NONE',  ( 6.684375000614518392, 6.421520780324663323E-16, -5.243569643749999010 ) ) ;
#5461 = CARTESIAN_POINT ( 'NONE',  ( 11.52187500061451608, -6.054752690667223547, -1.112240025338166033E-15 ) ) ;
#5462 = CARTESIAN_POINT ( 'NONE',  ( 22.24687500061451217, -3.027376345333614438, 5.243569643749998122 ) ) ;
#5463 = CARTESIAN_POINT ( 'NONE',  ( 4.898587196589411843E-16, 20.00000000000000000, 33.99999999999999289 ) ) ;
#5464 = VERTEX_POINT ( 'NONE', #18070 ) ;
#5465 = CARTESIAN_POINT ( 'NONE',  ( 4.584375000614516971, 4.541064518000418104, 2.621784821874999949 ) ) ;
#5466 = CARTESIAN_POINT ( 'NONE',  ( 10.91250000000000320, 2.886751345948129099, -4.999999999999998224 ) ) ;
#5467 = CARTESIAN_POINT ( 'NONE',  ( 6.121875000614517504, -6.054752690667223547, -1.112240025338166033E-15 ) ) ;
#5468 = CARTESIAN_POINT ( 'NONE',  ( -3.756430356250001434, 15.60312499938548392, 32.16877607737301048 ) ) ;
#5469 = CARTESIAN_POINT ( 'NONE',  ( 21.56250000000000000, -5.773502691896255534, -1.060575238724906372E-15 ) ) ;
#5470 = CARTESIAN_POINT ( 'NONE',  ( 17.27812500061451217, -4.541064518000419881, 2.621784821874995952 ) ) ;
#5471 = CARTESIAN_POINT ( 'NONE',  ( 2.000000000000000444, 17.97500000000000142, 26.53589838486224650 ) ) ;
#5472 = CARTESIAN_POINT ( 'NONE',  ( 30.00000000000000000, 0.000000000000000000, 0.000000000000000000 ) ) ;
#5473 = EDGE_CURVE ( 'NONE', #8533, #13160, #5917, .T. ) ;
#5474 = CARTESIAN_POINT ( 'NONE',  ( 22.50937500061451857, 4.119189519843966529, -2.378215178124998275 ) ) ;
#5475 = CARTESIAN_POINT ( 'NONE',  ( 10.11562500061451608, -6.054752690667223547, -1.112240025338166033E-15 ) ) ;
#5476 = CARTESIAN_POINT ( 'NONE',  ( 26.70937500061451431, 0.000000000000000000, 5.243569643749999010 ) ) ;
#5477 = CARTESIAN_POINT ( 'NONE',  ( -2.000000000000000000, 19.58750000122903501, 26.53589838486224650 ) ) ;
#5478 = CARTESIAN_POINT ( 'NONE',  ( 29.14687500061451075, -3.027376345333610441, -5.243569643749999898 ) ) ;
#5479 = CARTESIAN_POINT ( 'NONE',  ( 9.187500000000001776, 5.773502691896255534, 3.535250795749688894E-16 ) ) ;
#5480 = CARTESIAN_POINT ( 'NONE',  ( -3.999999999999999112, 16.51250000122903216, 30.00000000000000000 ) ) ;
#5481 = CARTESIAN_POINT ( 'NONE',  ( 9.862500001229033586, 0.000000000000000000, 4.999999999999998224 ) ) ;
#5482 = CARTESIAN_POINT ( 'NONE',  ( 20.10937500061451289, -4.541064518000417216, -2.621784821875001281 ) ) ;
#5483 = CARTESIAN_POINT ( 'NONE',  ( 14.52187500061451608, 3.027376345333611329, 5.243569643749999010 ) ) ;
#5484 = CARTESIAN_POINT ( 'NONE',  ( 9.225000001229034297, 2.886751345948129099, -4.999999999999997335 ) ) ;
#5485 = EDGE_LOOP ( 'NONE', ( #32259, #24814, #18681, #14610, #45131, #14448, #50932 ) ) ;
#5486 = CARTESIAN_POINT ( 'NONE',  ( 14.39062500061451821, 6.054752690667223547, 3.707466751127219781E-16 ) ) ;
#5487 = CARTESIAN_POINT ( 'NONE',  ( 26.02500000122903145, 2.886751345948126879, 4.999999999999999112 ) ) ;
#5488 = CARTESIAN_POINT ( 'NONE',  ( 14.07187500061451679, 3.027376345333611329, 5.243569643749999010 ) ) ;
#5489 = CARTESIAN_POINT ( 'NONE',  ( 3.178125000614515638, 4.541064518000418104, 2.621784821874999949 ) ) ;
#5490 = CARTESIAN_POINT ( 'NONE',  ( 16.00312500061451715, -4.541064518000417216, -2.621784821875001281 ) ) ;
#5491 = LINE ( 'NONE', #28379, #48040 ) ;
#5492 = CARTESIAN_POINT ( 'NONE',  ( 26.78437500061451360, -4.541064518000419881, 2.621784821874995952 ) ) ;
#5493 = CARTESIAN_POINT ( 'NONE',  ( 4.243569643749999010, 10.16562500061451857, 27.54997392385601174 ) ) ;
#5494 = CARTESIAN_POINT ( 'NONE',  ( 14.70937500061451786, -4.541064518000417216, -2.621784821875001281 ) ) ;
#5495 = CARTESIAN_POINT ( 'NONE',  ( 14.40000000122903323, -2.886751345948129988, 4.999999999999997335 ) ) ;
#5496 = CARTESIAN_POINT ( 'NONE',  ( 8.259375000614518569, 0.000000000000000000, 4.756430356249998326 ) ) ;
#5497 = DIRECTION ( 'NONE',  ( -0.000000000000000000, -1.000000000000000000, -0.000000000000000000 ) ) ;
#5498 = CARTESIAN_POINT ( 'NONE',  ( 21.34687500061451715, -3.027376345333614438, 5.243569643749998122 ) ) ;
#5499 = CARTESIAN_POINT ( 'NONE',  ( 20.40000000122903145, -2.886751345948125991, -5.000000000000000000 ) ) ;
#5500 = CARTESIAN_POINT ( 'NONE',  ( 14.48437500061451821, 4.541064518000418104, 2.621784821874999949 ) ) ;
#5501 = CARTESIAN_POINT ( 'NONE',  ( 4.243569643749999898, 12.39687500061451608, 32.45002607614398471 ) ) ;
#5502 = CARTESIAN_POINT ( 'NONE',  ( 22.42500000122903359, 2.886751345948126879, 4.999999999999999112 ) ) ;
#5503 = VECTOR ( 'NONE', #72848, 1000.000000000000000 ) ;
#5504 = CARTESIAN_POINT ( 'NONE',  ( 17.91562500061451502, 3.027376345333613106, -5.243569643749998122 ) ) ;
#5505 = ORIENTED_EDGE ( 'NONE', *, *, #48083, .F. ) ;
#5506 = VERTEX_POINT ( 'NONE', #62428 ) ;
#5507 = CARTESIAN_POINT ( 'NONE',  ( 19.98749999999999716, 5.773502691896255534, 3.535250795749688894E-16 ) ) ;
#5508 = DIRECTION ( 'NONE',  ( 0.000000000000000000, 0.000000000000000000, 1.000000000000000000 ) ) ;
#5509 = CARTESIAN_POINT ( 'NONE',  ( 25.41562500061451146, -6.054752690667223547, -1.112240025338166033E-15 ) ) ;
#5510 = CARTESIAN_POINT ( 'NONE',  ( 0.2755985575760803163, 4.994312242614637576, 33.99289732352644933 ) ) ;
#5511 = CARTESIAN_POINT ( 'NONE',  ( 16.76250000122903216, -4.330127018922190985, -2.500000000000001332 ) ) ;
#5512 = CARTESIAN_POINT ( 'NONE',  ( 21.59062500061451928, 6.054752690667223547, 3.707466751127219781E-16 ) ) ;
#5513 = CARTESIAN_POINT ( 'NONE',  ( 24.59062500061451573, -3.027376345333610441, -5.243569643749999898 ) ) ;
#5514 = CARTESIAN_POINT ( 'NONE',  ( 5.315625000614516260, 3.027376345333613106, -5.243569643749998122 ) ) ;
#5515 =( BOUNDED_CURVE ( )  B_SPLINE_CURVE ( 2, ( #70208, #47312, #1903, #58744, #59476, #24407, #69846, #30683, #19212 ),
 .UNSPECIFIED., .F., .F. ) 
 B_SPLINE_CURVE_WITH_KNOTS ( ( 3, 2, 2, 2, 3 ),
 ( 0.2065217391304347838, 0.2101449275362318736, 0.2173913043478260809, 0.2246376811594202882, 0.2282608695652174058 ),
 .UNSPECIFIED. ) 
 CURVE ( )  GEOMETRIC_REPRESENTATION_ITEM ( )  RATIONAL_B_SPLINE_CURVE ( ( 0.9330127018922194093, 0.9330127018922194093, 1.000000000000000000, 0.8660254037844387076, 1.000000000000000000, 0.8660254037844387076, 1.000000000000000000, 0.9330127018922190762, 0.9330127018922194093 ) ) 
 REPRESENTATION_ITEM ( '' )  );
#5516 = ORIENTED_EDGE ( 'NONE', *, *, #41396, .T. ) ;
#5517 = CARTESIAN_POINT ( 'NONE',  ( 29.66249999999999432, -5.773502691896255534, -1.060575238724906372E-15 ) ) ;
#5518 = CARTESIAN_POINT ( 'NONE',  ( -3.999999999999999112, 13.08124999877096606, 27.69059892324149530 ) ) ;
#5519 = CARTESIAN_POINT ( 'NONE',  ( 12.64687500061451608, 5.492252693125287522, 3.363034840372157021E-16 ) ) ;
#5520 = CARTESIAN_POINT ( 'NONE',  ( 0.000000000000000000, 20.00000000000000000, -30.00000000000000000 ) ) ;
#5521 = CARTESIAN_POINT ( 'NONE',  ( 1.999999999999998668, 10.96250000122903501, -33.46410161513775705 ) ) ;
#5522 = CARTESIAN_POINT ( 'NONE',  ( 4.243569643749999898, 18.24687500061451928, -27.54997392385601529 ) ) ;
#5523 = CARTESIAN_POINT ( 'NONE',  ( 7.950000000000001954, 0.000000000000000000, 4.999999999999998224 ) ) ;
#5524 = CARTESIAN_POINT ( 'NONE',  ( 3.675000001229035362, -5.773502691896255534, -1.060575238724906372E-15 ) ) ;
#5525 = CARTESIAN_POINT ( 'NONE',  ( 11.82187500061451679, 3.027376345333611329, 5.243569643749999010 ) ) ;
#5526 = CARTESIAN_POINT ( 'NONE',  ( 19.46250000122903145, -4.330127018922190985, -2.500000000000001332 ) ) ;
#5527 = CARTESIAN_POINT ( 'NONE',  ( 3.459375000614519635, -4.541064518000417216, -2.621784821875001281 ) ) ;
#5528 = CARTESIAN_POINT ( 'NONE',  ( 12.18749999999999645, -2.886751345948181946, -4.999999999999904077 ) ) ;
#5529 = VECTOR ( 'NONE', #60915, 1000.000000000000000 ) ;
#5530 = CARTESIAN_POINT ( 'NONE',  ( 12.58125000122903359, -4.330127018922194537, 2.499999999999995559 ) ) ;
#5531 = CARTESIAN_POINT ( 'NONE',  ( 10.88437500061451679, 4.541064518000418104, 2.621784821874999949 ) ) ;
#5532 = DIRECTION ( 'NONE',  ( -1.000000000000000000, -0.000000000000000000, -0.000000000000000000 ) ) ;
#5533 = CARTESIAN_POINT ( 'NONE',  ( 19.00312500061451715, 0.000000000000000000, 5.243569643749999010 ) ) ;
#5534 = CARTESIAN_POINT ( 'NONE',  ( 19.42499999999999716, 6.123233995736764310E-16, -4.999999999999998224 ) ) ;
#5535 = CARTESIAN_POINT ( 'NONE',  ( 4.243569643749999898, 18.22812500061459673, 30.00000000000000000 ) ) ;
#5536 = CARTESIAN_POINT ( 'NONE',  ( 24.75937500061451502, 4.541064518000418104, -2.621784821874998173 ) ) ;
#5537 = DIRECTION ( 'NONE',  ( 0.000000000000000000, 0.000000000000000000, -1.000000000000000000 ) ) ;
#5538 = CARTESIAN_POINT ( 'NONE',  ( 28.76250000122903216, 0.000000000000000000, 4.999999999999998224 ) ) ;
#5539 = CARTESIAN_POINT ( 'NONE',  ( 20.55937500061451217, 2.746126346562645981, -4.756430356249997438 ) ) ;
#5540 = CARTESIAN_POINT ( 'NONE',  ( 25.71562500061451573, 3.027376345333611329, 5.243569643749999010 ) ) ;
#5541 = CARTESIAN_POINT ( 'NONE',  ( 15.32812500061451644, 4.541064518000418104, 2.621784821874999949 ) ) ;
#5542 = CARTESIAN_POINT ( 'NONE',  ( 14.90625000122903110, -4.330127018922190985, -2.500000000000001332 ) ) ;
#5543 = CARTESIAN_POINT ( 'NONE',  ( 11.48437500061451644, -4.541064518000419881, 2.621784821874995952 ) ) ;
#5544 = CARTESIAN_POINT ( 'NONE',  ( 29.21249999999999858, -5.773502691896255534, -1.060575238724906372E-15 ) ) ;
#5545 = CARTESIAN_POINT ( 'NONE',  ( 23.81250000122903288, 0.000000000000000000, 4.999999999999998224 ) ) ;
#5546 = CARTESIAN_POINT ( 'NONE',  ( 3.121875000614518836, 3.027376345333613106, -5.243569643749998122 ) ) ;
#5547 = CARTESIAN_POINT ( 'NONE',  ( 14.40937500061451715, 4.541064518000418104, -2.621784821874998173 ) ) ;
#5548 = CARTESIAN_POINT ( 'NONE',  ( 29.03437500061451715, -4.541064518000419881, 2.621784821874995952 ) ) ;
#5549 = DIRECTION ( 'NONE',  ( 0.000000000000000000, 0.000000000000000000, -1.000000000000000000 ) ) ;
#5550 = CARTESIAN_POINT ( 'NONE',  ( -1.999999999999997113, 12.42500000000000249, -26.53589838486224295 ) ) ;
#5551 = CARTESIAN_POINT ( 'NONE',  ( 24.53437500061451715, -4.541064518000419881, 2.621784821874995952 ) ) ;
#5552 = CARTESIAN_POINT ( 'NONE',  ( 14.10937500061451644, 0.000000000000000000, 5.243569643749999010 ) ) ;
#5553 = CARTESIAN_POINT ( 'NONE',  ( 2.655984681222220721E-16, 15.56562499938548250, 25.66244784525396483 ) ) ;
#5554 = EDGE_CURVE ( 'NONE', #8225, #63037, #22891, .T. ) ;
#5555 = CARTESIAN_POINT ( 'NONE',  ( 28.42499999999999716, 6.123233995736764310E-16, -4.999999999999998224 ) ) ;
#5556 = CARTESIAN_POINT ( 'NONE',  ( 3.075000001229035718, 2.886751345948126879, 4.999999999999999112 ) ) ;
#5557 = CARTESIAN_POINT ( 'NONE',  ( 7.546875000614516438, 4.119189519843966529, -2.378215178124998275 ) ) ;
#5558 = CARTESIAN_POINT ( 'NONE',  ( 16.82812500061451644, -4.541064518000419881, 2.621784821874995952 ) ) ;
#5559 = CARTESIAN_POINT ( 'NONE',  ( 8.400000000000000355, 0.000000000000000000, 4.999999999999998224 ) ) ;
#5560 = CARTESIAN_POINT ( 'NONE',  ( -3.999999999999997335, 14.18750000000000000, 32.30940107675850470 ) ) ;
#5561 = CARTESIAN_POINT ( 'NONE',  ( 16.27499999999999858, 6.123233995736764310E-16, -4.999999999999998224 ) ) ;
#5562 = EDGE_CURVE ( 'NONE', #69508, #51457, #45449, .T. ) ;
#5563 = CARTESIAN_POINT ( 'NONE',  ( -4.243569643749997233, 13.54062500061451679, 32.45002607614398471 ) ) ;
#5564 = CARTESIAN_POINT ( 'NONE',  ( 21.41250000122903074, 4.330127018922192761, -2.499999999999997780 ) ) ;
#5565 = CARTESIAN_POINT ( 'NONE',  ( 5.672204065618860369, 8.235970573989481736, 31.96601703155577212 ) ) ;
#5566 = CARTESIAN_POINT ( 'NONE',  ( 26.82187500061451857, -6.054752690667223547, -1.112240025338166033E-15 ) ) ;
#5567 = ORIENTED_EDGE ( 'NONE', *, *, #16122, .F. ) ;
#5568 = CARTESIAN_POINT ( 'NONE',  ( 17.72812500061451502, -4.541064518000419881, 2.621784821874995952 ) ) ;
#5569 = CARTESIAN_POINT ( 'NONE',  ( 22.49062500061451431, 6.054752690667223547, 3.707466751127219781E-16 ) ) ;
#5570 = CARTESIAN_POINT ( 'NONE',  ( 22.24687500061451217, -3.027376345333614438, 5.243569643749998122 ) ) ;
#5571 = CARTESIAN_POINT ( 'NONE',  ( 7.012500000000001066, 2.886751345948126879, 4.999999999999999112 ) ) ;
#5572 = CARTESIAN_POINT ( 'NONE',  ( 9.440625000614517148, 6.054752690667223547, 3.707466751127219781E-16 ) ) ;
#5573 = CARTESIAN_POINT ( 'NONE',  ( 24.36562500061451786, 3.027376345333611329, 5.243569643749999010 ) ) ;
#5574 = CARTESIAN_POINT ( 'NONE',  ( 15.30937500061451750, 4.541064518000418104, -2.621784821874998173 ) ) ;
#5575 = CARTESIAN_POINT ( 'NONE',  ( 18.30937500061451928, -4.541064518000417216, -2.621784821875001281 ) ) ;
#5576 = DIRECTION ( 'NONE',  ( 0.000000000000000000, 0.000000000000000000, 1.000000000000000000 ) ) ;
#5577 = CARTESIAN_POINT ( 'NONE',  ( -4.243569643749999898, 16.61562500061451786, 27.54997392385601529 ) ) ;
#5578 = CARTESIAN_POINT ( 'NONE',  ( 22.27500000122903145, 2.886751345948129099, -4.999999999999998224 ) ) ;
#5579 = CARTESIAN_POINT ( 'NONE',  ( 15.53437500061451715, -4.119189519843968306, 2.378215178124996054 ) ) ;
#5580 = CARTESIAN_POINT ( 'NONE',  ( 12.02812500061451573, 6.421520780324663323E-16, -5.243569643749999010 ) ) ;
#5581 = CARTESIAN_POINT ( 'NONE',  ( 6.421875000614519102, 3.027376345333611329, 5.243569643749999010 ) ) ;
#5582 = CARTESIAN_POINT ( 'NONE',  ( 3.871875000614519280, -6.054752690667223547, -1.112240025338166033E-15 ) ) ;
#5583 = EDGE_CURVE ( 'NONE', #3561, #64855, #13260, .T. ) ;
#5584 = ORIENTED_EDGE ( 'NONE', *, *, #36389, .F. ) ;
#5585 = CARTESIAN_POINT ( 'NONE',  ( 28.02187500061451431, 3.027376345333611329, 5.243569643749999010 ) ) ;
#5586 = CARTESIAN_POINT ( 'NONE',  ( 20.46562500061451928, -6.054752690667223547, -1.112240025338166033E-15 ) ) ;
#5587 = CARTESIAN_POINT ( 'NONE',  ( 28.05000000122903359, -2.886751345948125991, -5.000000000000000000 ) ) ;
#5588 = CARTESIAN_POINT ( 'NONE',  ( 27.02812500061451573, 4.541064518000418104, 2.621784821874999949 ) ) ;
#5589 = CARTESIAN_POINT ( 'NONE',  ( 24.42187500061451999, 3.027376345333611329, 5.243569643749999010 ) ) ;
#5590 = CARTESIAN_POINT ( 'NONE',  ( 17.87812500061451715, 6.421520780324663323E-16, -5.243569643749999010 ) ) ;
#5591 = CARTESIAN_POINT ( 'NONE',  ( -1.389182184750238802, 10.01354716596406824, 26.18324255480197493 ) ) ;
#5592 = CARTESIAN_POINT ( 'NONE',  ( 23.91562500061451502, 3.027376345333611329, 5.243569643749999010 ) ) ;
#5593 = CARTESIAN_POINT ( 'NONE',  ( 4.987500001229032698, -4.330127018922194537, 2.499999999999995559 ) ) ;
#5594 = ORIENTED_EDGE ( 'NONE', *, *, #48575, .T. ) ;
#5595 = CARTESIAN_POINT ( 'NONE',  ( 27.37500000000000000, -4.330127018922194537, 2.499999999999995559 ) ) ;
#5596 = CARTESIAN_POINT ( 'NONE',  ( -3.999999999999999112, 15.05000000000000071, -30.00000000000000000 ) ) ;
#5597 = CARTESIAN_POINT ( 'NONE',  ( 3.756430356249998770, 16.76562499938548356, 32.16877607737302469 ) ) ;
#5598 = CARTESIAN_POINT ( 'NONE',  ( 5.746875000614517504, -3.027376345333610441, -5.243569643749999898 ) ) ;
#5599 = CARTESIAN_POINT ( 'NONE',  ( 10.64062500061451644, -3.027376345333610441, -5.243569643749999898 ) ) ;
#5600 = CARTESIAN_POINT ( 'NONE',  ( 6.496875000614517504, -3.027376345333614438, 5.243569643749998122 ) ) ;
#5601 = CARTESIAN_POINT ( 'NONE',  ( 24.33750000122903145, -4.330127018922194537, 2.499999999999995559 ) ) ;
#5602 = AXIS2_PLACEMENT_3D ( 'NONE', #51225, #24581, #69659 ) ;
#5603 = CARTESIAN_POINT ( 'NONE',  ( 15.08437500061451786, -4.541064518000419881, 2.621784821874995952 ) ) ;
#5604 = CARTESIAN_POINT ( 'NONE',  ( 29.65312500061451573, 4.541064518000418104, -2.621784821874998173 ) ) ;
#5605 = CARTESIAN_POINT ( 'NONE',  ( 27.52500000000000213, 6.123233995736764310E-16, -4.999999999999998224 ) ) ;
#5606 = CARTESIAN_POINT ( 'NONE',  ( 27.75937500061451502, -4.541064518000417216, -2.621784821875001281 ) ) ;
#5607 = CARTESIAN_POINT ( 'NONE',  ( 3.215625000614518836, 3.027376345333611329, 5.243569643749999010 ) ) ;
#5608 = CARTESIAN_POINT ( 'NONE',  ( 13.22812500061451502, -4.541064518000419881, 2.621784821874995952 ) ) ;
#5609 = ORIENTED_EDGE ( 'NONE', *, *, #2386, .T. ) ;
#5610 = CARTESIAN_POINT ( 'NONE',  ( 9.065625000614517148, 3.027376345333611329, 5.243569643749999010 ) ) ;
#5611 = CARTESIAN_POINT ( 'NONE',  ( 6.290625000614517681, 6.054752690667223547, 3.707466751127219781E-16 ) ) ;
#5612 = CARTESIAN_POINT ( 'NONE',  ( 17.78437500061451715, -4.119189519843968306, 2.378215178124996054 ) ) ;
#5613 = DIRECTION ( 'NONE',  ( 0.000000000000000000, -1.000000000000000000, 8.673617379884035472E-17 ) ) ;
#5614 = CARTESIAN_POINT ( 'NONE',  ( 15.00000000000000000, 4.330127018922192761, -2.499999999999997780 ) ) ;
#5615 = CARTESIAN_POINT ( 'NONE',  ( 16.32187500061451502, 3.027376345333611329, 5.243569643749999010 ) ) ;
#5616 = B_SPLINE_CURVE_WITH_KNOTS ( 'NONE', 3,
 ( #19471, #41306, #19842, #12851, #35384, #8770, #42394, #63816, #42029, #14307 ),
 .UNSPECIFIED., .F., .F.,
 ( 4, 3, 3, 4 ),
 ( 0.000000000000000000, 0.0001572298629325321207, 0.0003312541060196098224, 0.0005053537190665100551 ),
 .UNSPECIFIED. ) ;
#5617 = CARTESIAN_POINT ( 'NONE',  ( 12.48750000122903359, 4.330127018922191873, 2.499999999999999556 ) ) ;
#5618 = CARTESIAN_POINT ( 'NONE',  ( 20.85000000000000142, 4.330127018922192761, -2.499999999999997780 ) ) ;
#5619 = CARTESIAN_POINT ( 'NONE',  ( 20.82187500061451857, 3.027376345333611329, 5.243569643749999010 ) ) ;
#5620 = CARTESIAN_POINT ( 'NONE',  ( 2.121784821875001281, 14.10312500061451679, -26.32496088578401938 ) ) ;
#5621 = DIRECTION ( 'NONE',  ( 0.000000000000000000, 0.000000000000000000, -1.000000000000000000 ) ) ;
#5622 = CARTESIAN_POINT ( 'NONE',  ( 24.49687500061451573, -4.119189519843965641, -2.378215178125001383 ) ) ;
#5623 = CARTESIAN_POINT ( 'NONE',  ( 4.111889464957033447, 2.844708250062874644, 4.404844785106587501 ) ) ;
#5624 = CARTESIAN_POINT ( 'NONE',  ( 26.09062500061451573, 6.054752690667223547, 3.707466751127219781E-16 ) ) ;
#5625 = CARTESIAN_POINT ( 'NONE',  ( 1.510657702057710734E-15, 19.43750000000000000, -33.99999999999999289 ) ) ;
#5626 = DIRECTION ( 'NONE',  ( 0.000000000000000000, 0.000000000000000000, 1.000000000000000000 ) ) ;
#5627 = CARTESIAN_POINT ( 'NONE',  ( 27.29999999999999716, 0.000000000000000000, 4.999999999999998224 ) ) ;
#5628 = CARTESIAN_POINT ( 'NONE',  ( 9.103125000614515017, 0.000000000000000000, 5.243569643749999010 ) ) ;
#5629 = CARTESIAN_POINT ( 'NONE',  ( 26.10937500061451644, 2.746126346562643317, 4.756430356249998326 ) ) ;
#5630 = CARTESIAN_POINT ( 'NONE',  ( 19.88437500061451857, 4.541064518000418104, 2.621784821874999949 ) ) ;
#5631 = CARTESIAN_POINT ( 'NONE',  ( 12.49687500061451573, 4.119189519843966529, -2.378215178124998275 ) ) ;
#5632 = CARTESIAN_POINT ( 'NONE',  ( 5.615625000614517859, -6.054752690667223547, -1.112240025338166033E-15 ) ) ;
#5633 = CARTESIAN_POINT ( 'NONE',  ( 11.40937500061451892, 0.000000000000000000, 5.243569643749999010 ) ) ;
#5634 = ORIENTED_EDGE ( 'NONE', *, *, #39334, .F. ) ;
#5635 = CARTESIAN_POINT ( 'NONE',  ( 21.57187500061451502, 3.027376345333613106, -5.243569643749998122 ) ) ;
#5636 = CARTESIAN_POINT ( 'NONE',  ( 16.57499999999999929, -4.330127018922194537, 2.499999999999995559 ) ) ;
#5637 = CARTESIAN_POINT ( 'NONE',  ( 29.58749999999999858, -2.886751345948129988, 4.999999999999997335 ) ) ;
#5638 = CARTESIAN_POINT ( 'NONE',  ( 6.150000000000003020, 0.000000000000000000, 4.999999999999998224 ) ) ;
#5639 = VECTOR ( 'NONE', #24621, 1000.000000000000000 ) ;
#5640 = CARTESIAN_POINT ( 'NONE',  ( 14.40000000122903323, -2.886751345948129988, 4.999999999999997335 ) ) ;
#5641 = CARTESIAN_POINT ( 'NONE',  ( 1.071796769724489895, 12.32990381179670081, 26.00000000000000355 ) ) ;
#5642 = ORIENTED_EDGE ( 'NONE', *, *, #27759, .T. ) ;
#5643 = CARTESIAN_POINT ( 'NONE',  ( 13.46249999999999858, -5.773502691896255534, -1.060575238724906372E-15 ) ) ;
#5644 = CARTESIAN_POINT ( 'NONE',  ( 26.72812500061451502, -4.541064518000419881, 2.621784821874995952 ) ) ;
#5645 = CARTESIAN_POINT ( 'NONE',  ( 17.66249999999999787, 2.886751345948129099, -4.999999999999998224 ) ) ;
#5646 = CARTESIAN_POINT ( 'NONE',  ( 10.68750000122903288, 4.330127018922191873, 2.499999999999999556 ) ) ;
#5647 = CARTESIAN_POINT ( 'NONE',  ( 8.353125000614518569, -4.541064518000417216, -2.621784821875001281 ) ) ;
#5648 = ADVANCED_FACE ( 'NONE', ( #22181 ), #34709, .T. ) ;
#5649 = CARTESIAN_POINT ( 'NONE',  ( 9.712500000000002132, 2.886751345948126879, 4.999999999999999112 ) ) ;
#5650 = CARTESIAN_POINT ( 'NONE',  ( 15.97500000122903430, 2.886751345948062486, -5.000000000000113687 ) ) ;
#5651 = CARTESIAN_POINT ( 'NONE',  ( 2.121784821874999061, 15.20937500061451786, -33.67503911421598417 ) ) ;
#5652 = CARTESIAN_POINT ( 'NONE',  ( 27.48750000122903359, -4.330127018922194537, 2.499999999999995559 ) ) ;
#5653 = CARTESIAN_POINT ( 'NONE',  ( 1.878215178125000495, 13.61562499938548321, 26.74683588394047007 ) ) ;
#5654 = CARTESIAN_POINT ( 'NONE',  ( 7.724999999999999645, 6.123233995736764310E-16, -4.999999999999998224 ) ) ;
#5655 = CARTESIAN_POINT ( 'NONE',  ( -1.487416814333745711E-14, 16.96250000000000213, -26.00000000000000000 ) ) ;
#5656 = ORIENTED_EDGE ( 'NONE', *, *, #60084, .F. ) ;
#5657 = CARTESIAN_POINT ( 'NONE',  ( 23.76562500061451644, 3.027376345333613106, -5.243569643749998122 ) ) ;
#5658 = CARTESIAN_POINT ( 'NONE',  ( 28.67812500061451431, 6.421520780324663323E-16, -5.243569643749999010 ) ) ;
#5659 = CARTESIAN_POINT ( 'NONE',  ( 28.69687500061451502, -3.027376345333610441, -5.243569643749999898 ) ) ;
#5660 = CARTESIAN_POINT ( 'NONE',  ( 19.24687500061452283, -3.027376345333610441, -5.243569643749999898 ) ) ;
#5661 = CARTESIAN_POINT ( 'NONE',  ( 17.84062500061451573, -3.027376345333610441, -5.243569643749999898 ) ) ;
#5662 = CARTESIAN_POINT ( 'NONE',  ( 9.001249775931846008E-16, 10.46562500061459389, -25.09994784771203058 ) ) ;
#5663 = CARTESIAN_POINT ( 'NONE',  ( 7.115625000614516082, 3.027376345333613106, -5.243569643749998122 ) ) ;
#5664 = CARTESIAN_POINT ( 'NONE',  ( 27.67500000122903359, 2.886751345948129099, -4.999999999999998224 ) ) ;
#5665 = CARTESIAN_POINT ( 'NONE',  ( 23.82187500061451502, 2.746126346562645981, -4.756430356249997438 ) ) ;
#5666 = CARTESIAN_POINT ( 'NONE',  ( 18.21562500061451573, -6.054752690667223547, -1.112240025338166033E-15 ) ) ;
#5667 = DIRECTION ( 'NONE',  ( -0.000000000000000000, -1.000000000000000000, -0.000000000000000000 ) ) ;
#5668 = CARTESIAN_POINT ( 'NONE',  ( 1.878215178124997609, 18.86562499938548143, 33.25316411605952993 ) ) ;
#5669 = CARTESIAN_POINT ( 'NONE',  ( 12.83437500061451786, -4.541064518000419881, 2.621784821874995952 ) ) ;
#5670 = CARTESIAN_POINT ( 'NONE',  ( 12.79687500061451821, -3.027376345333614438, 5.243569643749998122 ) ) ;
#5671 = CARTESIAN_POINT ( 'NONE',  ( 22.54687500061451999, 6.054752690667223547, 3.707466751127219781E-16 ) ) ;
#5672 = ORIENTED_EDGE ( 'NONE', *, *, #16557, .T. ) ;
#5673 = LINE ( 'NONE', #6028, #11145 ) ;
#5674 = CARTESIAN_POINT ( 'NONE',  ( 26.65312500061451573, 0.000000000000000000, 5.243569643749999010 ) ) ;
#5675 = CARTESIAN_POINT ( 'NONE',  ( 26.95312500061451644, 4.541064518000418104, -2.621784821874998173 ) ) ;
#5676 = CARTESIAN_POINT ( 'NONE',  ( 15.09375000122903110, 5.773502691896255534, 3.535250795749688401E-16 ) ) ;
#5677 = CARTESIAN_POINT ( 'NONE',  ( -2.000000000000000000, 16.32499999999999929, 26.53589838486224650 ) ) ;
#5678 = CARTESIAN_POINT ( 'NONE',  ( 6.009375000614519458, 0.000000000000000000, 5.243569643749999010 ) ) ;
#5679 = CARTESIAN_POINT ( 'NONE',  ( 12.82500000122903394, 2.886751345948129099, -4.999999999999998224 ) ) ;
#5680 = CARTESIAN_POINT ( 'NONE',  ( 7.800000001229035362, -2.886751345948125991, -5.000000000000000000 ) ) ;
#5681 = CARTESIAN_POINT ( 'NONE',  ( 28.57500000122903572, 2.886751345948129099, -4.999999999999998224 ) ) ;
#5682 = CARTESIAN_POINT ( 'NONE',  ( -4.000000000000000888, 18.10624999877096641, 32.30940107675850470 ) ) ;
#5683 = CARTESIAN_POINT ( 'NONE',  ( 17.34375000122903288, 5.773502691896255534, 3.535250795749688894E-16 ) ) ;
#5684 = CARTESIAN_POINT ( 'NONE',  ( 11.40937500061451892, 0.000000000000000000, 5.243569643749999010 ) ) ;
#5685 = CARTESIAN_POINT ( 'NONE',  ( 18.30000000000000071, 0.000000000000000000, 4.999999999999998224 ) ) ;
#5686 = CARTESIAN_POINT ( 'NONE',  ( 18.92812500061451431, 4.541064518000418104, 2.621784821874999949 ) ) ;
#5687 = CARTESIAN_POINT ( 'NONE',  ( 12.64687500061451608, 6.054752690667223547, 3.707466751127219781E-16 ) ) ;
#5688 = CARTESIAN_POINT ( 'NONE',  ( 3.853125000614517681, -4.541064518000417216, -2.621784821875001281 ) ) ;
#5689 = CARTESIAN_POINT ( 'NONE',  ( 22.24687500061451573, -3.027376345333614438, 5.243569643749998122 ) ) ;
#5690 = CARTESIAN_POINT ( 'NONE',  ( 8.821875000614518569, -6.054752690667223547, -1.112240025338166033E-15 ) ) ;
#5691 = CARTESIAN_POINT ( 'NONE',  ( 5.953125000614519102, 0.000000000000000000, 5.243569643749999010 ) ) ;
#5692 = CARTESIAN_POINT ( 'NONE',  ( 5.737500001229033586, 4.330127018922191873, 2.499999999999999556 ) ) ;
#5693 = CARTESIAN_POINT ( 'NONE',  ( 20.27812500061451573, 4.541064518000418104, 2.621784821874999949 ) ) ;
#5694 = CARTESIAN_POINT ( 'NONE',  ( 7.275000001229035007, -5.773502691896255534, -1.060575238724906372E-15 ) ) ;
#5695 = CARTESIAN_POINT ( 'NONE',  ( 17.91562500061451502, 3.027376345333613106, -5.243569643749998122 ) ) ;
#5696 = CARTESIAN_POINT ( 'NONE',  ( 13.60312500061451679, 0.000000000000000000, 5.243569643749999010 ) ) ;
#5697 = CARTESIAN_POINT ( 'NONE',  ( 26.93437500061451573, 5.824947211148865298E-16, -4.756430356249998326 ) ) ;
#5698 = CARTESIAN_POINT ( 'NONE',  ( 13.76250000000000107, 2.886751345948126879, 4.999999999999999112 ) ) ;
#5699 = CARTESIAN_POINT ( 'NONE',  ( 8.175000001229031810, -5.773502691896255534, -1.060575238724906372E-15 ) ) ;
#5700 = CARTESIAN_POINT ( 'NONE',  ( 5.653125000614517504, -4.541064518000417216, -2.621784821875001281 ) ) ;
#5701 = EDGE_CURVE ( 'NONE', #68118, #41920, #63150, .T. ) ;
#5702 = CARTESIAN_POINT ( 'NONE',  ( 20.21250000122903145, 0.000000000000000000, 4.999999999999998224 ) ) ;
#5703 = CARTESIAN_POINT ( 'NONE',  ( 27.15000000000000213, 4.330127018922192761, -2.499999999999997780 ) ) ;
#5704 = CARTESIAN_POINT ( 'NONE',  ( -4.243569643749999898, 12.20937500061451608, -30.00000000000000000 ) ) ;
#5705 = CARTESIAN_POINT ( 'NONE',  ( 3.947751918878622757, -3.068428716296062841, 3.947751918878600108 ) ) ;
#5706 = DIRECTION ( 'NONE',  ( -0.000000000000000000, -1.000000000000000000, -0.000000000000000000 ) ) ;
#5707 =( BOUNDED_CURVE ( )  B_SPLINE_CURVE ( 2, ( #19430, #26091, #3936, #41991, #59694, #48629, #31639, #71154, #26459 ),
 .UNSPECIFIED., .F., .F. ) 
 B_SPLINE_CURVE_WITH_KNOTS ( ( 3, 2, 2, 2, 3 ),
 ( 0.6250000000000000000, 0.6296296296296296502, 0.6388888888888888395, 0.6481481481481481399, 0.6527777777777777901 ),
 .UNSPECIFIED. ) 
 CURVE ( )  GEOMETRIC_REPRESENTATION_ITEM ( )  RATIONAL_B_SPLINE_CURVE ( ( 0.9330127018922194093, 0.9330127018922194093, 1.000000000000000000, 0.8660254037844387076, 1.000000000000000000, 0.8660254037844387076, 1.000000000000000000, 0.9330127018922194093, 0.9330127018922194093 ) ) 
 REPRESENTATION_ITEM ( '' )  );
#5708 = CARTESIAN_POINT ( 'NONE',  ( 28.42500000122904069, -5.773502691896255534, -1.060575238724906372E-15 ) ) ;
#5709 = CARTESIAN_POINT ( 'NONE',  ( 20.78437500061451715, 4.541064518000418104, 2.621784821874999949 ) ) ;
#5710 = CARTESIAN_POINT ( 'NONE',  ( 17.50312500061451715, 4.541064518000418104, -2.621784821874998173 ) ) ;
#5711 = CARTESIAN_POINT ( 'NONE',  ( 12.24375000122903323, -2.886751345948125991, -5.000000000000000000 ) ) ;
#5712 = DIRECTION ( 'NONE',  ( -0.000000000000000000, -1.000000000000000000, -0.000000000000000000 ) ) ;
#5713 = CARTESIAN_POINT ( 'NONE',  ( 26.69999999999999929, 4.330127018922192761, -2.499999999999997780 ) ) ;
#5714 = CARTESIAN_POINT ( 'NONE',  ( 27.87187500061451573, 3.027376345333613106, -5.243569643749998122 ) ) ;
#5715 = CARTESIAN_POINT ( 'NONE',  ( 21.60937500061451644, 2.746126346562643317, 4.756430356249998326 ) ) ;
#5716 = CARTESIAN_POINT ( 'NONE',  ( 12.06562500061451537, 3.027376345333613106, -5.243569643749998122 ) ) ;
#5717 = CARTESIAN_POINT ( 'NONE',  ( 10.32187500061451679, 3.027376345333613106, -5.243569643749998122 ) ) ;
#5718 = ORIENTED_EDGE ( 'NONE', *, *, #10486, .F. ) ;
#5719 = CARTESIAN_POINT ( 'NONE',  ( 2.856422355664287593, -4.103760632159477950, -2.967416088732543145 ) ) ;
#5720 = CARTESIAN_POINT ( 'NONE',  ( 22.26562500061451644, -6.054752690667223547, -1.112240025338166033E-15 ) ) ;
#5721 = FACE_OUTER_BOUND ( 'NONE', #31390, .T. ) ;
#5722 = EDGE_CURVE ( 'NONE', #68198, #11370, #43043, .T. ) ;
#5723 = CARTESIAN_POINT ( 'NONE',  ( 10.85625000122903216, -4.330127018922190985, -2.500000000000001332 ) ) ;
#5724 = CARTESIAN_POINT ( 'NONE',  ( 11.40000000000000036, 4.330127018922192761, -2.499999999999997780 ) ) ;
#5725 = CARTESIAN_POINT ( 'NONE',  ( 22.68750000122903288, 6.123233995736764310E-16, -4.999999999999998224 ) ) ;
#5726 = CARTESIAN_POINT ( 'NONE',  ( 15.81562500061451537, 3.027376345333611329, 5.243569643749999010 ) ) ;
#5727 = CARTESIAN_POINT ( 'NONE',  ( 13.50937500061451679, 2.746126346562643317, 4.756430356249998326 ) ) ;
#5728 = ORIENTED_EDGE ( 'NONE', *, *, #36745, .T. ) ;
#5729 = CARTESIAN_POINT ( 'NONE',  ( 20.36249999999999716, 2.886751345948129099, -4.999999999999998224 ) ) ;
#5730 = CARTESIAN_POINT ( 'NONE',  ( 23.81250000000000000, -5.773502691896255534, -1.060575238724906372E-15 ) ) ;
#5731 = CARTESIAN_POINT ( 'NONE',  ( 21.30937500061451573, 0.000000000000000000, 5.243569643749999010 ) ) ;
#5732 = CARTESIAN_POINT ( 'NONE',  ( 24.92812500061451431, -4.541064518000419881, 2.621784821874995952 ) ) ;
#5733 =( BOUNDED_CURVE ( )  B_SPLINE_CURVE ( 2, ( #56705, #45995, #47081, #62969, #29367, #28637, #24170 ),
 .UNSPECIFIED., .F., .F. ) 
 B_SPLINE_CURVE_WITH_KNOTS ( ( 3, 2, 2, 3 ),
 ( 0.9684929749567240398, 0.9694444444444444420, 0.9722222222222222099, 0.9730758100533248856 ),
 .UNSPECIFIED. ) 
 CURVE ( )  GEOMETRIC_REPRESENTATION_ITEM ( )  RATIONAL_B_SPLINE_CURVE ( ( 0.9396570677417193096, 0.9541098134456433844, 1.000000000000000000, 0.8660254037844387076, 1.000000000000000000, 0.9588307293976606749, 0.9429634024444231155 ) ) 
 REPRESENTATION_ITEM ( '' )  );
#5734 = ORIENTED_EDGE ( 'NONE', *, *, #39155, .F. ) ;
#5735 = CARTESIAN_POINT ( 'NONE',  ( 19.08749999999999858, 5.773502691896255534, 3.535250795749688401E-16 ) ) ;
#5736 = CARTESIAN_POINT ( 'NONE',  ( 7.790625000614518569, -3.027376345333614438, 5.243569643749998122 ) ) ;
#5737 = CARTESIAN_POINT ( 'NONE',  ( 29.55000000000000071, 0.000000000000000000, 4.999999999999998224 ) ) ;
#5738 = CARTESIAN_POINT ( 'NONE',  ( 14.88750000000000107, -2.886751345948125991, -5.000000000000000000 ) ) ;
#5739 = CARTESIAN_POINT ( 'NONE',  ( -4.243569643749997233, 19.39062500061451999, 32.45002607614398471 ) ) ;
#5740 = CARTESIAN_POINT ( 'NONE',  ( 4.284375000614518925, -4.541064518000419881, 2.621784821874995952 ) ) ;
#5741 = CARTESIAN_POINT ( 'NONE',  ( 28.28437500061451715, 6.421520780324663323E-16, -5.243569643749999010 ) ) ;
#5742 = EDGE_LOOP ( 'NONE', ( #2005, #57763, #1995, #27992 ) ) ;
#5743 = CARTESIAN_POINT ( 'NONE',  ( 24.47812500061451502, -4.541064518000419881, 2.621784821874995952 ) ) ;
#5744 = CARTESIAN_POINT ( 'NONE',  ( 26.48437500061451644, 6.421520780324663323E-16, -5.243569643749999010 ) ) ;
#5745 = CARTESIAN_POINT ( 'NONE',  ( -4.243569643749998122, 19.39062500061459104, -27.54997392385601174 ) ) ;
#5746 = CARTESIAN_POINT ( 'NONE',  ( 10.80000000000000071, -4.330127018922190985, -2.500000000000001332 ) ) ;
#5747 = CARTESIAN_POINT ( 'NONE',  ( 8.465625000614515727, 3.027376345333613106, -5.243569643749998122 ) ) ;
#5748 = CARTESIAN_POINT ( 'NONE',  ( 2.393811435568372112E-14, 17.28124999877096712, 34.00000000000000000 ) ) ;
#5749 = CARTESIAN_POINT ( 'NONE',  ( 19.61249999999999716, 2.886751345948093572, 5.000000000000056843 ) ) ;
#5750 = CARTESIAN_POINT ( 'NONE',  ( 27.51562500061451644, 3.027376345333611329, 5.243569643749999010 ) ) ;
#5751 = CARTESIAN_POINT ( 'NONE',  ( 29.40937500061451360, -5.492252693125287522, -1.008910452111647106E-15 ) ) ;
#5752 = CARTESIAN_POINT ( 'NONE',  ( 13.05937500061451750, 4.119189519843966529, -2.378215178124998275 ) ) ;
#5753 = CARTESIAN_POINT ( 'NONE',  ( 2.990625000614519191, -3.027376345333610441, -5.243569643749999898 ) ) ;
#5754 = CARTESIAN_POINT ( 'NONE',  ( 18.94687500061451502, 6.054752690667223547, 3.707466751127219781E-16 ) ) ;
#5755 = CARTESIAN_POINT ( 'NONE',  ( -4.243569643749999898, 15.80937500061451573, 30.00000000000000000 ) ) ;
#5756 = CARTESIAN_POINT ( 'NONE',  ( 22.69687500061451857, -3.027376345333614438, 5.243569643749998122 ) ) ;
#5758 = EDGE_CURVE ( 'NONE', #964, #27078, #20525, .T. ) ;
#5757 = CARTESIAN_POINT ( 'NONE',  ( 3.712499999999999911, 2.886751345948129099, -4.999999999999998224 ) ) ;
#5759 = CARTESIAN_POINT ( 'NONE',  ( -2.121784821874999949, 18.88437500061451857, 26.32496088578401938 ) ) ;
#5760 = CARTESIAN_POINT ( 'NONE',  ( 10.34062500061451750, 6.054752690667223547, 3.707466751127219781E-16 ) ) ;
#5761 = CARTESIAN_POINT ( 'NONE',  ( 19.93125000122903145, 6.123233995736764310E-16, -4.999999999999998224 ) ) ;
#5762 = CARTESIAN_POINT ( 'NONE',  ( 7.434375000614519280, -4.541064518000419881, 2.621784821874995952 ) ) ;
#5763 = CARTESIAN_POINT ( 'NONE',  ( -3.999999999999997335, 16.10000000122903430, -27.69059892324149530 ) ) ;
#5764 =( BOUNDED_CURVE ( )  B_SPLINE_CURVE ( 2, ( #12387, #7934, #30472, #36375, #13457, #58524, #17914, #62992, #35282 ),
 .UNSPECIFIED., .F., .F. ) 
 B_SPLINE_CURVE_WITH_KNOTS ( ( 3, 2, 2, 2, 3 ),
 ( 0.7638888888888889506, 0.7685185185185184897, 0.7777777777777777901, 0.7870370370370370905, 0.7916666666666667407 ),
 .UNSPECIFIED. ) 
 CURVE ( )  GEOMETRIC_REPRESENTATION_ITEM ( )  RATIONAL_B_SPLINE_CURVE ( ( 0.9330127018922192983, 0.9330127018922200755, 1.000000000000000000, 0.8660254037844387076, 1.000000000000000000, 0.8660254037844387076, 1.000000000000000000, 0.9330127018922185211, 0.9330127018922192983 ) ) 
 REPRESENTATION_ITEM ( '' )  );
#5765 = CARTESIAN_POINT ( 'NONE',  ( 6.440625000614517148, -3.027376345333614438, 5.243569643749998122 ) ) ;
#5766 = CARTESIAN_POINT ( 'NONE',  ( 12.34687500061452070, -3.027376345333614438, 5.243569643749998122 ) ) ;
#5767 = CARTESIAN_POINT ( 'NONE',  ( 19.23750000122903714, 4.330127018922191873, 2.499999999999999556 ) ) ;
#5768 = CARTESIAN_POINT ( 'NONE',  ( 7.246875000614518392, 6.054752690667223547, 3.707466751127219781E-16 ) ) ;
#5769 = CARTESIAN_POINT ( 'NONE',  ( 8.878125000614515372, 6.421520780324663323E-16, -5.243569643749999010 ) ) ;
#5770 = CARTESIAN_POINT ( 'NONE',  ( 5.503125000614516260, 0.000000000000000000, 5.243569643749999010 ) ) ;
#5771 = CARTESIAN_POINT ( 'NONE',  ( 26.11875000122902790, -5.773502691896255534, -1.060575238724906372E-15 ) ) ;
#5772 = CARTESIAN_POINT ( 'NONE',  ( 20.07187500061451857, -6.054752690667223547, -1.112240025338166033E-15 ) ) ;
#5773 = CARTESIAN_POINT ( 'NONE',  ( 18.22499999999999787, 4.330127018922191873, 2.499999999999999556 ) ) ;
#5774 = CARTESIAN_POINT ( 'NONE',  ( 27.32812500061451644, 6.421520780324663323E-16, -5.243569643749999010 ) ) ;
#5775 = CARTESIAN_POINT ( 'NONE',  ( 12.44062500061451537, -3.027376345333610441, -5.243569643749999898 ) ) ;
#5776 = CARTESIAN_POINT ( 'NONE',  ( -2.928932188134523606, -4.999999999999997335, 2.928932188134523606 ) ) ;
#5777 = CARTESIAN_POINT ( 'NONE',  ( 4.509957931155624600, -2.159147578587980121, -4.574533615465857572 ) ) ;
#5778 = CARTESIAN_POINT ( 'NONE',  ( 13.01250000122903394, 0.000000000000000000, 4.999999999999998224 ) ) ;
#5779 = CARTESIAN_POINT ( 'NONE',  ( 26.76562500061451644, -6.054752690667223547, -1.112240025338166033E-15 ) ) ;
#5780 = CARTESIAN_POINT ( 'NONE',  ( -4.243569643749999898, 14.85312500061451679, -30.00000000000000000 ) ) ;
#5781 = CARTESIAN_POINT ( 'NONE',  ( 15.71250000122903501, 0.000000000000000000, 4.999999999999998224 ) ) ;
#5782 = CARTESIAN_POINT ( 'NONE',  ( 14.51250000000000107, 2.886751345948129099, -4.999999999999998224 ) ) ;
#5783 = CARTESIAN_POINT ( 'NONE',  ( 23.72812500061451502, 6.421520780324663323E-16, -5.243569643749999010 ) ) ;
#5784 = CARTESIAN_POINT ( 'NONE',  ( 8.296875000614518214, -3.027376345333614438, 5.243569643749998122 ) ) ;
#5785 = CARTESIAN_POINT ( 'NONE',  ( 6.975000001229032520, 2.886751345948129099, -4.999999999999998224 ) ) ;
#5786 = CARTESIAN_POINT ( 'NONE',  ( 15.75000000122902932, -2.886751345948129988, 4.999999999999997335 ) ) ;
#5787 = CARTESIAN_POINT ( 'NONE',  ( 12.36562500061451608, -6.054752690667223547, -1.112240025338166033E-15 ) ) ;
#5788 = CARTESIAN_POINT ( 'NONE',  ( 15.25312500061451715, 4.541064518000418104, -2.621784821874998173 ) ) ;
#5789 = CARTESIAN_POINT ( 'NONE',  ( 27.11250000122903359, -4.330127018922190985, -2.500000000000001332 ) ) ;
#5790 = CARTESIAN_POINT ( 'NONE',  ( 23.73749999999999716, -2.886751345948129988, 4.999999999999997335 ) ) ;
#5791 = CARTESIAN_POINT ( 'NONE',  ( 22.35937500061451644, -4.541064518000417216, -2.621784821875001281 ) ) ;
#5792 = DIRECTION ( 'NONE',  ( 0.000000000000000000, 0.000000000000000000, -1.000000000000000000 ) ) ;
#5793 = CARTESIAN_POINT ( 'NONE',  ( 10.16250000122903252, 4.330127018922192761, -2.499999999999997780 ) ) ;
#5794 = CARTESIAN_POINT ( 'NONE',  ( 27.49687500061451217, 6.054752690667223547, 3.707466751127219781E-16 ) ) ;
#5795 = EDGE_CURVE ( 'NONE', #24462, #11954, #63319, .T. ) ;
#5796 = CARTESIAN_POINT ( 'NONE',  ( 5.896875000614518747, 6.054752690667223547, 3.707466751127219781E-16 ) ) ;
#5797 = CARTESIAN_POINT ( 'NONE',  ( 24.74062500061451786, 6.054752690667223547, 3.707466751127219781E-16 ) ) ;
#5798 = CARTESIAN_POINT ( 'NONE',  ( -7.967954043666661671E-16, 15.79062499938548392, 34.33755215474603517 ) ) ;
#5799 = CARTESIAN_POINT ( 'NONE',  ( 6.975000000000002309, 4.330127018922191873, 2.499999999999999556 ) ) ;
#5800 = CARTESIAN_POINT ( 'NONE',  ( 9.346875000614517148, -3.027376345333610441, -5.243569643749999898 ) ) ;
#5801 = CARTESIAN_POINT ( 'NONE',  ( 1.999999999999998668, 12.65000000000000213, 26.53589838486224650 ) ) ;
#5802 = CARTESIAN_POINT ( 'NONE',  ( 3.759375000614517681, 0.000000000000000000, 5.243569643749999010 ) ) ;
#5803 = CARTESIAN_POINT ( 'NONE',  ( 6.196875000614515905, -3.027376345333610441, -5.243569643749999898 ) ) ;
#5804 = CARTESIAN_POINT ( 'NONE',  ( -3.999999999999999112, 14.60000000000000142, 30.00000000000000000 ) ) ;
#5805 = CARTESIAN_POINT ( 'NONE',  ( 26.37187500061451217, -6.054752690667223547, -1.112240025338166033E-15 ) ) ;
#5806 = CARTESIAN_POINT ( 'NONE',  ( -3.000416591977282496E-16, 10.69062500061459531, 25.09994784771203058 ) ) ;
#5807 = CARTESIAN_POINT ( 'NONE',  ( 18.75000000000000000, 0.000000000000000000, 4.999999999999998224 ) ) ;
#5808 = ORIENTED_EDGE ( 'NONE', *, *, #65184, .T. ) ;
#5809 = CARTESIAN_POINT ( 'NONE',  ( 27.71250000000000568, 2.886751345948126879, 4.999999999999999112 ) ) ;
#5810 = CARTESIAN_POINT ( 'NONE',  ( 29.52187500061451431, -6.054752690667223547, -1.112240025338166033E-15 ) ) ;
#5811 = EDGE_LOOP ( 'NONE', ( #62244, #57255, #12547, #27686 ) ) ;
#5812 = CARTESIAN_POINT ( 'NONE',  ( 14.91562500061451679, 3.027376345333611329, 5.243569643749999010 ) ) ;
#5813 = CARTESIAN_POINT ( 'NONE',  ( 8.353125000614518569, -4.541064518000417216, -2.621784821875001281 ) ) ;
#5814 = CARTESIAN_POINT ( 'NONE',  ( 18.08437500061451075, -2.746126346562646425, 4.756430356249996549 ) ) ;
#5815 = CARTESIAN_POINT ( 'NONE',  ( 4.959375000614516971, 4.541064518000418104, -2.621784821874998173 ) ) ;
#5816 = CARTESIAN_POINT ( 'NONE',  ( 17.25000000122903288, -2.886751345948125991, -5.000000000000000000 ) ) ;
#5817 = CARTESIAN_POINT ( 'NONE',  ( 22.38749999999999929, -2.886751345948129988, 4.999999999999997335 ) ) ;
#5818 = DIRECTION ( 'NONE',  ( 1.000000000000000000, 0.000000000000000000, 0.000000000000000000 ) ) ;
#5819 = CARTESIAN_POINT ( 'NONE',  ( 6.609375000614519102, -4.541064518000417216, -2.621784821875001281 ) ) ;
#5820 = CARTESIAN_POINT ( 'NONE',  ( 11.67187500061451821, 3.027376345333613106, -5.243569643749998122 ) ) ;
#5821 = CARTESIAN_POINT ( 'NONE',  ( 21.98437500061451644, 6.421520780324663323E-16, -5.243569643749999010 ) ) ;
#5822 = CARTESIAN_POINT ( 'NONE',  ( 26.81250000000000000, 2.886751345948126879, 4.999999999999998224 ) ) ;
#5823 = ORIENTED_EDGE ( 'NONE', *, *, #15041, .T. ) ;
#5824 = CARTESIAN_POINT ( 'NONE',  ( 3.346875000614518036, -3.027376345333614438, 5.243569643749998122 ) ) ;
#5826 = EDGE_CURVE ( 'NONE', #42194, #1783, #70886, .T. ) ;
#5825 = CARTESIAN_POINT ( 'NONE',  ( 5.859375000614519102, 4.541064518000418104, -2.621784821874998173 ) ) ;
#5827 = CARTESIAN_POINT ( 'NONE',  ( 18.59999999999999787, 4.330127018922192761, -2.499999999999997780 ) ) ;
#5828 = CARTESIAN_POINT ( 'NONE',  ( 15.66562500061451857, 3.027376345333613106, -5.243569643749998122 ) ) ;
#5829 = CARTESIAN_POINT ( 'NONE',  ( -4.000000000000000888, 16.81250000000000000, 32.30940107675850470 ) ) ;
#5830 = CARTESIAN_POINT ( 'NONE',  ( 23.59687500061451715, -2.746126346562646425, 4.756430356249996549 ) ) ;
#5831 = CARTESIAN_POINT ( 'NONE',  ( 10.34062500061451750, 6.054752690667223547, 3.707466751127219781E-16 ) ) ;
#5832 = CARTESIAN_POINT ( 'NONE',  ( 26.18437500061451573, 4.541064518000418104, 2.621784821874999949 ) ) ;
#5833 = CARTESIAN_POINT ( 'NONE',  ( -1.071796769724490561, 19.57009619066136707, 26.00000000000000000 ) ) ;
#5834 = CARTESIAN_POINT ( 'NONE',  ( 28.09687500061451360, -3.027376345333614438, 5.243569643749998122 ) ) ;
#5835 = CARTESIAN_POINT ( 'NONE',  ( 9.525000000000002132, 6.123233995736764310E-16, -4.999999999999998224 ) ) ;
#5836 = CARTESIAN_POINT ( 'NONE',  ( 3.999999999999998668, 14.52500000122903323, 27.69059892324149175 ) ) ;
#5837 = CARTESIAN_POINT ( 'NONE',  ( 9.150000001229033231, -2.886751345948125991, -5.000000000000000000 ) ) ;
#5838 = CARTESIAN_POINT ( 'NONE',  ( 18.79687500061451644, -3.027376345333610441, -5.243569643749999898 ) ) ;
#5839 = CARTESIAN_POINT ( 'NONE',  ( 13.62187500061451750, 3.027376345333611329, 5.243569643749999010 ) ) ;
#5840 = LINE ( 'NONE', #23545, #18282 ) ;
#5841 = ORIENTED_EDGE ( 'NONE', *, *, #59933, .T. ) ;
#5842 = CARTESIAN_POINT ( 'NONE',  ( 15.77812500061451573, 4.541064518000418104, 2.621784821874999949 ) ) ;
#5843 = CARTESIAN_POINT ( 'NONE',  ( 27.07500000122903216, -5.773502691896255534, -1.060575238724906372E-15 ) ) ;
#5844 = CARTESIAN_POINT ( 'NONE',  ( 15.49687500061451750, -3.027376345333614438, 5.243569643749998122 ) ) ;
#5845 = CARTESIAN_POINT ( 'NONE',  ( 3.975671559181608306, 9.180671356215658108, -34.51033026775080970 ) ) ;
#5846 = CARTESIAN_POINT ( 'NONE',  ( 17.50312500061451715, 4.541064518000418104, -2.621784821874998173 ) ) ;
#5847 = CARTESIAN_POINT ( 'NONE',  ( 45.00000000000000000, 0.000000000000000000, 4.999999999999998224 ) ) ;
#5848 = EDGE_CURVE ( 'NONE', #48096, #14158, #58125, .T. ) ;
#5849 = CARTESIAN_POINT ( 'NONE',  ( 27.34687500061451360, -3.027376345333610441, -5.243569643749999898 ) ) ;
#5850 = CARTESIAN_POINT ( 'NONE',  ( -4.243569643749997233, 11.29062500061451857, 32.45002607614398471 ) ) ;
#5851 = CARTESIAN_POINT ( 'NONE',  ( 15.04687500061451644, -3.027376345333614438, 5.243569643749998122 ) ) ;
#5852 = CARTESIAN_POINT ( 'NONE',  ( 13.08750000122903323, -4.330127018922194537, 2.499999999999995559 ) ) ;
#5853 = FACE_OUTER_BOUND ( 'NONE', #21261, .T. ) ;
#5854 = CARTESIAN_POINT ( 'NONE',  ( -2.121784821874996840, 18.58437500061451786, -26.32496088578401583 ) ) ;
#5855 = CARTESIAN_POINT ( 'NONE',  ( 18.08437500061451431, 4.541064518000418104, 2.621784821874999949 ) ) ;
#5856 = CARTESIAN_POINT ( 'NONE',  ( 19.50000000122903288, -2.886751345948125991, -5.000000000000000000 ) ) ;
#5857 = CARTESIAN_POINT ( 'NONE',  ( 15.53437500061451715, -4.541064518000419881, 2.621784821874995952 ) ) ;
#5858 = CARTESIAN_POINT ( 'NONE',  ( -2.121784821874996840, 12.28437500061451892, 33.67503911421598417 ) ) ;
#5859 = CARTESIAN_POINT ( 'NONE',  ( 21.63750000122903572, -4.330127018922194537, 2.499999999999995559 ) ) ;
#5860 = CARTESIAN_POINT ( 'NONE',  ( 15.32812500061451644, 4.541064518000418104, 2.621784821874999949 ) ) ;
#5861 = CARTESIAN_POINT ( 'NONE',  ( 29.01562500061451644, -6.054752690667223547, -1.112240025338166033E-15 ) ) ;
#5862 = EDGE_LOOP ( 'NONE', ( #33158, #41003, #23443, #42652 ) ) ;
#5863 = ORIENTED_EDGE ( 'NONE', *, *, #61233, .T. ) ;
#5864 = CARTESIAN_POINT ( 'NONE',  ( 20.85000000000000142, 4.330127018922192761, -2.499999999999997780 ) ) ;
#5865 = CYLINDRICAL_SURFACE ( 'NONE', #55222, 4.999999999999998224 ) ;
#5866 = CARTESIAN_POINT ( 'NONE',  ( 3.965625000614515727, 3.027376345333613106, -5.243569643749998122 ) ) ;
#5867 = CARTESIAN_POINT ( 'NONE',  ( 15.18750000122903465, 4.330127018922191873, 2.499999999999999556 ) ) ;
#5868 = CARTESIAN_POINT ( 'NONE',  ( 19.86562500061451786, 3.027376345333611329, 5.243569643749999010 ) ) ;
#5869 = EDGE_CURVE ( 'NONE', #10555, #8125, #41127, .T. ) ;
#5870 = CARTESIAN_POINT ( 'NONE',  ( 25.45312500061451644, -4.541064518000417216, -2.621784821875001281 ) ) ;
#5871 = CARTESIAN_POINT ( 'NONE',  ( 6.815625000614517148, 3.027376345333611329, 5.243569643749999010 ) ) ;
#5872 = CARTESIAN_POINT ( 'NONE',  ( 1.626862140677534273E-15, 14.26250000000000107, 34.00000000000000000 ) ) ;
#5873 = CARTESIAN_POINT ( 'NONE',  ( 30.00000000000000000, 0.000000000000000000, 4.999999999999998224 ) ) ;
#5874 = CARTESIAN_POINT ( 'NONE',  ( 10.13437500061451679, -4.119189519843968306, 2.378215178124996054 ) ) ;
#5875 = CARTESIAN_POINT ( 'NONE',  ( 11.21250000122903501, 0.000000000000000000, 4.999999999999998224 ) ) ;
#5876 = CARTESIAN_POINT ( 'NONE',  ( 3.999999999999998668, 12.27500000122903501, -32.30940107675850470 ) ) ;
#5877 = CARTESIAN_POINT ( 'NONE',  ( -4.243569643749997233, 18.54687500061451289, -27.54997392385601174 ) ) ;
#5878 = EDGE_CURVE ( 'NONE', #51815, #71973, #18010, .T. ) ;
#5879 = CARTESIAN_POINT ( 'NONE',  ( 6.300000001229033586, -2.886751345948129988, 4.999999999999997335 ) ) ;
#5880 = CARTESIAN_POINT ( 'NONE',  ( 8.625000000000000000, 6.123233995736764310E-16, -4.999999999999998224 ) ) ;
#5881 =( BOUNDED_CURVE ( )  B_SPLINE_CURVE ( 2, ( #34955, #51596, #63745, #996, #1353, #13134, #7967 ),
 .UNSPECIFIED., .F., .F. ) 
 B_SPLINE_CURVE_WITH_KNOTS ( ( 3, 2, 2, 3 ),
 ( 0.4600000000000000200, 0.4633333333333333748, 0.4666666666666667851, 0.4700000000000001399 ),
 .UNSPECIFIED. ) 
 CURVE ( )  GEOMETRIC_REPRESENTATION_ITEM ( )  RATIONAL_B_SPLINE_CURVE ( ( 1.000000000000000000, 0.8660254037844387076, 1.000000000000000000, 0.8660254037844387076, 1.000000000000000000, 0.8660254037844320463, 1.000000000000006661 ) ) 
 REPRESENTATION_ITEM ( '' )  );
#5882 = CARTESIAN_POINT ( 'NONE',  ( 4.837500001229035895, 4.330127018922191873, 2.499999999999999556 ) ) ;
#5883 = CARTESIAN_POINT ( 'NONE',  ( 12.90937500061451537, -4.541064518000417216, -2.621784821875001281 ) ) ;
#5884 = B_SPLINE_CURVE_WITH_KNOTS ( 'NONE', 3,
 ( #58479, #69945, #8617, #64763, #64398, #53316, #13789, #36330, #58845, #8255 ),
 .UNSPECIFIED., .F., .F.,
 ( 4, 3, 3, 4 ),
 ( 3.346269061518779240E-14, 0.0001125120373406391218, 0.0001770538234357889697, 0.0002416132447809637063 ),
 .UNSPECIFIED. ) ;
#5885 = CARTESIAN_POINT ( 'NONE',  ( 3.553125000614516082, 4.541064518000418104, -2.621784821874998173 ) ) ;
#5886 = CARTESIAN_POINT ( 'NONE',  ( 12.97500000122903430, 2.886751345948126879, 4.999999999999998224 ) ) ;
#5887 = CARTESIAN_POINT ( 'NONE',  ( -3.999999999999999112, 19.66250000122903430, -30.00000000000000000 ) ) ;
#5888 = CARTESIAN_POINT ( 'NONE',  ( 9.534375000614517148, 4.541064518000418104, 2.621784821874999949 ) ) ;
#5889 = LINE ( 'NONE', #51320, #35918 ) ;
#5890 = CARTESIAN_POINT ( 'NONE',  ( 19.65000000000000213, 0.000000000000000000, 4.999999999999998224 ) ) ;
#5891 = CARTESIAN_POINT ( 'NONE',  ( 2.121784821874999061, 17.85312500061459673, 26.32496088578401583 ) ) ;
#5892 = CARTESIAN_POINT ( 'NONE',  ( 21.49687500061451573, -3.027376345333610441, -5.243569643749999898 ) ) ;
#5893 = CARTESIAN_POINT ( 'NONE',  ( 28.68750000122903288, 4.330127018922191873, 2.499999999999999556 ) ) ;
#5894 = CARTESIAN_POINT ( 'NONE',  ( 17.93437500061451573, 5.492252693125287522, 3.363034840372157021E-16 ) ) ;
#5895 = CARTESIAN_POINT ( 'NONE',  ( 22.00312500061451360, 4.541064518000418104, -2.621784821874998173 ) ) ;
#5896 = CARTESIAN_POINT ( 'NONE',  ( 16.00312500061451715, -4.541064518000417216, -2.621784821875001281 ) ) ;
#5897 = CARTESIAN_POINT ( 'NONE',  ( 25.88437500061451857, -2.746126346562642428, -4.756430356249999214 ) ) ;
#5898 = CARTESIAN_POINT ( 'NONE',  ( 11.97187500061451892, -6.054752690667223547, -1.112240025338166033E-15 ) ) ;
#5899 = CARTESIAN_POINT ( 'NONE',  ( 29.69999999999999574, -4.330127018922190985, -2.500000000000001332 ) ) ;
#5900 = CARTESIAN_POINT ( 'NONE',  ( 25.91250000122903074, 4.330127018922192761, -2.499999999999997780 ) ) ;
#5901 = CARTESIAN_POINT ( 'NONE',  ( 3.234375000614516438, 4.541064518000418104, 2.621784821874999949 ) ) ;
#5902 = CARTESIAN_POINT ( 'NONE',  ( 14.10937500061451644, 0.000000000000000000, 5.243569643749999010 ) ) ;
#5903 = CARTESIAN_POINT ( 'NONE',  ( 28.50937500061451502, 0.000000000000000000, 5.243569643749999010 ) ) ;
#5904 = CARTESIAN_POINT ( 'NONE',  ( 3.075000000000001510, -4.330127018922194537, 2.499999999999995559 ) ) ;
#5905 = CYLINDRICAL_SURFACE ( 'NONE', #14771, 4.999999999999998224 ) ;
#5906 = CARTESIAN_POINT ( 'NONE',  ( 22.05937500061451573, 4.541064518000418104, -2.621784821874998173 ) ) ;
#5907 = CARTESIAN_POINT ( 'NONE',  ( 14.14687500061451786, -3.027376345333614438, 5.243569643749998122 ) ) ;
#5908 = CARTESIAN_POINT ( 'NONE',  ( 3.756430356250000546, 15.49062499938548321, 27.83122392262697886 ) ) ;
#5909 = CARTESIAN_POINT ( 'NONE',  ( 25.98750000000000071, -2.886751345948129988, 4.999999999999997335 ) ) ;
#5910 = CARTESIAN_POINT ( 'NONE',  ( 3.412500001229032964, 4.330127018922192761, -2.499999999999997780 ) ) ;
#5911 = CARTESIAN_POINT ( 'NONE',  ( 28.92187500061451644, 2.746126346562643317, 4.756430356249998326 ) ) ;
#5912 = CARTESIAN_POINT ( 'NONE',  ( 18.14062500061451644, -3.027376345333614438, 5.243569643749998122 ) ) ;
#5913 = CARTESIAN_POINT ( 'NONE',  ( 6.412500000000001421, 2.886751345948129099, -4.999999999999998224 ) ) ;
#5914 = CARTESIAN_POINT ( 'NONE',  ( -1.071796769724488563, 14.24240381056766758, 34.00000000000000000 ) ) ;
#5915 = CARTESIAN_POINT ( 'NONE',  ( 16.91250000000000142, 2.886751345948126879, 4.999999999999999112 ) ) ;
#5916 = CARTESIAN_POINT ( 'NONE',  ( -4.243569643749999898, 13.01562500061451999, 27.54997392385601529 ) ) ;
#5917 = LINE ( 'NONE', #11464, #17138 ) ;
#5918 = CARTESIAN_POINT ( 'NONE',  ( 21.37500000122902932, 2.886751345948129099, -4.999999999999998224 ) ) ;
#5919 = CARTESIAN_POINT ( 'NONE',  ( 4.520916466877475948, 8.924797207603107907, 26.03637063158135234 ) ) ;
#5920 = CARTESIAN_POINT ( 'NONE',  ( 26.33437500061451431, -4.541064518000419881, 2.621784821874995952 ) ) ;
#5921 = ORIENTED_EDGE ( 'NONE', *, *, #54530, .F. ) ;
#5922 = CARTESIAN_POINT ( 'NONE',  ( 21.47812500061451502, 6.421520780324663323E-16, -5.243569643749999010 ) ) ;
#5923 = CARTESIAN_POINT ( 'NONE',  ( 21.64687500061451786, 6.054752690667223547, 3.707466751127219781E-16 ) ) ;
#5924 = CARTESIAN_POINT ( 'NONE',  ( 5.437500000000001776, -2.886751345948125991, -5.000000000000000000 ) ) ;
#5925 = CARTESIAN_POINT ( 'NONE',  ( 9.965625000614517504, 3.027376345333611329, 5.243569643749999010 ) ) ;
#5926 = CARTESIAN_POINT ( 'NONE',  ( 23.80312500061451786, 4.541064518000418104, -2.621784821874998173 ) ) ;
#5927 = CARTESIAN_POINT ( 'NONE',  ( 12.79687500061451821, -3.027376345333614438, 5.243569643749998122 ) ) ;
#5928 = CARTESIAN_POINT ( 'NONE',  ( 16.50937500061451502, -4.541064518000417216, -2.621784821875001281 ) ) ;
#5929 = CARTESIAN_POINT ( 'NONE',  ( 4.458087853507603171, 2.264012079524543974, -4.729647261352303289 ) ) ;
#5930 = CARTESIAN_POINT ( 'NONE',  ( -4.243569643749999898, 17.96562500061451573, 27.54997392385601529 ) ) ;
#5931 = CARTESIAN_POINT ( 'NONE',  ( 22.57500000122903572, -5.773502691896255534, -1.060575238724906372E-15 ) ) ;
#5932 = CARTESIAN_POINT ( 'NONE',  ( 13.65937500061451715, 0.000000000000000000, 4.756430356249998326 ) ) ;
#5933 = CARTESIAN_POINT ( 'NONE',  ( 11.87812500061451537, -4.541064518000419881, 2.621784821874995952 ) ) ;
#5934 = CARTESIAN_POINT ( 'NONE',  ( 5.109375000614518214, 0.000000000000000000, 5.243569643749999010 ) ) ;
#5935 = CARTESIAN_POINT ( 'NONE',  ( 4.996875000614516615, 6.054752690667223547, 3.707466751127219781E-16 ) ) ;
#5936 = VERTEX_POINT ( 'NONE', #64510 ) ;
#5937 = CARTESIAN_POINT ( 'NONE',  ( 25.09687500061451715, -3.027376345333610441, -5.243569643749999898 ) ) ;
#5938 = CARTESIAN_POINT ( 'NONE',  ( 17.65312500061451573, 0.000000000000000000, 5.243569643749999010 ) ) ;
#5939 = CARTESIAN_POINT ( 'NONE',  ( 27.00000000122903288, -2.886751345948129988, 4.999999999999997335 ) ) ;
#5940 =( BOUNDED_CURVE ( )  B_SPLINE_CURVE ( 2, ( #71584, #14683, #9156, #9523, #14325, #26145, #48322 ),
 .UNSPECIFIED., .F., .F. ) 
 B_SPLINE_CURVE_WITH_KNOTS ( ( 3, 2, 2, 3 ),
 ( 0.9000000000000000222, 0.9033333333333333215, 0.9066666666666666208, 0.9100000000000000311 ),
 .UNSPECIFIED. ) 
 CURVE ( )  GEOMETRIC_REPRESENTATION_ITEM ( )  RATIONAL_B_SPLINE_CURVE ( ( 1.000000000000000000, 0.8660254037844387076, 1.000000000000000000, 0.8660254037844387076, 1.000000000000000000, 0.8660254037844387076, 1.000000000000000000 ) ) 
 REPRESENTATION_ITEM ( '' )  );
#5941 = CARTESIAN_POINT ( 'NONE',  ( 26.99062500061451431, 6.054752690667223547, 3.707466751127219781E-16 ) ) ;
#5942 = CARTESIAN_POINT ( 'NONE',  ( 22.39687500061451075, -3.027376345333610441, -5.243569643749999898 ) ) ;
#5943 = CARTESIAN_POINT ( 'NONE',  ( 16.45312500061451289, -4.541064518000417216, -2.621784821875001281 ) ) ;
#5944 = CARTESIAN_POINT ( 'NONE',  ( -2.000000000000000000, 10.02500000000000036, 26.53589838486224650 ) ) ;
#5945 = CARTESIAN_POINT ( 'NONE',  ( 23.46562500061451573, 3.027376345333611329, 5.243569643749999010 ) ) ;
#5946 = CARTESIAN_POINT ( 'NONE',  ( 3.937500001229034208, 4.330127018922191873, 2.499999999999999556 ) ) ;
#5947 = ORIENTED_EDGE ( 'NONE', *, *, #19674, .F. ) ;
#5948 = CARTESIAN_POINT ( 'NONE',  ( 28.72500000000000142, -4.330127018922194537, 2.499999999999995559 ) ) ;
#5949 = CARTESIAN_POINT ( 'NONE',  ( -2.828200636599751609E-16, 12.68750000000000000, -34.61880215351700230 ) ) ;
#5950 = CARTESIAN_POINT ( 'NONE',  ( -1.878215178124999163, 16.95312499938548356, 26.74683588394047007 ) ) ;
#5951 = CARTESIAN_POINT ( 'NONE',  ( 28.56562500061451715, -6.054752690667223547, -1.112240025338166033E-15 ) ) ;
#5952 = EDGE_CURVE ( 'NONE', #19210, #33154, #20825, .T. ) ;
#5953 = CARTESIAN_POINT ( 'NONE',  ( 10.37812500061451715, 4.541064518000418104, 2.621784821874999949 ) ) ;
#5954 = CARTESIAN_POINT ( 'NONE',  ( 21.37500000122902932, 2.886751345948129099, -4.999999999999998224 ) ) ;
#5955 = CARTESIAN_POINT ( 'NONE',  ( 13.24687500061451750, -3.027376345333614438, 5.243569643749998122 ) ) ;
#5956 = CARTESIAN_POINT ( 'NONE',  ( 27.62812500061451360, -4.541064518000419881, 2.621784821874995952 ) ) ;
#5957 = CARTESIAN_POINT ( 'NONE',  ( 28.87499999999999645, 6.123233995736764310E-16, -4.999999999999998224 ) ) ;
#5958 = CARTESIAN_POINT ( 'NONE',  ( -2.828200636599751609E-16, 19.10000000122903074, -34.61880215351700230 ) ) ;
#5959 = CARTESIAN_POINT ( 'NONE',  ( 14.66250000122903252, 4.330127018922192761, -2.499999999999997780 ) ) ;
#5960 = CARTESIAN_POINT ( 'NONE',  ( 12.36562500061451608, -6.054752690667223547, -1.112240025338166033E-15 ) ) ;
#5961 = VERTEX_POINT ( 'NONE', #47527 ) ;
#5962 = CARTESIAN_POINT ( 'NONE',  ( 9.403125000614517504, 4.541064518000418104, -2.621784821874998173 ) ) ;
#5963 = CARTESIAN_POINT ( 'NONE',  ( 6.628125000614517148, 6.421520780324663323E-16, -5.243569643749999010 ) ) ;
#5964 = CARTESIAN_POINT ( 'NONE',  ( 19.35937500061451644, 4.119189519843966529, -2.378215178124998275 ) ) ;
#5965 = DIRECTION ( 'NONE',  ( 0.000000000000000000, 0.000000000000000000, 1.000000000000000000 ) ) ;
#5966 = ADVANCED_FACE ( 'NONE', ( #53435 ), #13903, .F. ) ;
#5967 = CARTESIAN_POINT ( 'NONE',  ( 15.59999999999999964, 0.000000000000000000, 4.999999999999998224 ) ) ;
#5968 = EDGE_CURVE ( 'NONE', #60873, #17509, #26830, .T. ) ;
#5969 = CARTESIAN_POINT ( 'NONE',  ( 17.14687500061451786, 6.054752690667223547, 3.707466751127219781E-16 ) ) ;
#5970 = CARTESIAN_POINT ( 'NONE',  ( 11.43750000122903465, 6.123233995736764310E-16, -4.999999999999998224 ) ) ;
#5971 = CARTESIAN_POINT ( 'NONE',  ( 18.64687500061451786, -3.027376345333614438, 5.243569643749998122 ) ) ;
#5972 = CARTESIAN_POINT ( 'NONE',  ( 18.75000000000000000, 0.000000000000000000, 4.999999999999998224 ) ) ;
#5973 = EDGE_CURVE ( 'NONE', #18820, #37430, #4305, .T. ) ;
#5974 = CARTESIAN_POINT ( 'NONE',  ( 20.78437500061451715, 4.541064518000418104, 2.621784821874999949 ) ) ;
#5975 = CARTESIAN_POINT ( 'NONE',  ( 4.243569643749999898, 14.62812500061451715, -30.00000000000000000 ) ) ;
#5976 = CARTESIAN_POINT ( 'NONE',  ( -4.243569643749999898, 19.80312500061451786, 30.00000000000000000 ) ) ;
#5977 = CARTESIAN_POINT ( 'NONE',  ( 25.95937500061451431, 2.746126346562645981, -4.756430356249997438 ) ) ;
#5978 = CARTESIAN_POINT ( 'NONE',  ( 4.116754692841747776, 2.837675796283581686, 4.409386438731211832 ) ) ;
#5979 = CARTESIAN_POINT ( 'NONE',  ( 27.29062500061451502, -3.027376345333610441, -5.243569643749999898 ) ) ;
#5980 = CARTESIAN_POINT ( 'NONE',  ( 5.212500001229032343, 4.330127018922192761, -2.499999999999997780 ) ) ;
#5981 = CARTESIAN_POINT ( 'NONE',  ( 28.65937500061451715, -4.541064518000417216, -2.621784821875001281 ) ) ;
#5982 = CARTESIAN_POINT ( 'NONE',  ( 24.97499999999999787, 4.330127018922191873, 2.499999999999999556 ) ) ;
#5983 = CARTESIAN_POINT ( 'NONE',  ( 8.353125000614518569, -4.541064518000417216, -2.621784821875001281 ) ) ;
#5984 = CARTESIAN_POINT ( 'NONE',  ( 24.04687500061451289, -4.119189519843965641, -2.378215178125001383 ) ) ;
#5985 = CARTESIAN_POINT ( 'NONE',  ( 19.99687500061451573, -3.027376345333614438, 5.243569643749998122 ) ) ;
#5986 = CARTESIAN_POINT ( 'NONE',  ( 11.48437500061451644, -2.746126346562641984, -4.756430356249999214 ) ) ;
#5987 = CARTESIAN_POINT ( 'NONE',  ( 6.140625000614516438, -3.027376345333610441, -5.243569643749999898 ) ) ;
#5988 = CARTESIAN_POINT ( 'NONE',  ( 11.82187500061451679, 3.027376345333611329, 5.243569643749999010 ) ) ;
#5989 = EDGE_LOOP ( 'NONE', ( #26647, #40947, #41103, #17915 ) ) ;
#5990 = CARTESIAN_POINT ( 'NONE',  ( 21.94687500061451857, -3.027376345333610441, -5.243569643749999898 ) ) ;
#5991 = CARTESIAN_POINT ( 'NONE',  ( 45.00000000000000000, 0.000000000000000000, 0.000000000000000000 ) ) ;
#5992 = CARTESIAN_POINT ( 'NONE',  ( 28.27499999999999858, -4.330127018922194537, 2.499999999999995559 ) ) ;
#5993 = CARTESIAN_POINT ( 'NONE',  ( 3.412500000000002309, 2.886751345948126879, 4.999999999999999112 ) ) ;
#5994 = CARTESIAN_POINT ( 'NONE',  ( 14.43750000122903288, -4.330127018922194537, 2.499999999999995559 ) ) ;
#5995 = CARTESIAN_POINT ( 'NONE',  ( 4.000000000000000000, 12.20000000122903394, 32.30940107675849760 ) ) ;
#5996 = CARTESIAN_POINT ( 'NONE',  ( 14.43750000122903288, -4.330127018922194537, 2.499999999999995559 ) ) ;
#5997 = EDGE_LOOP ( 'NONE', ( #61702, #13702, #39988, #34006 ) ) ;
#5998 = CARTESIAN_POINT ( 'NONE',  ( 13.61250000000000071, 2.886751345948129099, -4.999999999999998224 ) ) ;
#5999 = CARTESIAN_POINT ( 'NONE',  ( 24.10312500061451502, -4.541064518000417216, -2.621784821875001281 ) ) ;
#6000 = CARTESIAN_POINT ( 'NONE',  ( 14.10000000000000142, 4.330127018922192761, -2.499999999999997780 ) ) ;
#6001 = CARTESIAN_POINT ( 'NONE',  ( 11.40000000122903501, -2.886751345948125991, -5.000000000000000000 ) ) ;
#6002 = CARTESIAN_POINT ( 'NONE',  ( 9.590625000614517504, -3.027376345333614438, 5.243569643749998122 ) ) ;
#6003 = CARTESIAN_POINT ( 'NONE',  ( 9.000000000000001776, -4.330127018922190985, -2.500000000000001332 ) ) ;
#6004 = CARTESIAN_POINT ( 'NONE',  ( 9.001249775931846008E-16, 14.57187500061451679, -25.09994784771203058 ) ) ;
#6005 = CARTESIAN_POINT ( 'NONE',  ( 27.75000000122903288, 5.773502691896255534, 3.535250795749688894E-16 ) ) ;
#6006 = CARTESIAN_POINT ( 'NONE',  ( 3.756430356250000102, 16.69062499938548427, 30.00000000000000000 ) ) ;
#6007 = CARTESIAN_POINT ( 'NONE',  ( 8.587500000000002132, -2.886751345948125991, -5.000000000000000000 ) ) ;
#6008 = CARTESIAN_POINT ( 'NONE',  ( -2.000000000000000000, 13.17500000000000071, -33.46410161513775705 ) ) ;
#6009 = ORIENTED_EDGE ( 'NONE', *, *, #59897, .T. ) ;
#6010 = CARTESIAN_POINT ( 'NONE',  ( 20.76562500061451644, 3.027376345333611329, 5.243569643749999010 ) ) ;
#6011 = CARTESIAN_POINT ( 'NONE',  ( 14.62500000122903288, 2.886751345948129099, -4.999999999999998224 ) ) ;
#6012 = CARTESIAN_POINT ( 'NONE',  ( 28.97812500061451502, -4.541064518000419881, 2.621784821874995952 ) ) ;
#6013 = CARTESIAN_POINT ( 'NONE',  ( 29.63437500061451502, 6.421520780324663323E-16, -5.243569643749999010 ) ) ;
#6014 = CARTESIAN_POINT ( 'NONE',  ( 19.39687500061451786, 6.054752690667223547, 3.707466751127219781E-16 ) ) ;
#6015 = CARTESIAN_POINT ( 'NONE',  ( 16.90312500061451573, -4.541064518000417216, -2.621784821875001281 ) ) ;
#6016 = CARTESIAN_POINT ( 'NONE',  ( 4.243569643749999898, 11.02812500061459389, -30.00000000000000000 ) ) ;
#6017 = CARTESIAN_POINT ( 'NONE',  ( 5.840625000614516615, 6.054752690667223547, 3.707466751127219781E-16 ) ) ;
#6018 = CARTESIAN_POINT ( 'NONE',  ( 29.13750000122903216, 4.330127018922191873, 2.499999999999999556 ) ) ;
#6019 = CARTESIAN_POINT ( 'NONE',  ( 22.77187500061451786, -5.492252693125287522, -1.008910452111647106E-15 ) ) ;
#6020 = CARTESIAN_POINT ( 'NONE',  ( 19.45312500061451644, 0.000000000000000000, 5.243569643749999010 ) ) ;
#6021 = CARTESIAN_POINT ( 'NONE',  ( 13.50000000000000178, -4.330127018922190985, -2.500000000000001332 ) ) ;
#6022 = CARTESIAN_POINT ( 'NONE',  ( 4.050000001229035362, -2.886751345948129988, 4.999999999999997335 ) ) ;
#6023 = CARTESIAN_POINT ( 'NONE',  ( 12.64687500061451608, 6.054752690667223547, 3.707466751127219781E-16 ) ) ;
#6024 = AXIS2_PLACEMENT_3D ( 'NONE', #59768, #32074, #19878 ) ;
#6025 = CARTESIAN_POINT ( 'NONE',  ( 12.34687500061452070, -3.027376345333614438, 5.243569643749998122 ) ) ;
#6026 = CARTESIAN_POINT ( 'NONE',  ( 20.25937500061451857, 4.541064518000418104, -2.621784821874998173 ) ) ;
#6027 = EDGE_LOOP ( 'NONE', ( #68075, #43354, #44679, #36902 ) ) ;
#6028 = CARTESIAN_POINT ( 'NONE',  ( 30.00000000000000000, 6.123233995736764310E-16, -4.999999999999998224 ) ) ;
#6029 = CARTESIAN_POINT ( 'NONE',  ( 23.09062500061451573, -3.027376345333614438, 5.243569643749998122 ) ) ;
#6030 = CARTESIAN_POINT ( 'NONE',  ( 19.17187500061451999, -6.054752690667223547, -1.112240025338166033E-15 ) ) ;
#6031 = CARTESIAN_POINT ( 'NONE',  ( 23.50312500061451360, 0.000000000000000000, 5.243569643749999010 ) ) ;
#6032 = CARTESIAN_POINT ( 'NONE',  ( 45.00000000000000000, 0.000000000000000000, 4.999999999999998224 ) ) ;
#6033 = CARTESIAN_POINT ( 'NONE',  ( 2.000000000000001332, 16.55000000000000071, 33.46410161513774995 ) ) ;
#6034 = CARTESIAN_POINT ( 'NONE',  ( 4.171875000614517326, 3.027376345333611329, 5.243569643749999010 ) ) ;
#6035 = CARTESIAN_POINT ( 'NONE',  ( 12.60000000122903430, -2.886751345948129988, 4.999999999999997335 ) ) ;
#6036 = CARTESIAN_POINT ( 'NONE',  ( 6.975000001229032520, 2.886751345948129099, -4.999999999999998224 ) ) ;
#6037 = CARTESIAN_POINT ( 'NONE',  ( 27.67500000122903359, 2.886751345948129099, -4.999999999999998224 ) ) ;
#6038 = CARTESIAN_POINT ( 'NONE',  ( 2.828200636599751609E-16, 17.50624999877096499, 25.38119784648299415 ) ) ;
#6039 = CARTESIAN_POINT ( 'NONE',  ( 17.26875000122903003, 2.886751345948129099, -4.999999999999998224 ) ) ;
#6040 = CARTESIAN_POINT ( 'NONE',  ( 13.09687500061451892, 6.054752690667223547, 3.707466751127219781E-16 ) ) ;
#6041 = CARTESIAN_POINT ( 'NONE',  ( -5.810221930991193690E-16, 14.93750000000000000, -34.00000000000000000 ) ) ;
#6042 = CARTESIAN_POINT ( 'NONE',  ( 16.49062500061451786, -3.027376345333610441, -5.243569643749999898 ) ) ;
#6043 = CARTESIAN_POINT ( 'NONE',  ( 14.55937500061451573, 0.000000000000000000, 5.243569643749999010 ) ) ;
#6044 = CARTESIAN_POINT ( 'NONE',  ( 3.740625000614516527, -3.027376345333614438, 5.243569643749998122 ) ) ;
#6045 = CARTESIAN_POINT ( 'NONE',  ( 20.40937500061451715, 0.000000000000000000, 5.243569643749999010 ) ) ;
#6046 = CARTESIAN_POINT ( 'NONE',  ( 8.671875000614518214, 3.027376345333611329, 5.243569643749999010 ) ) ;
#6047 = CARTESIAN_POINT ( 'NONE',  ( 15.03750000122903252, 6.123233995736764310E-16, -4.999999999999998224 ) ) ;
#6048 = CARTESIAN_POINT ( 'NONE',  ( 5.775000000000002132, -4.330127018922194537, 2.499999999999995559 ) ) ;
#6049 = CARTESIAN_POINT ( 'NONE',  ( 5.587500001229033231, 6.123233995736764310E-16, -4.999999999999998224 ) ) ;
#6050 = CARTESIAN_POINT ( 'NONE',  ( 19.37812500061451715, 4.541064518000418104, 2.621784821874999949 ) ) ;
#6051 = CARTESIAN_POINT ( 'NONE',  ( 8.850000001229034297, 5.773502691896255534, 3.535250795749688894E-16 ) ) ;
#6052 = CARTESIAN_POINT ( 'NONE',  ( 17.09062500061451573, 6.054752690667223547, 3.707466751127219781E-16 ) ) ;
#6053 = CARTESIAN_POINT ( 'NONE',  ( 12.40312500061451573, -4.541064518000417216, -2.621784821875001281 ) ) ;
#6054 = CARTESIAN_POINT ( 'NONE',  ( 26.63437500061451857, 4.119189519843966529, 2.378215178124999607 ) ) ;
#6055 = CARTESIAN_POINT ( 'NONE',  ( 13.38750000000000107, -2.886751345948129988, 4.999999999999997335 ) ) ;
#6056 = PRESENTATION_LAYER_ASSIGNMENT (  '', '', ( #37895 ) ) ;
#6057 = CARTESIAN_POINT ( 'NONE',  ( 9.937500001229032875, -4.330127018922194537, 2.499999999999995559 ) ) ;
#6058 = CARTESIAN_POINT ( 'NONE',  ( 6.178125000614518747, 6.421520780324663323E-16, -5.243569643749999010 ) ) ;
#6059 = EDGE_CURVE ( 'NONE', #40707, #23277, #57498, .T. ) ;
#6060 = CARTESIAN_POINT ( 'NONE',  ( 19.27500000122903145, 2.886751345948126879, 4.999999999999999112 ) ) ;
#6061 = CARTESIAN_POINT ( 'NONE',  ( 27.63749999999999929, 5.773502691896255534, 3.535250795749688894E-16 ) ) ;
#6062 = CARTESIAN_POINT ( 'NONE',  ( 4.243569643749999898, 11.04687500061451999, -27.54997392385601529 ) ) ;
#6063 = DIRECTION ( 'NONE',  ( -0.000000000000000000, -1.000000000000000000, -0.000000000000000000 ) ) ;
#6064 = CYLINDRICAL_SURFACE ( 'NONE', #19381, 4.999999999999998224 ) ;
#6065 = LINE ( 'NONE', #50774, #72936 ) ;
#6066 = CARTESIAN_POINT ( 'NONE',  ( 20.29687500061451644, 6.054752690667223547, 3.707466751127219781E-16 ) ) ;
#6067 = AXIS2_PLACEMENT_3D ( 'NONE', #3586, #65256, #37920 ) ;
#6068 = CARTESIAN_POINT ( 'NONE',  ( 15.33750000000000036, -2.886751345948126435, -5.000000000000000000 ) ) ;
#6069 = CARTESIAN_POINT ( 'NONE',  ( 17.09062500061451573, 6.054752690667223547, 3.707466751127219781E-16 ) ) ;
#6070 = CARTESIAN_POINT ( 'NONE',  ( 12.20625000122903181, -4.330127018922190985, -2.500000000000001332 ) ) ;
#6071 = CARTESIAN_POINT ( 'NONE',  ( 10.87500000000000000, 6.123233995736764310E-16, -4.999999999999998224 ) ) ;
#6072 = DIRECTION ( 'NONE',  ( -1.000000000000000000, 0.000000000000000000, 0.000000000000000000 ) ) ;
#6073 = CARTESIAN_POINT ( 'NONE',  ( 26.89687500061451431, -3.027376345333610441, -5.243569643749999898 ) ) ;
#6074 = CARTESIAN_POINT ( 'NONE',  ( 19.47187500061451360, -4.119189519843968306, 2.378215178124996054 ) ) ;
#6075 = CARTESIAN_POINT ( 'NONE',  ( 11.27812500061451573, 4.541064518000418104, 2.621784821874999949 ) ) ;
#6076 = CARTESIAN_POINT ( 'NONE',  ( 10.05937500061451750, 0.000000000000000000, 5.243569643749999010 ) ) ;
#6077 = VERTEX_POINT ( 'NONE', #4663 ) ;
#6078 = CARTESIAN_POINT ( 'NONE',  ( -3.999999999999997335, 14.18750000000000000, -27.69059892324149530 ) ) ;
#6079 = CARTESIAN_POINT ( 'NONE',  ( 20.61562500061451431, 3.027376345333613106, -5.243569643749998122 ) ) ;
#6080 = CARTESIAN_POINT ( 'NONE',  ( 17.62500000122903288, -5.773502691896255534, -1.060575238724906372E-15 ) ) ;
#6081 = CARTESIAN_POINT ( 'NONE',  ( 4.000000000000000000, 15.35000000122903252, -27.69059892324149885 ) ) ;
#6082 = CARTESIAN_POINT ( 'NONE',  ( 12.75000000000000178, 4.330127018922192761, -2.499999999999997780 ) ) ;
#6083 = CARTESIAN_POINT ( 'NONE',  ( 22.80000000122903359, 5.773502691896255534, 3.535250795749688894E-16 ) ) ;
#6084 = CARTESIAN_POINT ( 'NONE',  ( 15.44062500061451537, -3.027376345333614438, 5.243569643749998122 ) ) ;
#6085 = CARTESIAN_POINT ( 'NONE',  ( 13.54687500061451466, 0.000000000000000000, 4.756430356249998326 ) ) ;
#6086 = VERTEX_POINT ( 'NONE', #44917 ) ;
#6087 = CARTESIAN_POINT ( 'NONE',  ( 20.06250000000000000, 2.886751345948126879, 4.999999999999999112 ) ) ;
#6088 =( BOUNDED_CURVE ( )  B_SPLINE_CURVE ( 2, ( #69625, #58880, #52270, #1672, #69268, #19352, #52991 ),
 .UNSPECIFIED., .F., .F. ) 
 B_SPLINE_CURVE_WITH_KNOTS ( ( 3, 2, 2, 3 ),
 ( 0.1250000000000000000, 0.1277777777777777679, 0.1305555555555555358, 0.1333333333333333037 ),
 .UNSPECIFIED. ) 
 CURVE ( )  GEOMETRIC_REPRESENTATION_ITEM ( )  RATIONAL_B_SPLINE_CURVE ( ( 1.000000000000000000, 0.8660254037844387076, 1.000000000000000000, 0.8660254037844387076, 1.000000000000000000, 0.8660254037844400399, 0.9999999999999986677 ) ) 
 REPRESENTATION_ITEM ( '' )  );
#6089 = CARTESIAN_POINT ( 'NONE',  ( 23.51249999999999574, 2.886751345948129099, -4.999999999999998224 ) ) ;
#6090 = CARTESIAN_POINT ( 'NONE',  ( 20.63437500061451857, 6.421520780324663323E-16, -5.243569643749999010 ) ) ;
#6091 = CARTESIAN_POINT ( 'NONE',  ( 26.09062500061451573, 6.054752690667223547, 3.707466751127219781E-16 ) ) ;
#6092 = EDGE_LOOP ( 'NONE', ( #10688, #72175, #13296, #49439 ) ) ;
#6093 = CARTESIAN_POINT ( 'NONE',  ( 30.00000000000000000, 6.123233995736764310E-16, -4.999999999999998224 ) ) ;
#6094 = CARTESIAN_POINT ( 'NONE',  ( 7.490625000614516082, -3.027376345333610441, -5.243569643749999898 ) ) ;
#6095 = CARTESIAN_POINT ( 'NONE',  ( 3.250662400336420177, 3.799104362746421604, 3.614115195980558859 ) ) ;
#6096 = CARTESIAN_POINT ( 'NONE',  ( 14.21249999999999858, 2.886751345948126879, 4.999999999999999112 ) ) ;
#6097 = CARTESIAN_POINT ( 'NONE',  ( -4.243569643749999898, 18.41562500061451857, 27.54997392385601529 ) ) ;
#6098 = CARTESIAN_POINT ( 'NONE',  ( 3.571875000614517237, 3.027376345333613106, -5.243569643749998122 ) ) ;
#6099 = CARTESIAN_POINT ( 'NONE',  ( 26.63437500061451857, 4.541064518000418104, 2.621784821874999949 ) ) ;
#6100 = EDGE_LOOP ( 'NONE', ( #46601, #21606, #13078, #18475 ) ) ;
#6101 = CARTESIAN_POINT ( 'NONE',  ( 23.01562500061451644, 3.027376345333611329, 5.243569643749999010 ) ) ;
#6102 = CARTESIAN_POINT ( 'NONE',  ( 24.38437500061451502, 4.541064518000418104, 2.621784821874999949 ) ) ;
#6103 = CARTESIAN_POINT ( 'NONE',  ( -4.243569643749999898, 19.35312500061459318, -30.00000000000000000 ) ) ;
#6104 = CARTESIAN_POINT ( 'NONE',  ( 12.33750000000000036, 5.773502691896255534, 3.535250795749688894E-16 ) ) ;
#6105 = CARTESIAN_POINT ( 'NONE',  ( 10.07812500061451644, -4.541064518000419881, 2.621784821874995952 ) ) ;
#6106 = CARTESIAN_POINT ( 'NONE',  ( 29.78437500061451715, 4.119189519843966529, 2.378215178124999607 ) ) ;
#6107 = CARTESIAN_POINT ( 'NONE',  ( 28.15312500061451573, -4.541064518000417216, -2.621784821875001281 ) ) ;
#6108 = CARTESIAN_POINT ( 'NONE',  ( 25.56562500061451715, 3.027376345333612662, -5.243569643749998122 ) ) ;
#6109 = CARTESIAN_POINT ( 'NONE',  ( -1.071796769724492338, 18.29240381056766651, 34.00000000000000000 ) ) ;
#6110 = CARTESIAN_POINT ( 'NONE',  ( 12.68437500061451573, 4.119189519843966529, 2.378215178124999607 ) ) ;
#6111 = CARTESIAN_POINT ( 'NONE',  ( 18.60937500061451644, 0.000000000000000000, 5.243569643749999010 ) ) ;
#6112 = CARTESIAN_POINT ( 'NONE',  ( 2.121784821875001281, 13.70937500061451786, 33.67503911421598417 ) ) ;
#6113 = CARTESIAN_POINT ( 'NONE',  ( 19.17187500061451999, -6.054752690667223547, -1.112240025338166033E-15 ) ) ;
#6114 = CARTESIAN_POINT ( 'NONE',  ( 28.13437500061451502, -4.541064518000419881, 2.621784821874995952 ) ) ;
#6115 = CARTESIAN_POINT ( 'NONE',  ( 2.121784821874999061, 16.55937500061451573, 26.32496088578401583 ) ) ;
#6116 = CARTESIAN_POINT ( 'NONE',  ( 9.553125000614517859, 0.000000000000000000, 5.243569643749999010 ) ) ;
#6117 = FACE_OUTER_BOUND ( 'NONE', #42006, .T. ) ;
#6118 = EDGE_CURVE ( 'NONE', #2103, #38096, #2920, .T. ) ;
#6119 = CARTESIAN_POINT ( 'NONE',  ( 4.509375000614518569, 4.541064518000418104, -2.621784821874998173 ) ) ;
#6120 = CARTESIAN_POINT ( 'NONE',  ( 11.64375000122903003, -2.886751345948130876, 4.999999999999996447 ) ) ;
#6121 = CARTESIAN_POINT ( 'NONE',  ( 8.053125000614516082, 4.541064518000418104, -2.621784821874998173 ) ) ;
#6122 = CARTESIAN_POINT ( 'NONE',  ( 12.27187500061451786, 3.027376345333611329, 5.243569643749999010 ) ) ;
#6123 = CARTESIAN_POINT ( 'NONE',  ( 20.28750000122903074, -4.330127018922194537, 2.499999999999995559 ) ) ;
#6124 = CARTESIAN_POINT ( 'NONE',  ( 5.821875000614519458, 3.027376345333613106, -5.243569643749998122 ) ) ;
#6125 = CARTESIAN_POINT ( 'NONE',  ( 10.86562500061451431, 3.027376345333611329, 5.243569643749999010 ) ) ;
#6126 = FACE_OUTER_BOUND ( 'NONE', #35513, .T. ) ;
#6127 = CARTESIAN_POINT ( 'NONE',  ( 23.38125000122903074, -4.330127018922194537, 2.499999999999995559 ) ) ;
#6128 = CARTESIAN_POINT ( 'NONE',  ( 18.15937500061451715, 0.000000000000000000, 5.243569643749999010 ) ) ;
#6129 = CARTESIAN_POINT ( 'NONE',  ( 8.962500001229033231, 0.000000000000000000, 4.999999999999998224 ) ) ;
#6130 = EDGE_LOOP ( 'NONE', ( #29125, #59504, #27177, #71562 ) ) ;
#6131 = CARTESIAN_POINT ( 'NONE',  ( 23.80312500061451786, 4.541064518000418104, -2.621784821874998173 ) ) ;
#6132 = CARTESIAN_POINT ( 'NONE',  ( 12.89062500061451821, -3.027376345333610441, -5.243569643749999898 ) ) ;
#6133 = CARTESIAN_POINT ( 'NONE',  ( 7.429687500307258219, 0.000000000000000000, 4.878215178124998275 ) ) ;
#6134 = AXIS2_PLACEMENT_3D ( 'NONE', #59617, #14926, #26017 ) ;
#6135 = CARTESIAN_POINT ( 'NONE',  ( 11.95312500061451644, -4.541064518000417216, -2.621784821875001281 ) ) ;
#6136 = CARTESIAN_POINT ( 'NONE',  ( 9.001249775931846008E-16, 10.52187500061451964, -25.09994784771203058 ) ) ;
#6137 = CARTESIAN_POINT ( 'NONE',  ( 11.88750000122903216, 6.123233995736764310E-16, -4.999999999999998224 ) ) ;
#6138 = CARTESIAN_POINT ( 'NONE',  ( 27.74062500061451431, -3.027376345333610441, -5.243569643749999898 ) ) ;
#6139 = CARTESIAN_POINT ( 'NONE',  ( 2.121784821874999061, 13.80312500061451786, -33.67503911421598417 ) ) ;
#6140 = CARTESIAN_POINT ( 'NONE',  ( 15.11250000122903359, 4.330127018922192761, -2.499999999999997780 ) ) ;
#6141 = CARTESIAN_POINT ( 'NONE',  ( 10.87500000000000000, 6.123233995736764310E-16, -4.999999999999998224 ) ) ;
#6142 = CARTESIAN_POINT ( 'NONE',  ( 20.01562500061451644, -6.054752690667223547, -1.112240025338166033E-15 ) ) ;
#6143 = CARTESIAN_POINT ( 'NONE',  ( 7.996875000614519280, -3.027376345333610441, -5.243569643749999898 ) ) ;
#6144 = EDGE_CURVE ( 'NONE', #67346, #68632, #53392, .T. ) ;
#6145 = CARTESIAN_POINT ( 'NONE',  ( 7.762500001229033053, -4.330127018922190985, -2.500000000000001332 ) ) ;
#6146 = CARTESIAN_POINT ( 'NONE',  ( 15.18750000122903465, 4.330127018922191873, 2.499999999999999556 ) ) ;
#6147 =( BOUNDED_CURVE ( )  B_SPLINE_CURVE ( 2, ( #63118, #62757, #52042, #23951, #11433, #67951, #46501 ),
 .UNSPECIFIED., .F., .F. ) 
 B_SPLINE_CURVE_WITH_KNOTS ( ( 3, 2, 2, 3 ),
 ( 0.9000000000000000222, 0.9033333333333333215, 0.9066666666666666208, 0.9100000000000000311 ),
 .UNSPECIFIED. ) 
 CURVE ( )  GEOMETRIC_REPRESENTATION_ITEM ( )  RATIONAL_B_SPLINE_CURVE ( ( 1.000000000000000000, 0.8660254037844387076, 1.000000000000000000, 0.8660254037844387076, 1.000000000000000000, 0.8660254037844387076, 1.000000000000000000 ) ) 
 REPRESENTATION_ITEM ( '' )  );
#6148 = CARTESIAN_POINT ( 'NONE',  ( 12.62812500061451537, 4.541064518000418104, 2.621784821874999949 ) ) ;
#6149 = CARTESIAN_POINT ( 'NONE',  ( 15.96562500061451573, -6.054752690667223547, -1.112240025338166033E-15 ) ) ;
#6150 = CARTESIAN_POINT ( 'NONE',  ( 25.72500000122903074, -5.773502691896255534, -1.060575238724906372E-15 ) ) ;
#6151 = CARTESIAN_POINT ( 'NONE',  ( 23.88749999999999929, -2.886751345948125991, -5.000000000000000000 ) ) ;
#6152 = CARTESIAN_POINT ( 'NONE',  ( 24.00937500061451502, 0.000000000000000000, 5.243569643749999010 ) ) ;
#6153 = CARTESIAN_POINT ( 'NONE',  ( 1.999999999999997335, 13.77500000000000036, 33.46410161513775705 ) ) ;
#6154 = CARTESIAN_POINT ( 'NONE',  ( 9.825000001229033941, 2.886751345948126879, 4.999999999999999112 ) ) ;
#6155 = CARTESIAN_POINT ( 'NONE',  ( 28.84687500061452070, 6.054752690667223547, 3.707466751127219781E-16 ) ) ;
#6156 =( BOUNDED_CURVE ( )  B_SPLINE_CURVE ( 2, ( #44086, #55529, #4923, #66989, #61425, #4199, #55891, #5280, #22266 ),
 .UNSPECIFIED., .F., .F. ) 
 B_SPLINE_CURVE_WITH_KNOTS ( ( 3, 2, 2, 2, 3 ),
 ( 0.3804347826086956763, 0.3840579710144927383, 0.3913043478260869734, 0.3985507246376811530, 0.4021739130434782705 ),
 .UNSPECIFIED. ) 
 CURVE ( )  GEOMETRIC_REPRESENTATION_ITEM ( )  RATIONAL_B_SPLINE_CURVE ( ( 0.9330127018922194093, 0.9330127018922198534, 1.000000000000000000, 0.8660254037844387076, 1.000000000000000000, 0.8660254037844387076, 1.000000000000000000, 0.9330127018922194093, 0.9330127018922194093 ) ) 
 REPRESENTATION_ITEM ( '' )  );
#6157 = CARTESIAN_POINT ( 'NONE',  ( 4.059375000614519280, 4.541064518000418104, -2.621784821874998173 ) ) ;
#6158 = CARTESIAN_POINT ( 'NONE',  ( 23.50312500061451360, 0.000000000000000000, 5.243569643749999010 ) ) ;
#6159 = CARTESIAN_POINT ( 'NONE',  ( 3.756430356250000102, 15.90312499938548108, 30.00000000000000000 ) ) ;
#6160 = CARTESIAN_POINT ( 'NONE',  ( 0.000000000000000000, 20.00000000000000000, 30.00000000000000000 ) ) ;
#6161 = CARTESIAN_POINT ( 'NONE',  ( 7.021875000614518747, -6.054752690667223547, -1.112240025338166033E-15 ) ) ;
#6162 = CARTESIAN_POINT ( 'NONE',  ( 20.78732959644809952, -4.500000000000000000, 3.499999999999999556 ) ) ;
#6163 = CARTESIAN_POINT ( 'NONE',  ( 27.25312500061451360, -4.541064518000417216, -2.621784821875001281 ) ) ;
#6164 = CARTESIAN_POINT ( 'NONE',  ( 6.421875000614519102, 3.027376345333611329, 5.243569643749999010 ) ) ;
#6165 = CARTESIAN_POINT ( 'NONE',  ( 0.000000000000000000, 12.50000000000000000, 30.00000000000000000 ) ) ;
#6166 = CARTESIAN_POINT ( 'NONE',  ( 26.52187500061451431, 3.027376345333613106, -5.243569643749998122 ) ) ;
#6167 = CARTESIAN_POINT ( 'NONE',  ( 4.243569643749999898, 10.12812500061459353, 30.00000000000000000 ) ) ;
#6168 = CARTESIAN_POINT ( 'NONE',  ( 18.30000000000000071, 0.000000000000000000, 4.999999999999998224 ) ) ;
#6169 = ORIENTED_EDGE ( 'NONE', *, *, #36318, .F. ) ;
#6170 = CARTESIAN_POINT ( 'NONE',  ( 27.41250000000000142, -5.773502691896255534, -1.060575238724906372E-15 ) ) ;
#6171 = CARTESIAN_POINT ( 'NONE',  ( 28.32187500061451502, 3.027376345333613106, -5.243569643749998122 ) ) ;
#6172 = ORIENTED_EDGE ( 'NONE', *, *, #61587, .T. ) ;
#6173 = CARTESIAN_POINT ( 'NONE',  ( 15.70312500061451644, 4.541064518000418104, -2.621784821874998173 ) ) ;
#6174 = CARTESIAN_POINT ( 'NONE',  ( 8.090625000614515727, 6.054752690667223547, 3.707466751127219781E-16 ) ) ;
#6175 = CARTESIAN_POINT ( 'NONE',  ( 18.72187500061451360, 5.824947211148865298E-16, -4.756430356249998326 ) ) ;
#6176 = CARTESIAN_POINT ( 'NONE',  ( 5.634375000614519458, -4.541064518000419881, 2.621784821874995952 ) ) ;
#6177 =( BOUNDED_CURVE ( )  B_SPLINE_CURVE ( 2, ( #57360, #18552, #63627, #13017, #35555, #69906, #68828 ),
 .UNSPECIFIED., .F., .F. ) 
 B_SPLINE_CURVE_WITH_KNOTS ( ( 3, 2, 2, 3 ),
 ( 0.9100000000000000311, 0.9133333333333333304, 0.9166666666666667407, 0.9200000000000001510 ),
 .UNSPECIFIED. ) 
 CURVE ( )  GEOMETRIC_REPRESENTATION_ITEM ( )  RATIONAL_B_SPLINE_CURVE ( ( 1.000000000000000000, 0.8660254037844387076, 1.000000000000000000, 0.8660254037844387076, 1.000000000000000000, 0.8660254037844342667, 1.000000000000004441 ) ) 
 REPRESENTATION_ITEM ( '' )  );
#6178 = CARTESIAN_POINT ( 'NONE',  ( 16.91250000122903430, 4.330127018922192761, -2.499999999999997780 ) ) ;
#6179 = CARTESIAN_POINT ( 'NONE',  ( 21.97500000000000142, -4.330127018922194537, 2.499999999999995559 ) ) ;
#6180 = CARTESIAN_POINT ( 'NONE',  ( 29.96250000000000213, 2.886751345948126879, 4.999999999999999112 ) ) ;
#6181 = CARTESIAN_POINT ( 'NONE',  ( 3.496875000614518836, -3.027376345333610441, -5.243569643749999898 ) ) ;
#6182 = CARTESIAN_POINT ( 'NONE',  ( 12.15937500061451892, 4.541064518000418104, -2.621784821874998173 ) ) ;
#6183 = CARTESIAN_POINT ( 'NONE',  ( 22.92187500061451644, 3.027376345333613106, -5.243569643749998122 ) ) ;
#6184 = CARTESIAN_POINT ( 'NONE',  ( -3.999999999999997335, 15.20000000122903572, -27.69059892324149530 ) ) ;
#6185 = EDGE_LOOP ( 'NONE', ( #61084, #1603, #60824, #24890 ) ) ;
#6186 = CARTESIAN_POINT ( 'NONE',  ( 3.609375000614516882, 4.541064518000418104, -2.621784821874998173 ) ) ;
#6187 = CARTESIAN_POINT ( 'NONE',  ( 7.396875000614519635, -3.027376345333614438, 5.243569643749998122 ) ) ;
#6188 = CARTESIAN_POINT ( 'NONE',  ( 18.71249999999999858, 2.886751345948126879, 4.999999999999999112 ) ) ;
#6189 = CARTESIAN_POINT ( 'NONE',  ( 15.40312500061451573, 0.000000000000000000, 5.243569643749999010 ) ) ;
#6190 = CARTESIAN_POINT ( 'NONE',  ( -1.999999999999999112, 20.29999999999999716, 26.53589838486224650 ) ) ;
#6191 = DIRECTION ( 'NONE',  ( -1.000000000000000000, -0.000000000000000000, -0.000000000000000000 ) ) ;
#6192 = CARTESIAN_POINT ( 'NONE',  ( 19.80937500061451573, 4.119189519843966529, -2.378215178124998275 ) ) ;
#6193 = CARTESIAN_POINT ( 'NONE',  ( 9.928125000614517859, 4.541064518000418104, 2.621784821874999949 ) ) ;
#6194 = CARTESIAN_POINT ( 'NONE',  ( 25.73437500061451644, 4.541064518000418104, 2.621784821874999949 ) ) ;
#6195 = CARTESIAN_POINT ( 'NONE',  ( 12.90000000000000213, 0.000000000000000000, 4.999999999999998224 ) ) ;
#6196 = CARTESIAN_POINT ( 'NONE',  ( 26.07187500061451857, 3.027376345333613106, -5.243569643749998122 ) ) ;
#6197 = CARTESIAN_POINT ( 'NONE',  ( 10.98750000000000071, 5.773502691896255534, 3.535250795749688894E-16 ) ) ;
#6198 = CARTESIAN_POINT ( 'NONE',  ( 2.000000000000001332, 16.21250000122903501, 33.46410161513774995 ) ) ;
#6199 = CARTESIAN_POINT ( 'NONE',  ( 8.212500001229035007, -4.330127018922190985, -2.500000000000001332 ) ) ;
#6200 = EDGE_CURVE ( 'NONE', #70091, #8864, #45274, .T. ) ;
#6201 = CARTESIAN_POINT ( 'NONE',  ( 19.54687500061451644, -3.027376345333614438, 5.243569643749998122 ) ) ;
#6202 = CARTESIAN_POINT ( 'NONE',  ( 14.74687500061451573, -3.027376345333610441, -5.243569643749999898 ) ) ;
#6203 = VERTEX_POINT ( 'NONE', #66721 ) ;
#6204 = CARTESIAN_POINT ( 'NONE',  ( 15.02812500061451750, -4.541064518000419881, 2.621784821874995952 ) ) ;
#6205 = CARTESIAN_POINT ( 'NONE',  ( 26.10000000122903430, -2.886751345948129988, 4.999999999999997335 ) ) ;
#6206 = CARTESIAN_POINT ( 'NONE',  ( 13.95937500061451786, 4.541064518000418104, -2.621784821874998173 ) ) ;
#6207 = CARTESIAN_POINT ( 'NONE',  ( 1.999999999999998668, 12.76250000122903394, 26.53589838486224650 ) ) ;
#6208 = CARTESIAN_POINT ( 'NONE',  ( 17.57812500061451644, 4.541064518000418104, 2.621784821874999949 ) ) ;
#6209 = EDGE_CURVE ( 'NONE', #51293, #9005, #5308, .T. ) ;
#6210 = LINE ( 'NONE', #29469, #72836 ) ;
#6211 = CARTESIAN_POINT ( 'NONE',  ( 25.20937500061451431, 4.541064518000418104, -2.621784821874998173 ) ) ;
#6212 = CARTESIAN_POINT ( 'NONE',  ( 2.917166856763841132, -4.060812204189049091, 3.317359856706287413 ) ) ;
#6213 = CARTESIAN_POINT ( 'NONE',  ( 16.02187500061451786, -6.054752690667223547, -1.112240025338166033E-15 ) ) ;
#6214 = CARTESIAN_POINT ( 'NONE',  ( 11.81250000122903465, -4.330127018922190985, -2.500000000000001332 ) ) ;
#6215 = DIRECTION ( 'NONE',  ( 0.000000000000000000, 0.000000000000000000, -1.000000000000000000 ) ) ;
#6216 = CARTESIAN_POINT ( 'NONE',  ( 4.243569643749999010, 17.42187500061451999, -32.45002607614398471 ) ) ;
#6217 = ADVANCED_FACE ( 'NONE', ( #27559 ), #10921, .F. ) ;
#6218 = CARTESIAN_POINT ( 'NONE',  ( 18.00937500061451502, 4.541064518000418104, -2.621784821874998173 ) ) ;
#6219 = CARTESIAN_POINT ( 'NONE',  ( 20.92500000122903714, 2.886751345948129099, -4.999999999999998224 ) ) ;
#6220 = CARTESIAN_POINT ( 'NONE',  ( 14.03437500061451715, 4.541064518000418104, 2.621784821874999949 ) ) ;
#6221 = CARTESIAN_POINT ( 'NONE',  ( 4.243569643749999010, 12.92187500061451644, 27.54997392385601174 ) ) ;
#6222 = CARTESIAN_POINT ( 'NONE',  ( 22.65000000122903856, -2.886751345948125991, -5.000000000000000000 ) ) ;
#6223 = CARTESIAN_POINT ( 'NONE',  ( 14.39062500061451821, 6.054752690667223547, 3.707466751127219781E-16 ) ) ;
#6224 = CARTESIAN_POINT ( 'NONE',  ( 29.80312500061451431, 0.000000000000000000, 5.243569643749999010 ) ) ;
#6225 = ORIENTED_EDGE ( 'NONE', *, *, #37306, .T. ) ;
#6226 = VERTEX_POINT ( 'NONE', #55992 ) ;
#6227 = CARTESIAN_POINT ( 'NONE',  ( 20.02500000000000213, 4.330127018922191873, 2.499999999999999556 ) ) ;
#6228 = CARTESIAN_POINT ( 'NONE',  ( 7.320879633048903241E-15, 17.75000000122903288, 26.00000000000000355 ) ) ;
#6229 = CARTESIAN_POINT ( 'NONE',  ( 3.178125000614515638, 4.541064518000418104, 2.621784821874999949 ) ) ;
#6230 = CARTESIAN_POINT ( 'NONE',  ( 14.06250000122903288, -4.330127018922190985, -2.500000000000001332 ) ) ;
#6231 = CARTESIAN_POINT ( 'NONE',  ( 21.14062500061451289, 6.054752690667223547, 3.707466751127219781E-16 ) ) ;
#6232 = CARTESIAN_POINT ( 'NONE',  ( 22.34062500061451573, -3.027376345333610441, -5.243569643749999898 ) ) ;
#6233 = CARTESIAN_POINT ( 'NONE',  ( 29.58750000122903501, 4.330127018922191873, 2.499999999999999556 ) ) ;
#6234 = VECTOR ( 'NONE', #39196, 1000.000000000000000 ) ;
#6235 = CARTESIAN_POINT ( 'NONE',  ( 26.77500000122903145, 2.886751345948112668, -5.000000000000024869 ) ) ;
#6236 = CARTESIAN_POINT ( 'NONE',  ( 4.582326623766785900, 2.000647313145979656, 4.846930428394146340 ) ) ;
#6237 = CARTESIAN_POINT ( 'NONE',  ( 8.896875000614517859, -2.746126346562642428, -4.756430356249999214 ) ) ;
#6238 = DIRECTION ( 'NONE',  ( -0.000000000000000000, -1.000000000000000000, -0.000000000000000000 ) ) ;
#6239 = CARTESIAN_POINT ( 'NONE',  ( 1.999999999999998668, 11.86250000122903359, -33.46410161513775705 ) ) ;
#6240 = CARTESIAN_POINT ( 'NONE',  ( 4.243569643749999898, 17.79687500061451999, -27.54997392385601529 ) ) ;
#6241 = EDGE_CURVE ( 'NONE', #37474, #69178, #40775, .T. ) ;
#6242 = CARTESIAN_POINT ( 'NONE',  ( 5.962500001229033231, -4.330127018922190985, -2.500000000000001332 ) ) ;
#6243 = CARTESIAN_POINT ( 'NONE',  ( 7.875000000000000000, 4.330127018922191873, 2.499999999999999556 ) ) ;
#6244 = CARTESIAN_POINT ( 'NONE',  ( 4.350000001229033408, 5.773502691896255534, 3.535250795749688894E-16 ) ) ;
#6245 = CARTESIAN_POINT ( 'NONE',  ( 11.14687500061451608, -3.027376345333610441, -5.243569643749999898 ) ) ;
#6246 = CARTESIAN_POINT ( 'NONE',  ( 3.999999999999998668, 16.77500000122903145, -32.30940107675850470 ) ) ;
#6247 = CARTESIAN_POINT ( 'NONE',  ( 3.046875000614519990, -3.027376345333610441, -5.243569643749999898 ) ) ;
#6248 = CARTESIAN_POINT ( 'NONE',  ( 18.75000000000000000, 0.000000000000000000, 4.999999999999998224 ) ) ;
#6249 = CARTESIAN_POINT ( 'NONE',  ( 12.61875000122903145, -5.773502691896255534, -1.060575238724906372E-15 ) ) ;
#6250 = CARTESIAN_POINT ( 'NONE',  ( 11.29687500061451644, 6.054752690667223547, 3.707466751127219781E-16 ) ) ;
#6251 = CARTESIAN_POINT ( 'NONE',  ( 13.77187500061451786, -6.054752690667223547, -1.112240025338166033E-15 ) ) ;
#6252 = CARTESIAN_POINT ( 'NONE',  ( 1.999999999999998668, 14.11250000122903359, -33.46410161513775705 ) ) ;
#6253 = CARTESIAN_POINT ( 'NONE',  ( 6.750000000000002665, -4.330127018922190985, -2.500000000000001332 ) ) ;
#6254 = CARTESIAN_POINT ( 'NONE',  ( -2.121784821874999949, 17.47812500061459673, 26.32496088578401938 ) ) ;
#6255 = CARTESIAN_POINT ( 'NONE',  ( 21.79687500061451644, -3.027376345333614438, 5.243569643749998122 ) ) ;
#6256 = CARTESIAN_POINT ( 'NONE',  ( 2.752374072010383532, -4.174317300471400927, 2.814089559418405884 ) ) ;
#6257 = CARTESIAN_POINT ( 'NONE',  ( 27.07500000122903216, -5.773502691896255534, -1.060575238724906372E-15 ) ) ;
#6258 = CARTESIAN_POINT ( 'NONE',  ( 17.40937500061451360, 2.746126346562645981, -4.756430356249997438 ) ) ;
#6259 = CARTESIAN_POINT ( 'NONE',  ( 22.82812500061451644, 6.421520780324663323E-16, -5.243569643749999010 ) ) ;
#6260 = CARTESIAN_POINT ( 'NONE',  ( 14.61562500061451608, -6.054752690667223547, -1.112240025338166033E-15 ) ) ;
#6261 = CARTESIAN_POINT ( 'NONE',  ( 25.62187500061451573, 4.119189519843966529, 2.378215178124999607 ) ) ;
#6262 = CARTESIAN_POINT ( 'NONE',  ( 11.44687500061451857, -3.027376345333614438, 5.243569643749998122 ) ) ;
#6263 = CARTESIAN_POINT ( 'NONE',  ( 28.72500000000000142, -4.330127018922194537, 2.499999999999995559 ) ) ;
#6264 = CARTESIAN_POINT ( 'NONE',  ( 25.53750000122903074, 4.330127018922191873, 2.499999999999999556 ) ) ;
#6265 = CARTESIAN_POINT ( 'NONE',  ( 4.209375000614516971, 0.000000000000000000, 5.243569643749999010 ) ) ;
#6266 = CARTESIAN_POINT ( 'NONE',  ( 10.99687500061451750, -3.027376345333614438, 5.243569643749998122 ) ) ;
#6267 = CARTESIAN_POINT ( 'NONE',  ( 28.24687500061451573, -3.027376345333610441, -5.243569643749999898 ) ) ;
#6268 = CYLINDRICAL_SURFACE ( 'NONE', #13559, 4.000000000000000000 ) ;
#6269 = CARTESIAN_POINT ( 'NONE',  ( 30.00000000000000000, 0.000000000000000000, 0.000000000000000000 ) ) ;
#6270 = CARTESIAN_POINT ( 'NONE',  ( 23.33437500061451786, 6.421520780324663323E-16, -5.243569643749999010 ) ) ;
#6271 = CARTESIAN_POINT ( 'NONE',  ( 13.35937500061451821, -4.541064518000417216, -2.621784821875001281 ) ) ;
#6272 = CARTESIAN_POINT ( 'NONE',  ( 1.878215178125000495, 17.77812499938548285, 26.74683588394047007 ) ) ;
#6273 = CARTESIAN_POINT ( 'NONE',  ( 26.09999999999999787, -4.330127018922190985, -2.500000000000001332 ) ) ;
#6274 = CARTESIAN_POINT ( 'NONE',  ( 4.162500001229033408, -4.330127018922190985, -2.500000000000001332 ) ) ;
#6275 = CARTESIAN_POINT ( 'NONE',  ( 26.63437500061451857, 4.119189519843966529, 2.378215178124999607 ) ) ;
#6276 = CARTESIAN_POINT ( 'NONE',  ( 16.07812500061451289, 6.421520780324663323E-16, -5.243569643749999010 ) ) ;
#6277 = CARTESIAN_POINT ( 'NONE',  ( 6.600000000000001421, 0.000000000000000000, 4.999999999999998224 ) ) ;
#6278 = CARTESIAN_POINT ( 'NONE',  ( 13.53750000122903430, -4.330127018922194537, 2.499999999999995559 ) ) ;
#6279 = CARTESIAN_POINT ( 'NONE',  ( 18.03749999999999787, -2.886751345948125991, -5.000000000000000000 ) ) ;
#6280 = CARTESIAN_POINT ( 'NONE',  ( 2.121784821874999061, 12.45312500061451821, 26.32496088578401583 ) ) ;
#6281 = CARTESIAN_POINT ( 'NONE',  ( -1.999999999999999112, 16.25000000000000000, 26.53589838486224650 ) ) ;
#6282 = CARTESIAN_POINT ( 'NONE',  ( 20.47500000122903074, 2.886751345948129099, -4.999999999999998224 ) ) ;
#6283 = CARTESIAN_POINT ( 'NONE',  ( 26.70937500061451431, 0.000000000000000000, 5.243569643749999010 ) ) ;
#6284 = ORIENTED_EDGE ( 'NONE', *, *, #65329, .T. ) ;
#6285 = CARTESIAN_POINT ( 'NONE',  ( 21.62812500061451360, 4.541064518000418104, 2.621784821874999949 ) ) ;
#6286 = B_SPLINE_CURVE_WITH_KNOTS ( 'NONE', 3,
 ( #41316, #52033, #63474, #1800, #19482, #30222, #24669, #30942, #42040, #24310 ),
 .UNSPECIFIED., .F., .F.,
 ( 4, 3, 3, 4 ),
 ( 4.080289400222272056E-17, 7.861589888542538148E-05, 0.0001572322621546033250, 0.0002879325728988927887 ),
 .UNSPECIFIED. ) ;
#6287 = CARTESIAN_POINT ( 'NONE',  ( 21.53437500061451715, 6.421520780324663323E-16, -5.243569643749999010 ) ) ;
#6288 = CARTESIAN_POINT ( 'NONE',  ( 4.387500000000002842, -2.886751345948129988, 4.999999999999997335 ) ) ;
#6289 = CARTESIAN_POINT ( 'NONE',  ( 7.228125000614517681, 4.541064518000418104, 2.621784821874999949 ) ) ;
#6290 = CARTESIAN_POINT ( 'NONE',  ( 23.20312500061451644, -4.541064518000417216, -2.621784821875001281 ) ) ;
#6291 = CARTESIAN_POINT ( 'NONE',  ( 13.43437500061451750, 6.421520780324663323E-16, -5.243569643749999010 ) ) ;
#6292 = CARTESIAN_POINT ( 'NONE',  ( 15.79687500061451821, 6.054752690667223547, 3.707466751127219781E-16 ) ) ;
#6293 = CARTESIAN_POINT ( 'NONE',  ( -4.243569643749997233, 17.14062500061451644, 32.45002607614398471 ) ) ;
#6294 = CARTESIAN_POINT ( 'NONE',  ( 22.31250000122903288, 4.330127018922192761, -2.499999999999997780 ) ) ;
#6295 = CARTESIAN_POINT ( 'NONE',  ( 15.12187500061451928, -5.492252693125287522, -1.008910452111647106E-15 ) ) ;
#6296 = CARTESIAN_POINT ( 'NONE',  ( 10.71562500061451750, 3.027376345333612662, -5.243569643749998122 ) ) ;
#6297 = CARTESIAN_POINT ( 'NONE',  ( 5.559375000614517504, 0.000000000000000000, 5.243569643749999010 ) ) ;
#6298 = CARTESIAN_POINT ( 'NONE',  ( 4.809375000614516615, -4.541064518000417216, -2.621784821875001281 ) ) ;
#6299 = ORIENTED_EDGE ( 'NONE', *, *, #43763, .F. ) ;
#6300 = EDGE_CURVE ( 'NONE', #37421, #30066, #43821, .T. ) ;
#6301 = CARTESIAN_POINT ( 'NONE',  ( 24.45937500061451786, 0.000000000000000000, 5.243569643749999010 ) ) ;
#6302 = CARTESIAN_POINT ( 'NONE',  ( 15.92812500061451608, -4.541064518000419881, 2.621784821874995952 ) ) ;
#6303 = CARTESIAN_POINT ( 'NONE',  ( 26.55000000122902648, -2.886751345948129988, 4.999999999999997335 ) ) ;
#6304 = CARTESIAN_POINT ( 'NONE',  ( 28.79062500061451502, 6.054752690667223547, 3.707466751127219781E-16 ) ) ;
#6305 = CARTESIAN_POINT ( 'NONE',  ( 20.74687500061451573, 6.054752690667223547, 3.707466751127219781E-16 ) ) ;
#6306 = CARTESIAN_POINT ( 'NONE',  ( 17.76562500061451644, -6.054752690667223547, -1.112240025338166033E-15 ) ) ;
#6307 = CARTESIAN_POINT ( 'NONE',  ( -4.243569643749997233, 18.99687500061451928, 32.45002607614398471 ) ) ;
#6308 = CARTESIAN_POINT ( 'NONE',  ( 22.41562500061451502, 3.027376345333613106, -5.243569643749998122 ) ) ;
#6309 = CARTESIAN_POINT ( 'NONE',  ( 3.187500001229033764, -4.330127018922194537, 2.499999999999995559 ) ) ;
#6310 = EDGE_LOOP ( 'NONE', ( #62679, #9673, #1955, #58484 ) ) ;
#6311 = CARTESIAN_POINT ( 'NONE',  ( 27.00000000000000000, -4.330127018922190985, -2.500000000000001332 ) ) ;
#6312 = CARTESIAN_POINT ( 'NONE',  ( -2.828200636599751609E-16, 14.03750000000000142, -34.61880215351700230 ) ) ;
#6313 = CARTESIAN_POINT ( 'NONE',  ( 1.878215178124997609, 18.07812499938548356, 33.25316411605952993 ) ) ;
#6314 = CARTESIAN_POINT ( 'NONE',  ( 29.16562500061451502, 3.027376345333613106, -5.243569643749998122 ) ) ;
#6315 = CARTESIAN_POINT ( 'NONE',  ( 10.94062500061451537, -3.027376345333614438, 5.243569643749998122 ) ) ;
#6316 = CARTESIAN_POINT ( 'NONE',  ( 21.71250000122903501, -4.330127018922190985, -2.500000000000001332 ) ) ;
#6317 = CARTESIAN_POINT ( 'NONE',  ( 12.27187500061451608, 3.027376345333611329, 5.243569643749999010 ) ) ;
#6318 = CARTESIAN_POINT ( 'NONE',  ( 27.92812500061451431, 4.541064518000418104, 2.621784821874999949 ) ) ;
#6319 = CARTESIAN_POINT ( 'NONE',  ( 27.18750000000000000, 5.773502691896255534, 3.535250795749688894E-16 ) ) ;
#6320 = CARTESIAN_POINT ( 'NONE',  ( -3.999999999999999556, 19.17500000122903359, -32.30940107675850470 ) ) ;
#6321 = LINE ( 'NONE', #52836, #33804 ) ;
#6322 = CARTESIAN_POINT ( 'NONE',  ( 11.76562500061451644, 3.027376345333611329, 5.243569643749999010 ) ) ;
#6323 = ORIENTED_EDGE ( 'NONE', *, *, #39198, .T. ) ;
#6324 = CARTESIAN_POINT ( 'NONE',  ( 6.553125000614518747, -4.541064518000417216, -2.621784821875001281 ) ) ;
#6325 = CARTESIAN_POINT ( 'NONE',  ( 5.840625000614516615, 6.054752690667223547, 3.707466751127219781E-16 ) ) ;
#6326 = CARTESIAN_POINT ( 'NONE',  ( 15.98437500061451821, -4.119189519843968306, 2.378215178124996054 ) ) ;
#6327 = CARTESIAN_POINT ( 'NONE',  ( 9.862500001229033586, 0.000000000000000000, 4.999999999999998224 ) ) ;
#6328 = CARTESIAN_POINT ( 'NONE',  ( 14.77500000000000036, -4.330127018922194537, 2.499999999999995559 ) ) ;
#6329 = CARTESIAN_POINT ( 'NONE',  ( 15.38437500061451679, 4.541064518000418104, 2.621784821874999949 ) ) ;
#6330 = CARTESIAN_POINT ( 'NONE',  ( 10.83750000122903501, -4.330127018922194537, 2.499999999999995559 ) ) ;
#6331 = CARTESIAN_POINT ( 'NONE',  ( 18.42187500061451644, 3.027376345333613106, -5.243569643749998122 ) ) ;
#6332 = CARTESIAN_POINT ( 'NONE',  ( 16.50000000000000000, 0.000000000000000000, 4.999999999999998224 ) ) ;
#6333 = CARTESIAN_POINT ( 'NONE',  ( 21.30937500061451573, 0.000000000000000000, 5.243569643749999010 ) ) ;
#6334 = CARTESIAN_POINT ( 'NONE',  ( -2.121784821874996840, 14.02812500061451750, -26.32496088578401583 ) ) ;
#6335 = CARTESIAN_POINT ( 'NONE',  ( 7.500000000000000000, 0.000000000000000000, 4.999999999999998224 ) ) ;
#6336 = CARTESIAN_POINT ( 'NONE',  ( 25.47187500061451360, 5.824947211148865298E-16, -4.756430356249998326 ) ) ;
#6337 = CARTESIAN_POINT ( 'NONE',  ( -1.243387493232115393E-14, 15.25624999877096677, 26.00000000000000000 ) ) ;
#6338 = ADVANCED_FACE ( 'NONE', ( #55268 ), #216, .F. ) ;
#6339 = CARTESIAN_POINT ( 'NONE',  ( 26.99062500061451431, 6.054752690667223547, 3.707466751127219781E-16 ) ) ;
#6340 = CARTESIAN_POINT ( 'NONE',  ( 65.00000000000000000, 0.000000000000000000, 0.000000000000000000 ) ) ;
#6341 = CARTESIAN_POINT ( 'NONE',  ( 28.17187500061451644, -6.054752690667223547, -1.112240025338166033E-15 ) ) ;
#6342 = CARTESIAN_POINT ( 'NONE',  ( 24.14999999999999858, 0.000000000000000000, 4.999999999999998224 ) ) ;
#6343 = CARTESIAN_POINT ( 'NONE',  ( 5.915625000614515905, 3.027376345333611329, 5.243569643749999010 ) ) ;
#6344 = CARTESIAN_POINT ( 'NONE',  ( 24.15937500061451360, 2.746126346562645981, -4.756430356249997438 ) ) ;
#6345 = CARTESIAN_POINT ( 'NONE',  ( 20.03437500061451715, -4.541064518000419881, 2.621784821874995952 ) ) ;
#6346 = CARTESIAN_POINT ( 'NONE',  ( 10.54687500061451644, -4.119189519843965641, -2.378215178125001383 ) ) ;
#6347 = CARTESIAN_POINT ( 'NONE',  ( 5.165625000614518569, -6.054752690667223547, -1.112240025338166033E-15 ) ) ;
#6348 = CARTESIAN_POINT ( 'NONE',  ( 9.684375000614517504, -4.541064518000419881, 2.621784821874995952 ) ) ;
#6349 = ORIENTED_EDGE ( 'NONE', *, *, #39819, .T. ) ;
#6350 = CARTESIAN_POINT ( 'NONE',  ( 21.75937500061451502, 0.000000000000000000, 5.243569643749999010 ) ) ;
#6351 = CARTESIAN_POINT ( 'NONE',  ( -1.071796769724492115, 15.91115380933863577, 34.00000000000000000 ) ) ;
#6352 = CARTESIAN_POINT ( 'NONE',  ( 29.25000000000000000, -4.330127018922190985, -2.500000000000001332 ) ) ;
#6353 = CARTESIAN_POINT ( 'NONE',  ( 29.55937500061451573, -4.541064518000417216, -2.621784821875001281 ) ) ;
#6354 = CYLINDRICAL_SURFACE ( 'NONE', #40790, 4.999999999999998224 ) ;
#6355 = CARTESIAN_POINT ( 'NONE',  ( 12.39375000122903536, 5.773502691896255534, 3.535250795749688401E-16 ) ) ;
#6356 = ORIENTED_EDGE ( 'NONE', *, *, #28164, .T. ) ;
#6357 = CARTESIAN_POINT ( 'NONE',  ( 10.49999999999999822, 4.330127018922192761, -2.499999999999997780 ) ) ;
#6358 = CARTESIAN_POINT ( 'NONE',  ( 12.04687500061451821, 4.119189519843966529, -2.378215178124998275 ) ) ;
#6359 = CARTESIAN_POINT ( 'NONE',  ( 24.47812500061451502, -4.541064518000419881, 2.621784821874995952 ) ) ;
#6360 = CARTESIAN_POINT ( 'NONE',  ( 14.40000000000000036, -4.330127018922190985, -2.500000000000001332 ) ) ;
#6361 = CARTESIAN_POINT ( 'NONE',  ( 11.17500000122903536, 2.886751345948126879, 4.999999999999999112 ) ) ;
#6362 = CARTESIAN_POINT ( 'NONE',  ( 8.578125000614518214, 4.541064518000418104, 2.621784821874999949 ) ) ;
#6363 =( BOUNDED_CURVE ( )  B_SPLINE_CURVE ( 2, ( #20687, #43246, #49876, #9981, #38423, #60208, #49154, #26617, #55780 ),
 .UNSPECIFIED., .F., .F. ) 
 B_SPLINE_CURVE_WITH_KNOTS ( ( 3, 2, 2, 2, 3 ),
 ( 0.5543478260869565410, 0.5579710144927536586, 0.5652173913043477826, 0.5724637681159420177, 0.5760869565217391353 ),
 .UNSPECIFIED. ) 
 CURVE ( )  GEOMETRIC_REPRESENTATION_ITEM ( )  RATIONAL_B_SPLINE_CURVE ( ( 0.9330127018922194093, 0.9330127018922194093, 1.000000000000000000, 0.8660254037844387076, 1.000000000000000000, 0.8660254037844387076, 1.000000000000000000, 0.9330127018922194093, 0.9330127018922194093 ) ) 
 REPRESENTATION_ITEM ( '' )  );
#6364 = CARTESIAN_POINT ( 'NONE',  ( 9.487500000000000711, -2.886751345948125991, -5.000000000000000000 ) ) ;
#6365 = CYLINDRICAL_SURFACE ( 'NONE', #26599, 4.999999999999998224 ) ;
#6366 = CARTESIAN_POINT ( 'NONE',  ( 28.46250000122903145, -4.330127018922190985, -2.500000000000001332 ) ) ;
#6367 = CARTESIAN_POINT ( 'NONE',  ( 1.878215178125000495, 16.31562499938548427, 26.74683588394047007 ) ) ;
#6368 = CARTESIAN_POINT ( 'NONE',  ( 8.625000000000000000, 6.123233995736764310E-16, -4.999999999999998224 ) ) ;
#6369 = DIRECTION ( 'NONE',  ( -0.000000000000000000, -1.000000000000000000, -0.000000000000000000 ) ) ;
#6370 = ORIENTED_EDGE ( 'NONE', *, *, #41487, .T. ) ;
#6371 = CARTESIAN_POINT ( 'NONE',  ( 21.70312500061451644, 0.000000000000000000, 5.243569643749999010 ) ) ;
#6372 = CARTESIAN_POINT ( 'NONE',  ( 28.19062500061451715, -3.027376345333610441, -5.243569643749999898 ) ) ;
#6373 = CARTESIAN_POINT ( 'NONE',  ( 29.33437500061451431, 4.541064518000418104, 2.621784821874999949 ) ) ;
#6374 = CARTESIAN_POINT ( 'NONE',  ( 18.90937500061451360, 4.541064518000418104, -2.621784821874998173 ) ) ;
#6375 = CARTESIAN_POINT ( 'NONE',  ( 17.31562500061451715, -6.054752690667223547, -1.112240025338166033E-15 ) ) ;
#6376 = CARTESIAN_POINT ( 'NONE',  ( 2.121784821875001281, 12.75312500061459353, -26.32496088578401938 ) ) ;
#6377 = CARTESIAN_POINT ( 'NONE',  ( 4.903125000614516615, 4.541064518000418104, -2.621784821874998173 ) ) ;
#6378 = CARTESIAN_POINT ( 'NONE',  ( 28.12500000122902932, 2.886751345948129099, -4.999999999999998224 ) ) ;
#6379 = CARTESIAN_POINT ( 'NONE',  ( 21.60937500061451644, 4.119189519843966529, -2.378215178124998275 ) ) ;
#6380 = CARTESIAN_POINT ( 'NONE',  ( 18.06562500061451715, 3.027376345333611329, 5.243569643749999010 ) ) ;
#6381 = CARTESIAN_POINT ( 'NONE',  ( 3.999999999999998668, 13.96250000000000036, 27.69059892324149530 ) ) ;
#6382 = CARTESIAN_POINT ( 'NONE',  ( 4.125000001229034652, -5.773502691896255534, -1.060575238724906372E-15 ) ) ;
#6383 = CARTESIAN_POINT ( 'NONE',  ( 12.19687500061451679, 6.054752690667223547, 3.707466751127219781E-16 ) ) ;
#6384 = CARTESIAN_POINT ( 'NONE',  ( 12.08437500061451608, 6.421520780324663323E-16, -5.243569643749999010 ) ) ;
#6385 = CARTESIAN_POINT ( 'NONE',  ( 19.65937500061451360, -4.541064518000417216, -2.621784821875001281 ) ) ;
#6386 = ORIENTED_EDGE ( 'NONE', *, *, #26754, .F. ) ;
#6387 = CARTESIAN_POINT ( 'NONE',  ( -5.672756003115388523, 8.235591643417166097, 31.96448613495275737 ) ) ;
#6388 = CARTESIAN_POINT ( 'NONE',  ( 24.32812500061451289, 4.541064518000418104, 2.621784821874999949 ) ) ;
#6389 = ADVANCED_FACE ( 'NONE', ( #39740 ), #9830, .F. ) ;
#6390 = B_SPLINE_CURVE_WITH_KNOTS ( 'NONE', 3,
 ( #44450, #61053, #56250, #27450, #16344, #66980, #34059, #56600, #5272, #66232 ),
 .UNSPECIFIED., .F., .F.,
 ( 4, 3, 3, 4 ),
 ( 0.000000000000000000, 2.812507756822774961E-05, 5.625015391946155925E-05, 9.833933667866477343E-05 ),
 .UNSPECIFIED. ) ;
#6391 = CARTESIAN_POINT ( 'NONE',  ( 18.45937500061451431, 4.541064518000418104, -2.621784821874998173 ) ) ;
#6392 = CARTESIAN_POINT ( 'NONE',  ( 24.66562500061451502, 3.027376345333613106, -5.243569643749998122 ) ) ;
#6393 = CARTESIAN_POINT ( 'NONE',  ( 15.01875000122903359, 2.886751345948129099, -4.999999999999997335 ) ) ;
#6394 = CARTESIAN_POINT ( 'NONE',  ( 1.999999999999998668, 15.80000000000000071, 26.53589838486224650 ) ) ;
#6395 = AXIS2_PLACEMENT_3D ( 'NONE', #56749, #61938, #27972 ) ;
#6396 = CARTESIAN_POINT ( 'NONE',  ( 3.159375000614518036, 4.541064518000418104, -2.621784821874998173 ) ) ;
#6397 = CARTESIAN_POINT ( 'NONE',  ( 10.76250000122903572, 0.000000000000000000, 4.999999999999998224 ) ) ;
#6398 = CARTESIAN_POINT ( 'NONE',  ( 6.637500001229035718, 4.330127018922191873, 2.499999999999999556 ) ) ;
#6399 = CARTESIAN_POINT ( 'NONE',  ( -1.999999999999997113, 19.17500000000000071, -26.53589838486224295 ) ) ;
#6400 = CARTESIAN_POINT ( 'NONE',  ( 26.66250000122903430, -4.330127018922190985, -2.500000000000001332 ) ) ;
#6401 = CARTESIAN_POINT ( 'NONE',  ( -8.484601909799255319E-16, 18.63124999877096499, 34.61880215351700940 ) ) ;
#6402 = CARTESIAN_POINT ( 'NONE',  ( 16.74375000122903145, -2.886751345948125991, -5.000000000000000000 ) ) ;
#6403 = CARTESIAN_POINT ( 'NONE',  ( 8.934375000614517504, 6.421520780324663323E-16, -5.243569643749999010 ) ) ;
#6404 = CARTESIAN_POINT ( 'NONE',  ( 17.69999999999999929, 4.330127018922192761, -2.499999999999997780 ) ) ;
#6405 = CARTESIAN_POINT ( 'NONE',  ( 17.09062500061451573, 6.054752690667223547, 3.707466751127219781E-16 ) ) ;
#6406 = CARTESIAN_POINT ( 'NONE',  ( 10.65937500061451715, -4.541064518000417216, -2.621784821875001281 ) ) ;
#6407 = CARTESIAN_POINT ( 'NONE',  ( 3.215625000614518836, 3.027376345333611329, 5.243569643749999010 ) ) ;
#6408 = CARTESIAN_POINT ( 'NONE',  ( 19.88437500061451857, 4.541064518000418104, 2.621784821874999949 ) ) ;
#6409 = CARTESIAN_POINT ( 'NONE',  ( 6.834375000614518747, 4.541064518000418104, 2.621784821874999949 ) ) ;
#6410 = CARTESIAN_POINT ( 'NONE',  ( 20.78732959644809952, 2.500000000000000000, -3.500000000000000000 ) ) ;
#6411 = CARTESIAN_POINT ( 'NONE',  ( 11.77500000122903501, -5.773502691896255534, -1.060575238724906372E-15 ) ) ;
#6412 = CARTESIAN_POINT ( 'NONE',  ( 10.94062500061451537, -3.027376345333614438, 5.243569643749998122 ) ) ;
#6413 = CARTESIAN_POINT ( 'NONE',  ( 20.80312500061451431, 0.000000000000000000, 5.243569643749999010 ) ) ;
#6414 = EDGE_LOOP ( 'NONE', ( #3300, #61462, #38867, #64999, #62594, #72737, #7843, #19691, #68962, #58407, #32626, #67710, #9221, #27099, #63406, #53640, #63613, #8265, #15789, #15095, #65507, #60274, #10624, #8152, #18946, #3454, #69164, #43392, #47718, #1642, #54428, #4921, #17809, #22288, #6900, #36173, #4404, #15217, #33575, #10677, #73049, #57962, #71011, #25947, #51980, #20052, #3466, #30887, #32828, #54016, #30141, #10444, #55127, #60390, #43428, #68594, #1188, #40212, #35685, #70668, #35167, #65057, #20897, #9079, #63554, #11506, #28171, #12208, #66597, #31842, #21523, #11483, #12619, #36475, #41655, #66185, #70034, #18719, #24752, #26722, #51956, #54731, #10545, #44019, #37149, #45369, #45886, #53781, #57412, #71498, #28480, #19780, #5594, #49346, #69361, #49358, #25795, #23696, #821, #12108, #57282, #6356, #6932 ) ) ;
#6415 = CARTESIAN_POINT ( 'NONE',  ( 6.487500001229034474, 6.123233995736764310E-16, -4.999999999999998224 ) ) ;
#6416 = CARTESIAN_POINT ( 'NONE',  ( 15.96562500061451573, -6.054752690667223547, -1.112240025338166033E-15 ) ) ;
#6417 = CARTESIAN_POINT ( 'NONE',  ( 13.86562500061451431, 3.027376345333613106, -5.243569643749998122 ) ) ;
#6418 = CARTESIAN_POINT ( 'NONE',  ( 24.57187500061451502, -5.492252693125287522, -1.008910452111647106E-15 ) ) ;
#6419 = CARTESIAN_POINT ( 'NONE',  ( 12.30000000000000249, 4.330127018922192761, -2.499999999999997780 ) ) ;
#6420 = CARTESIAN_POINT ( 'NONE',  ( 9.262500001229033941, 4.330127018922192761, -2.499999999999997780 ) ) ;
#6421 = CARTESIAN_POINT ( 'NONE',  ( 5.165625000614518569, -6.054752690667223547, -1.112240025338166033E-15 ) ) ;
#6422 = CARTESIAN_POINT ( 'NONE',  ( 17.70000000122903216, -2.886751345948125991, -5.000000000000000000 ) ) ;
#6423 = CARTESIAN_POINT ( 'NONE',  ( 26.58750000000000213, -2.886751345948125991, -5.000000000000000000 ) ) ;
#6424 = CARTESIAN_POINT ( 'NONE',  ( -3.000416591977282496E-16, 12.09687500061451715, -34.90005215228797653 ) ) ;
#6425 = CARTESIAN_POINT ( 'NONE',  ( 8.474999999999999645, -4.330127018922194537, 2.499999999999995559 ) ) ;
#6426 = CARTESIAN_POINT ( 'NONE',  ( 3.900000001229034563, 5.773502691896255534, 3.535250795749688894E-16 ) ) ;
#6427 = CARTESIAN_POINT ( 'NONE',  ( 1.071796769724485232, 14.84240381056766545, 25.99999999999999645 ) ) ;
#6428 = CARTESIAN_POINT ( 'NONE',  ( 18.23437500061451999, -4.541064518000419881, 2.621784821874995952 ) ) ;
#6429 = DIRECTION ( 'NONE',  ( -0.000000000000000000, -1.000000000000000000, -0.000000000000000000 ) ) ;
#6430 = CARTESIAN_POINT ( 'NONE',  ( 16.19062500061451715, 6.054752690667223547, 3.707466751127219781E-16 ) ) ;
#6431 = CARTESIAN_POINT ( 'NONE',  ( 8.868750001229033231, 2.886751345948126879, 4.999999999999999112 ) ) ;
#6432 = CARTESIAN_POINT ( 'NONE',  ( 22.65000000122903856, -2.886751345948092684, -5.000000000000057732 ) ) ;
#6433 = CARTESIAN_POINT ( 'NONE',  ( 29.48437500061451644, -4.541064518000419881, 2.621784821874995952 ) ) ;
#6434 = CARTESIAN_POINT ( 'NONE',  ( 27.00937500061451857, 4.541064518000418104, -2.621784821874998173 ) ) ;
#6435 = CARTESIAN_POINT ( 'NONE',  ( 19.24687500061451573, 4.119189519843966529, -2.378215178124998275 ) ) ;
#6436 = AXIS2_PLACEMENT_3D ( 'NONE', #64013, #35939, #59192 ) ;
#6437 = CARTESIAN_POINT ( 'NONE',  ( 13.45312500061451466, 4.541064518000418104, -2.621784821874998173 ) ) ;
#6438 = CARTESIAN_POINT ( 'NONE',  ( 11.10937500061451644, -4.541064518000417216, -2.621784821875001281 ) ) ;
#6439 = VERTEX_POINT ( 'NONE', #1661 ) ;
#6440 = CARTESIAN_POINT ( 'NONE',  ( 65.00000000000000000, 0.000000000000000000, 0.000000000000000000 ) ) ;
#6441 = CARTESIAN_POINT ( 'NONE',  ( 21.17812500061451431, 4.541064518000418104, 2.621784821874999949 ) ) ;
#6442 = CARTESIAN_POINT ( 'NONE',  ( 18.75000000000000000, 0.000000000000000000, 4.999999999999998224 ) ) ;
#6443 = CARTESIAN_POINT ( 'NONE',  ( 1.071796769724489895, 14.91740381056766829, 26.00000000000000355 ) ) ;
#6444 = CARTESIAN_POINT ( 'NONE',  ( 10.20000000000000107, 0.000000000000000000, 4.999999999999998224 ) ) ;
#6445 = CARTESIAN_POINT ( 'NONE',  ( 20.77500000122903145, -5.773502691896255534, -1.060575238724906372E-15 ) ) ;
#6446 = CARTESIAN_POINT ( 'NONE',  ( 15.14062500061451644, -3.027376345333610441, -5.243569643749999898 ) ) ;
#6447 = CARTESIAN_POINT ( 'NONE',  ( 10.35937500061451644, 2.746126346562643317, 4.756430356249998326 ) ) ;
#6448 = ORIENTED_EDGE ( 'NONE', *, *, #58318, .F. ) ;
#6449 = CARTESIAN_POINT ( 'NONE',  ( 16.46249999999999503, 2.886751345948126879, 4.999999999999999112 ) ) ;
#6450 = CARTESIAN_POINT ( 'NONE',  ( 21.07499999999999929, -4.330127018922194537, 2.499999999999995559 ) ) ;
#6451 = CARTESIAN_POINT ( 'NONE',  ( 19.88437500061451857, 4.541064518000418104, 2.621784821874999949 ) ) ;
#6452 = CARTESIAN_POINT ( 'NONE',  ( 25.82812500061451644, -4.541064518000419881, 2.621784821874995952 ) ) ;
#6453 = ORIENTED_EDGE ( 'NONE', *, *, #40061, .F. ) ;
#6454 = EDGE_CURVE ( 'NONE', #23277, #35963, #5733, .T. ) ;
#6455 = CARTESIAN_POINT ( 'NONE',  ( -3.999999999999997335, 17.00000000122903288, 32.30940107675850470 ) ) ;
#6456 = CARTESIAN_POINT ( 'NONE',  ( 9.065625000614517148, 3.027376345333611329, 5.243569643749999010 ) ) ;
#6457 = CARTESIAN_POINT ( 'NONE',  ( 1.626862140677534273E-15, 15.27500000122903501, 34.00000000000000000 ) ) ;
#6458 = CARTESIAN_POINT ( 'NONE',  ( 13.64999999999999858, 4.330127018922192761, -2.499999999999997780 ) ) ;
#6459 = CARTESIAN_POINT ( 'NONE',  ( -2.121784821874996840, 16.72812500061451857, 33.67503911421598417 ) ) ;
#6460 = CARTESIAN_POINT ( 'NONE',  ( 29.61562500061451431, 3.027376345333613106, -5.243569643749998122 ) ) ;
#6461 = AXIS2_PLACEMENT_3D ( 'NONE', #36951, #59471, #8882 ) ;
#6462 = CARTESIAN_POINT ( 'NONE',  ( 26.10937500061451644, 4.541064518000418104, -2.621784821874998173 ) ) ;
#6463 = VERTEX_POINT ( 'NONE', #12365 ) ;
#6464 = CARTESIAN_POINT ( 'NONE',  ( 22.82812500061451644, 6.421520780324663323E-16, -5.243569643749999010 ) ) ;
#6465 = CARTESIAN_POINT ( 'NONE',  ( 26.40937500061451715, -4.541064518000417216, -2.621784821875001281 ) ) ;
#6466 = CARTESIAN_POINT ( 'NONE',  ( 2.121784821875001281, 17.70312500061459104, -26.32496088578401938 ) ) ;
#6467 = CARTESIAN_POINT ( 'NONE',  ( 12.56250000000000178, -5.773502691896255534, -1.060575238724906372E-15 ) ) ;
#6468 = CARTESIAN_POINT ( 'NONE',  ( 9.515625000614518214, 3.027376345333611329, 5.243569643749999010 ) ) ;
#6469 = CARTESIAN_POINT ( 'NONE',  ( 28.13437500061451502, -4.119189519843968306, 2.378215178124996054 ) ) ;
#6470 = CARTESIAN_POINT ( 'NONE',  ( 28.71562500061451573, 3.027376345333613106, -5.243569643749998122 ) ) ;
#6471 = CARTESIAN_POINT ( 'NONE',  ( 26.57812500061451644, 4.541064518000418104, 2.621784821874999949 ) ) ;
#6472 = CARTESIAN_POINT ( 'NONE',  ( 27.94687500061451502, 0.000000000000000000, 4.756430356249998326 ) ) ;
#6473 = CARTESIAN_POINT ( 'NONE',  ( 13.24687500061451750, -2.746126346562646425, 4.756430356249996549 ) ) ;
#6474 = CARTESIAN_POINT ( 'NONE',  ( 19.47187500061451360, 3.027376345333611329, 5.243569643749999010 ) ) ;
#6475 = CARTESIAN_POINT ( 'NONE',  ( 4.243569643749999010, 12.02187500061451786, 27.54997392385601174 ) ) ;
#6476 = CARTESIAN_POINT ( 'NONE',  ( 20.10937500061451289, -4.541064518000417216, -2.621784821875001281 ) ) ;
#6477 = CARTESIAN_POINT ( 'NONE',  ( 27.90937500061451715, 4.541064518000418104, -2.621784821874998173 ) ) ;
#6478 = CARTESIAN_POINT ( 'NONE',  ( 2.121784821875001281, 16.85937500061451999, 33.67503911421598417 ) ) ;
#6479 = CARTESIAN_POINT ( 'NONE',  ( 7.265625000614516438, 3.027376345333611329, 5.243569643749999010 ) ) ;
#6480 = CARTESIAN_POINT ( 'NONE',  ( 30.00000000000000000, 0.000000000000000000, 0.000000000000000000 ) ) ;
#6481 = EDGE_CURVE ( 'NONE', #53529, #40722, #40677, .T. ) ;
#6482 = CARTESIAN_POINT ( 'NONE',  ( 3.834375000614519635, -4.541064518000419881, 2.621784821874995952 ) ) ;
#6483 = CARTESIAN_POINT ( 'NONE',  ( 3.837848076843224376, 3.204827942194517831, -3.837848076843224376 ) ) ;
#6484 = CARTESIAN_POINT ( 'NONE',  ( 4.078125000614517326, 4.541064518000418104, 2.621784821874999949 ) ) ;
#6485 = CARTESIAN_POINT ( 'NONE',  ( 10.20937500061451786, -4.541064518000417216, -2.621784821875001281 ) ) ;
#6486 = CARTESIAN_POINT ( 'NONE',  ( 20.06250000122903643, 4.330127018922192761, -2.499999999999997780 ) ) ;
#6487 = CARTESIAN_POINT ( 'NONE',  ( 5.896875000614518747, 6.054752690667223547, 3.707466751127219781E-16 ) ) ;
#6488 = CARTESIAN_POINT ( 'NONE',  ( 6.590625000614518392, -3.027376345333610441, -5.243569643749999898 ) ) ;
#6489 = CARTESIAN_POINT ( 'NONE',  ( 45.00000000000000000, 6.123233995736764310E-16, -4.999999999999998224 ) ) ;
#6490 = CARTESIAN_POINT ( 'NONE',  ( 23.79375000122903216, -2.886751345948129988, 4.999999999999997335 ) ) ;
#6491 = CARTESIAN_POINT ( 'NONE',  ( 16.54687500061451644, -3.027376345333610441, -5.243569643749999898 ) ) ;
#6492 = CARTESIAN_POINT ( 'NONE',  ( -1.071796769724488563, 11.65490381179670010, 34.00000000000000000 ) ) ;
#6493 = ORIENTED_EDGE ( 'NONE', *, *, #62104, .F. ) ;
#6494 = CARTESIAN_POINT ( 'NONE',  ( 23.50312500061451360, 0.000000000000000000, 5.243569643749999010 ) ) ;
#6495 = CARTESIAN_POINT ( 'NONE',  ( 10.45312500061451644, 0.000000000000000000, 5.243569643749999010 ) ) ;
#6496 = CARTESIAN_POINT ( 'NONE',  ( 27.83437500061451786, 6.421520780324663323E-16, -5.243569643749999010 ) ) ;
#6497 = CARTESIAN_POINT ( 'NONE',  ( 10.07812500061451644, -4.541064518000419881, 2.621784821874995952 ) ) ;
#6498 = CARTESIAN_POINT ( 'NONE',  ( 25.40625000122903288, 4.330127018922192761, -2.499999999999997780 ) ) ;
#6499 = ADVANCED_FACE ( 'NONE', ( #5853 ), #22472, .F. ) ;
#6500 = CARTESIAN_POINT ( 'NONE',  ( 11.92500000122903181, 2.886751345948129099, -4.999999999999998224 ) ) ;
#6501 = CARTESIAN_POINT ( 'NONE',  ( 27.40312500061451573, 4.541064518000418104, -2.621784821874998173 ) ) ;
#6502 = CARTESIAN_POINT ( 'NONE',  ( 4.243569643749999898, 12.79062500061451679, -27.54997392385601529 ) ) ;
#6503 = CARTESIAN_POINT ( 'NONE',  ( 12.63750000122903394, -4.330127018922194537, 2.499999999999995559 ) ) ;
#6504 = AXIS2_PLACEMENT_3D ( 'NONE', #54407, #65850, #43691 ) ;
#6505 = CARTESIAN_POINT ( 'NONE',  ( 10.72500000000000142, -4.330127018922194537, 2.499999999999995559 ) ) ;
#6506 = CARTESIAN_POINT ( 'NONE',  ( 20.12812500061451715, 6.421520780324663323E-16, -5.243569643749999010 ) ) ;
#6507 = CARTESIAN_POINT ( 'NONE',  ( 29.59687500061451715, -2.746126346562642428, -4.756430356249999214 ) ) ;
#6508 = CARTESIAN_POINT ( 'NONE',  ( 21.30000000000000071, 4.330127018922192761, -2.499999999999997780 ) ) ;
#6509 = CARTESIAN_POINT ( 'NONE',  ( 6.712500001229034119, 0.000000000000000000, 4.999999999999998224 ) ) ;
#6510 = CARTESIAN_POINT ( 'NONE',  ( 15.30000000122903359, -2.886751345948129988, 4.999999999999997335 ) ) ;
#6511 = AXIS2_PLACEMENT_3D ( 'NONE', #53416, #31244, #64123 ) ;
#6512 = CARTESIAN_POINT ( 'NONE',  ( 12.85312500061451502, -4.541064518000417216, -2.621784821875001281 ) ) ;
#6513 = CARTESIAN_POINT ( 'NONE',  ( 15.85312500061451857, 0.000000000000000000, 5.243569643749999010 ) ) ;
#6514 = AXIS2_PLACEMENT_3D ( 'NONE', #1050, #6585, #34643 ) ;
#6515 = CARTESIAN_POINT ( 'NONE',  ( 25.83750000122903501, 6.123233995736764310E-16, -4.999999999999998224 ) ) ;
#6516 = CARTESIAN_POINT ( 'NONE',  ( 20.21250000000000213, -5.773502691896255534, -1.060575238724906372E-15 ) ) ;
#6517 = CARTESIAN_POINT ( 'NONE',  ( 24.45937500061451786, 0.000000000000000000, 5.243569643749999010 ) ) ;
#6518 = DIRECTION ( 'NONE',  ( -1.000000000000000000, -0.000000000000000000, -0.000000000000000000 ) ) ;
#6519 = CARTESIAN_POINT ( 'NONE',  ( 9.037500001229034297, -4.330127018922194537, 2.499999999999995559 ) ) ;
#6520 = CARTESIAN_POINT ( 'NONE',  ( 8.971875000614515372, 3.027376345333613106, -5.243569643749998122 ) ) ;
#6521 = CARTESIAN_POINT ( 'NONE',  ( 24.75937500061451502, 4.541064518000418104, -2.621784821874998173 ) ) ;
#6522 =( BOUNDED_CURVE ( )  B_SPLINE_CURVE ( 2, ( #42640, #60344, #21930, #31924, #66269, #61452, #16379, #48553, #71821 ),
 .UNSPECIFIED., .F., .F. ) 
 B_SPLINE_CURVE_WITH_KNOTS ( ( 3, 2, 2, 2, 3 ),
 ( 0.01086956521739130578, 0.01449275362318840597, 0.02173913043478260809, 0.02898550724637680848, 0.03260869565217391908 ),
 .UNSPECIFIED. ) 
 CURVE ( )  GEOMETRIC_REPRESENTATION_ITEM ( )  RATIONAL_B_SPLINE_CURVE ( ( 0.9330127018922194093, 0.9330127018922194093, 1.000000000000000000, 0.8660254037844387076, 1.000000000000000000, 0.8660254037844387076, 1.000000000000000000, 0.9330127018922191873, 0.9330127018922192983 ) ) 
 REPRESENTATION_ITEM ( '' )  );
#6523 = CYLINDRICAL_SURFACE ( 'NONE', #23233, 4.999999999999998224 ) ;
#6524 = CARTESIAN_POINT ( 'NONE',  ( 23.12812500061451360, -4.541064518000419881, 2.621784821874995952 ) ) ;
#6525 = CARTESIAN_POINT ( 'NONE',  ( 27.34687500061451360, -3.027376345333610441, -5.243569643749999898 ) ) ;
#6526 = CARTESIAN_POINT ( 'NONE',  ( -3.756430356249999214, 17.44062499938548072, 27.83122392262697176 ) ) ;
#6527 = CARTESIAN_POINT ( 'NONE',  ( 17.92500000000000071, -4.330127018922194537, 2.499999999999995559 ) ) ;
#6528 = CARTESIAN_POINT ( 'NONE',  ( 8.371875000614515727, -6.054752690667223547, -1.112240025338166033E-15 ) ) ;
#6529 = CARTESIAN_POINT ( 'NONE',  ( 5.000000000000945022, -0.1513208456332415797, 5.148249888508871663 ) ) ;
#6530 = CARTESIAN_POINT ( 'NONE',  ( 26.72812500061451502, -4.541064518000419881, 2.621784821874995952 ) ) ;
#6531 = CARTESIAN_POINT ( 'NONE',  ( 5.446875000614518569, 6.054752690667223547, 3.707466751127219781E-16 ) ) ;
#6532 = CARTESIAN_POINT ( 'NONE',  ( 3.160880256176461511, -3.874123901750303300, -3.160880256176591185 ) ) ;
#6533 = CARTESIAN_POINT ( 'NONE',  ( -4.243569643749999898, 10.35312500061459673, 30.00000000000000000 ) ) ;
#6534 = CARTESIAN_POINT ( 'NONE',  ( 15.97499999999999964, 4.330127018922191873, 2.499999999999999556 ) ) ;
#6535 = ORIENTED_EDGE ( 'NONE', *, *, #67586, .T. ) ;
#6536 = CARTESIAN_POINT ( 'NONE',  ( 28.12499999999999645, 4.330127018922191873, 2.499999999999999556 ) ) ;
#6537 = CARTESIAN_POINT ( 'NONE',  ( 29.55937500061451573, -4.541064518000417216, -2.621784821875001281 ) ) ;
#6538 = ORIENTED_EDGE ( 'NONE', *, *, #14507, .F. ) ;
#6539 = CARTESIAN_POINT ( 'NONE',  ( 15.02812500061451750, -4.541064518000419881, 2.621784821874995952 ) ) ;
#6540 = CARTESIAN_POINT ( 'NONE',  ( 5.765625000614519102, 3.027376345333613106, -5.243569643749998122 ) ) ;
#6541 = CARTESIAN_POINT ( 'NONE',  ( 20.03437500061451715, -2.746126346562642428, -4.756430356249999214 ) ) ;
#6542 = CARTESIAN_POINT ( 'NONE',  ( 4.434375000614519280, 6.421520780324663323E-16, -5.243569643749999010 ) ) ;
#6543 = CARTESIAN_POINT ( 'NONE',  ( 14.85000000122903252, -2.886751345948129988, 4.999999999999997335 ) ) ;
#6544 = CARTESIAN_POINT ( 'NONE',  ( 21.44999999999999929, 0.000000000000000000, 4.999999999999998224 ) ) ;
#6545 = CARTESIAN_POINT ( 'NONE',  ( 29.62500000000000000, -4.330127018922194537, 2.499999999999995559 ) ) ;
#6546 = CARTESIAN_POINT ( 'NONE',  ( 4.959375000614516971, 4.541064518000418104, -2.621784821874998173 ) ) ;
#6547 = CARTESIAN_POINT ( 'NONE',  ( 8.709375000614517859, 0.000000000000000000, 5.243569643749999010 ) ) ;
#6548 = CARTESIAN_POINT ( 'NONE',  ( 22.62187500061451573, 3.027376345333611329, 5.243569643749999010 ) ) ;
#6549 = ADVANCED_FACE ( 'NONE', ( #11032 ), #28743, .F. ) ;
#6550 = CARTESIAN_POINT ( 'NONE',  ( 17.17500000000000071, 6.123233995736764310E-16, -4.999999999999998224 ) ) ;
#6551 = ORIENTED_EDGE ( 'NONE', *, *, #19199, .T. ) ;
#6552 = CARTESIAN_POINT ( 'NONE',  ( 4.021875000614516082, 3.027376345333613106, -5.243569643749998122 ) ) ;
#6553 = CARTESIAN_POINT ( 'NONE',  ( 6.337499999999998579, -2.886751345948125991, -5.000000000000000000 ) ) ;
#6554 = VECTOR ( 'NONE', #68710, 1000.000000000000000 ) ;
#6555 = CARTESIAN_POINT ( 'NONE',  ( 6.684375000614518392, 6.421520780324663323E-16, -5.243569643749999010 ) ) ;
#6556 = CARTESIAN_POINT ( 'NONE',  ( 17.62500000000000000, 6.123233995736764310E-16, -4.999999999999998224 ) ) ;
#6557 = CARTESIAN_POINT ( 'NONE',  ( 15.89062500061451289, -3.027376345333614438, 5.243569643749998122 ) ) ;
#6558 = CARTESIAN_POINT ( 'NONE',  ( -8.484601909799255319E-16, 20.03750000000000142, 34.61880215351700940 ) ) ;
#6559 = CARTESIAN_POINT ( 'NONE',  ( 4.194367172679521083, 2.721727781396576784, 4.432111563841672819 ) ) ;
#6560 = CARTESIAN_POINT ( 'NONE',  ( 18.83437500061451431, 5.824947211148865298E-16, -4.756430356249998326 ) ) ;
#6561 = CARTESIAN_POINT ( 'NONE',  ( 9.553125000614517859, 0.000000000000000000, 5.243569643749999010 ) ) ;
#6562 = CARTESIAN_POINT ( 'NONE',  ( 25.99687500061451928, -3.027376345333610441, -5.243569643749999898 ) ) ;
#6563 = CARTESIAN_POINT ( 'NONE',  ( 65.00000000000000000, 0.000000000000000000, 0.000000000000000000 ) ) ;
#6564 = CARTESIAN_POINT ( 'NONE',  ( 26.55937500061451573, 4.541064518000418104, -2.621784821874998173 ) ) ;
#6565 = CARTESIAN_POINT ( 'NONE',  ( 8.699999999999999289, 4.330127018922192761, -2.499999999999997780 ) ) ;
#6566 = CARTESIAN_POINT ( 'NONE',  ( -1.999999999999997113, 13.88750000122903394, 33.46410161513775705 ) ) ;
#6567 = CARTESIAN_POINT ( 'NONE',  ( 7.837500001229035007, 6.123233995736764310E-16, -4.999999999999998224 ) ) ;
#6568 = AXIS2_PLACEMENT_3D ( 'NONE', #2542, #46885, #63855 ) ;
#6569 = CARTESIAN_POINT ( 'NONE',  ( 17.37187500061451573, -6.054752690667223547, -1.112240025338166033E-15 ) ) ;
#6570 = CARTESIAN_POINT ( 'NONE',  ( 12.08437500061451608, 6.421520780324663323E-16, -5.243569643749999010 ) ) ;
#6571 = CARTESIAN_POINT ( 'NONE',  ( -3.992949912593975359, 3.009468837316803924, -30.27463465970910406 ) ) ;
#6572 = EDGE_LOOP ( 'NONE', ( #66325, #19695, #30020, #7543 ) ) ;
#6573 = CARTESIAN_POINT ( 'NONE',  ( 14.84062500061451750, 6.054752690667223547, 3.707466751127219781E-16 ) ) ;
#6574 = AXIS2_PLACEMENT_3D ( 'NONE', #30059, #53319, #2354 ) ;
#6575 = CARTESIAN_POINT ( 'NONE',  ( 25.61250000122903359, 0.000000000000000000, 4.999999999999998224 ) ) ;
#6576 = CARTESIAN_POINT ( 'NONE',  ( 12.57187500061451857, 3.027376345333613106, -5.243569643749998122 ) ) ;
#6577 = CARTESIAN_POINT ( 'NONE',  ( 3.999999999999998668, 12.72500000122903430, 27.69059892324149530 ) ) ;
#6578 = CARTESIAN_POINT ( 'NONE',  ( 13.71562500061451750, -6.054752690667223547, -1.112240025338166033E-15 ) ) ;
#6579 = CARTESIAN_POINT ( 'NONE',  ( 26.36250000122903003, 4.330127018922192761, -2.499999999999997780 ) ) ;
#6580 = CARTESIAN_POINT ( 'NONE',  ( 26.14687500061451431, 6.054752690667223547, 3.707466751127219781E-16 ) ) ;
#6581 = CARTESIAN_POINT ( 'NONE',  ( 5.190092854996874117, 9.698896338944486217, 24.77581305162949832 ) ) ;
#6582 =( BOUNDED_CURVE ( )  B_SPLINE_CURVE ( 2, ( #57205, #63483, #57572, #56493, #22506, #50955, #35403 ),
 .UNSPECIFIED., .F., .F. ) 
 B_SPLINE_CURVE_WITH_KNOTS ( ( 3, 2, 2, 3 ),
 ( 0.2300000000000000100, 0.2333333333333333370, 0.2366666666666666363, 0.2399999999999999634 ),
 .UNSPECIFIED. ) 
 CURVE ( )  GEOMETRIC_REPRESENTATION_ITEM ( )  RATIONAL_B_SPLINE_CURVE ( ( 1.000000000000000000, 0.8660254037844387076, 1.000000000000000000, 0.8660254037844387076, 1.000000000000000000, 0.8660254037844398178, 0.9999999999999988898 ) ) 
 REPRESENTATION_ITEM ( '' )  );
#6583 = CARTESIAN_POINT ( 'NONE',  ( 12.15000000122903501, -2.886751345948129988, 4.999999999999997335 ) ) ;
#6584 = FACE_OUTER_BOUND ( 'NONE', #47893, .T. ) ;
#6585 = DIRECTION ( 'NONE',  ( 1.000000000000000000, 0.000000000000000000, 0.000000000000000000 ) ) ;
#6586 = CARTESIAN_POINT ( 'NONE',  ( 4.243569643749999898, 17.34687500061451715, -27.54997392385601529 ) ) ;
#6587 = CARTESIAN_POINT ( 'NONE',  ( 18.30937500061451928, -4.541064518000417216, -2.621784821875001281 ) ) ;
#6588 = CARTESIAN_POINT ( 'NONE',  ( 19.61250000122903359, 4.330127018922192761, -2.499999999999997780 ) ) ;
#6589 =( BOUNDED_CURVE ( )  B_SPLINE_CURVE ( 2, ( #22167, #45073, #61684, #55431, #21430, #49888, #43987, #62057, #16975 ),
 .UNSPECIFIED., .F., .F. ) 
 B_SPLINE_CURVE_WITH_KNOTS ( ( 3, 2, 2, 2, 3 ),
 ( 0.8152173913043478937, 0.8188405797101449002, 0.8260869565217391353, 0.8333333333333333703, 0.8369565217391304879 ),
 .UNSPECIFIED. ) 
 CURVE ( )  GEOMETRIC_REPRESENTATION_ITEM ( )  RATIONAL_B_SPLINE_CURVE ( ( 0.9330127018922192983, 0.9330127018922202975, 1.000000000000000000, 0.8660254037844387076, 1.000000000000000000, 0.8660254037844387076, 1.000000000000000000, 0.9330127018922182991, 0.9330127018922192983 ) ) 
 REPRESENTATION_ITEM ( '' )  );
#6590 = CARTESIAN_POINT ( 'NONE',  ( 14.63437500061451679, -4.541064518000419881, 2.621784821874995952 ) ) ;
#6591 = FACE_OUTER_BOUND ( 'NONE', #59994, .T. ) ;
#6592 = CARTESIAN_POINT ( 'NONE',  ( 22.31250000122903288, 4.330127018922192761, -2.499999999999997780 ) ) ;
#6593 = CARTESIAN_POINT ( 'NONE',  ( 15.85312500061451857, 0.000000000000000000, 5.243569643749999010 ) ) ;
#6594 = CARTESIAN_POINT ( 'NONE',  ( 29.72812500061451502, 4.541064518000418104, 2.621784821874999949 ) ) ;
#6595 = ORIENTED_EDGE ( 'NONE', *, *, #39975, .F. ) ;
#6596 = ORIENTED_EDGE ( 'NONE', *, *, #38656, .F. ) ;
#6597 = CARTESIAN_POINT ( 'NONE',  ( 17.39999999999999858, 0.000000000000000000, 4.999999999999998224 ) ) ;
#6598 = CARTESIAN_POINT ( 'NONE',  ( 0.000000000000000000, 27.50000000000000000, 30.00000000000000000 ) ) ;
#6599 = CARTESIAN_POINT ( 'NONE',  ( 3.103125000614517237, 4.541064518000418104, -2.621784821874998173 ) ) ;
#6600 = CARTESIAN_POINT ( 'NONE',  ( 14.62500000122903288, 2.886751345948129099, -4.999999999999998224 ) ) ;
#6601 = CARTESIAN_POINT ( 'NONE',  ( 20.72812500061451502, 4.541064518000418104, 2.621784821874999949 ) ) ;
#6602 = CARTESIAN_POINT ( 'NONE',  ( 23.99062500061451786, -3.027376345333614438, 5.243569643749998122 ) ) ;
#6603 = CARTESIAN_POINT ( 'NONE',  ( 2.803125000614518747, 0.000000000000000000, 5.243569643749999010 ) ) ;
#6604 =( BOUNDED_CURVE ( )  B_SPLINE_CURVE ( 2, ( #56693, #57049, #52244, #68161, #68517, #12712, #18234 ),
 .UNSPECIFIED., .F., .F. ) 
 B_SPLINE_CURVE_WITH_KNOTS ( ( 3, 2, 2, 3 ),
 ( 0.7666666666666668295, 0.7694444444444445974, 0.7722222222222223653, 0.7750000000000001332 ),
 .UNSPECIFIED. ) 
 CURVE ( )  GEOMETRIC_REPRESENTATION_ITEM ( )  RATIONAL_B_SPLINE_CURVE ( ( 0.9999999999999946709, 0.8660254037844440367, 1.000000000000000000, 0.8660254037844387076, 1.000000000000000000, 0.8660254037844333785, 1.000000000000005329 ) ) 
 REPRESENTATION_ITEM ( '' )  );
#6605 = CARTESIAN_POINT ( 'NONE',  ( 27.37500000000000000, -4.330127018922194537, 2.499999999999995559 ) ) ;
#6606 = CARTESIAN_POINT ( 'NONE',  ( 4.575260086717170438, 2.016679235498957112, 4.840250765194281435 ) ) ;
#6607 = AXIS2_PLACEMENT_3D ( 'NONE', #16146, #42772, #72305 ) ;
#6608 = CARTESIAN_POINT ( 'NONE',  ( 9.234375000614518214, -4.119189519843968306, 2.378215178124996054 ) ) ;
#6609 = LINE ( 'NONE', #29137, #5242 ) ;
#6610 = CARTESIAN_POINT ( 'NONE',  ( 3.999999999999999112, 11.33750000122903501, -30.00000000000000000 ) ) ;
#6611 = CARTESIAN_POINT ( 'NONE',  ( -4.243569643749997233, 15.84687500061451715, -27.54997392385601174 ) ) ;
#6612 = CARTESIAN_POINT ( 'NONE',  ( 6.487500001229034474, 6.123233995736764310E-16, -4.999999999999998224 ) ) ;
#6613 = CARTESIAN_POINT ( 'NONE',  ( 9.187500000000001776, 5.773502691896255534, 3.535250795749688894E-16 ) ) ;
#6614 = EDGE_CURVE ( 'NONE', #65643, #53042, #685, .T. ) ;
#6615 = CARTESIAN_POINT ( 'NONE',  ( 4.987500001229032698, -4.330127018922194537, 2.499999999999995559 ) ) ;
#6616 = CARTESIAN_POINT ( 'NONE',  ( 9.609375000614518214, 0.000000000000000000, 5.243569643749999010 ) ) ;
#6617 = FACE_OUTER_BOUND ( 'NONE', #71782, .T. ) ;
#6618 = CARTESIAN_POINT ( 'NONE',  ( 3.121875000614518836, 3.027376345333613106, -5.243569643749998122 ) ) ;
#6619 = CARTESIAN_POINT ( 'NONE',  ( 28.01249999999999929, 2.886751345948146419, -4.999999999999968914 ) ) ;
#6620 = CARTESIAN_POINT ( 'NONE',  ( 7.320879633048903241E-15, 18.53750000000000142, -34.00000000000000000 ) ) ;
#6621 = CARTESIAN_POINT ( 'NONE',  ( 7.471875000614519813, -6.054752690667223547, -1.112240025338166033E-15 ) ) ;
#6622 = CARTESIAN_POINT ( 'NONE',  ( 12.60937500061451821, 4.541064518000418104, -2.621784821874998173 ) ) ;
#6623 = CARTESIAN_POINT ( 'NONE',  ( 6.075000001229034829, 2.886751345948129099, -4.999999999999997335 ) ) ;
#6624 = CARTESIAN_POINT ( 'NONE',  ( 6.450000000000001066, 4.330127018922192761, -2.499999999999997780 ) ) ;
#6625 = CARTESIAN_POINT ( 'NONE',  ( -4.243569643749999898, 16.20312500061459815, 30.00000000000000000 ) ) ;
#6626 = CARTESIAN_POINT ( 'NONE',  ( 22.35937500061451644, -4.541064518000417216, -2.621784821875001281 ) ) ;
#6627 = DIRECTION ( 'NONE',  ( -0.000000000000000000, -1.000000000000000000, -0.000000000000000000 ) ) ;
#6628 = CARTESIAN_POINT ( 'NONE',  ( 25.83750000122903501, 6.123233995736764310E-16, -4.999999999999998224 ) ) ;
#6629 = CARTESIAN_POINT ( 'NONE',  ( 17.22187500061451360, -4.119189519843968306, 2.378215178124996054 ) ) ;
#6630 = CARTESIAN_POINT ( 'NONE',  ( 21.81562500061451004, -6.054752690667223547, -1.112240025338166033E-15 ) ) ;
#6631 = CARTESIAN_POINT ( 'NONE',  ( 15.74062500061451608, 6.054752690667223547, 3.707466751127219781E-16 ) ) ;
#6632 = CARTESIAN_POINT ( 'NONE',  ( 26.74687500061451573, -4.119189519843965641, -2.378215178125001383 ) ) ;
#6633 = CARTESIAN_POINT ( 'NONE',  ( 11.89687500061451608, -3.027376345333614438, 5.243569643749998122 ) ) ;
#6634 = CARTESIAN_POINT ( 'NONE',  ( 29.02499999999999858, 4.330127018922191873, 2.499999999999999556 ) ) ;
#6635 = CARTESIAN_POINT ( 'NONE',  ( 22.68750000122903288, 6.123233995736764310E-16, -4.999999999999998224 ) ) ;
#6636 = FACE_OUTER_BOUND ( 'NONE', #28702, .T. ) ;
#6637 = CARTESIAN_POINT ( 'NONE',  ( 11.44687500061451857, -3.027376345333614438, 5.243569643749998122 ) ) ;
#6638 = CARTESIAN_POINT ( 'NONE',  ( 29.18437500061451573, 6.421520780324663323E-16, -5.243569643749999010 ) ) ;
#6639 = ADVANCED_FACE ( 'NONE', ( #61630 ), #22829, .F. ) ;
#6640 = CARTESIAN_POINT ( 'NONE',  ( 28.06875000122903074, 2.886751345948129099, -4.999999999999997335 ) ) ;
#6641 = CARTESIAN_POINT ( 'NONE',  ( 45.00000000000000000, 0.000000000000000000, 0.000000000000000000 ) ) ;
#6642 = CARTESIAN_POINT ( 'NONE',  ( 21.98437500061451644, 6.421520780324663323E-16, -5.243569643749999010 ) ) ;
#6643 = CARTESIAN_POINT ( 'NONE',  ( 13.20937500061451786, 0.000000000000000000, 5.243569643749999010 ) ) ;
#6644 = CARTESIAN_POINT ( 'NONE',  ( -3.756430356250000102, 18.37812499938548427, 30.00000000000000000 ) ) ;
#6645 = CARTESIAN_POINT ( 'NONE',  ( 25.38749999999999929, 5.773502691896255534, 3.535250795749688894E-16 ) ) ;
#6646 = CARTESIAN_POINT ( 'NONE',  ( 4.000000000000000000, 13.40000000000000036, 30.00000000000000000 ) ) ;
#6647 = CARTESIAN_POINT ( 'NONE',  ( 28.24687500061451573, -2.746126346562642428, -4.756430356249999214 ) ) ;
#6648 = CARTESIAN_POINT ( 'NONE',  ( 17.24062500061451786, -3.027376345333614438, 5.243569643749998122 ) ) ;
#6649 = CARTESIAN_POINT ( 'NONE',  ( 7.724999999999999645, 6.123233995736764310E-16, -4.999999999999998224 ) ) ;
#6650 = CARTESIAN_POINT ( 'NONE',  ( 15.67500000000000071, -4.330127018922194537, 2.499999999999995559 ) ) ;
#6651 = CARTESIAN_POINT ( 'NONE',  ( -3.999999999999999556, 19.62500000122903643, 27.69059892324149530 ) ) ;
#6652 = CARTESIAN_POINT ( 'NONE',  ( 45.00000000000000000, 0.000000000000000000, 4.999999999999998224 ) ) ;
#6653 = CARTESIAN_POINT ( 'NONE',  ( 26.29687500061451644, -3.027376345333614438, 5.243569643749998122 ) ) ;
#6654 = EDGE_LOOP ( 'NONE', ( #64634, #28623, #38613, #16531 ) ) ;
#6655 = CARTESIAN_POINT ( 'NONE',  ( 22.26562500061451644, -6.054752690667223547, -1.112240025338166033E-15 ) ) ;
#6656 = CARTESIAN_POINT ( 'NONE',  ( 20.25937500061451857, 4.541064518000418104, -2.621784821874998173 ) ) ;
#6657 = CARTESIAN_POINT ( 'NONE',  ( 3.600000000000002309, -4.330127018922190985, -2.500000000000001332 ) ) ;
#6658 = CARTESIAN_POINT ( 'NONE',  ( 7.190625000614518036, 6.054752690667223547, 3.707466751127219781E-16 ) ) ;
#6659 = CARTESIAN_POINT ( 'NONE',  ( 21.51562500061451644, 3.027376345333613106, -5.243569643749998122 ) ) ;
#6660 = CARTESIAN_POINT ( 'NONE',  ( 11.70937500061451608, 4.541064518000418104, -2.621784821874998173 ) ) ;
#6661 = CARTESIAN_POINT ( 'NONE',  ( 17.33437500061451431, -4.541064518000419881, 2.621784821874995952 ) ) ;
#6662 = CARTESIAN_POINT ( 'NONE',  ( 4.243569643749999898, 17.32812500061451644, 30.00000000000000000 ) ) ;
#6663 = EDGE_CURVE ( 'NONE', #10265, #9450, #39476, .T. ) ;
#6664 = CARTESIAN_POINT ( 'NONE',  ( 20.02500000122903145, 2.886751345948129099, -4.999999999999998224 ) ) ;
#6665 = CARTESIAN_POINT ( 'NONE',  ( 14.78437500061451715, 5.824947211148865298E-16, -4.756430356249998326 ) ) ;
#6666 = CARTESIAN_POINT ( 'NONE',  ( 10.15312500061451750, -4.541064518000417216, -2.621784821875001281 ) ) ;
#6667 = CARTESIAN_POINT ( 'NONE',  ( 6.196875000614515905, -3.027376345333610441, -5.243569643749999898 ) ) ;
#6668 = CARTESIAN_POINT ( 'NONE',  ( 4.884375000614518569, 6.421520780324663323E-16, -5.243569643749999010 ) ) ;
#6669 = CARTESIAN_POINT ( 'NONE',  ( 26.18437500061451573, 4.541064518000418104, 2.621784821874999949 ) ) ;
#6670 = CARTESIAN_POINT ( 'NONE',  ( 16.22812500061451857, 4.541064518000418104, 2.621784821874999949 ) ) ;
#6671 = CARTESIAN_POINT ( 'NONE',  ( 27.60000000122903430, -2.886751345948125991, -5.000000000000000000 ) ) ;
#6672 = CARTESIAN_POINT ( 'NONE',  ( 25.22812500061451502, 4.541064518000418104, 2.621784821874999949 ) ) ;
#6673 = CARTESIAN_POINT ( 'NONE',  ( 21.53437500061451715, 6.421520780324663323E-16, -5.243569643749999010 ) ) ;
#6674 = CARTESIAN_POINT ( 'NONE',  ( 18.36562500061451431, 3.027376345333613106, -5.243569643749998122 ) ) ;
#6675 = CARTESIAN_POINT ( 'NONE',  ( -3.000416591977282496E-16, 16.59687500061452070, 25.09994784771203058 ) ) ;
#6676 = CARTESIAN_POINT ( 'NONE',  ( 22.82812500061451644, 6.421520780324663323E-16, -5.243569643749999010 ) ) ;
#6677 = CARTESIAN_POINT ( 'NONE',  ( 0.000000000000000000, 20.00000000000000000, -33.99999999999999289 ) ) ;
#6678 = ORIENTED_EDGE ( 'NONE', *, *, #40891, .T. ) ;
#6679 = CARTESIAN_POINT ( 'NONE',  ( 25.42500000000000071, 4.330127018922191873, 2.499999999999999556 ) ) ;
#6680 = CARTESIAN_POINT ( 'NONE',  ( -2.828200636599751609E-16, 13.58750000000000213, -34.61880215351700230 ) ) ;
#6681 = CARTESIAN_POINT ( 'NONE',  ( 1.878215178125000495, 19.12812499938548427, 26.74683588394047007 ) ) ;
#6682 = CARTESIAN_POINT ( 'NONE',  ( 28.94062500061452070, -3.027376345333614438, 5.243569643749998122 ) ) ;
#6683 = CARTESIAN_POINT ( 'NONE',  ( 9.215625000614515727, -6.054752690667223547, -1.112240025338166033E-15 ) ) ;
#6684 = CARTESIAN_POINT ( 'NONE',  ( 21.48750000122903003, 4.330127018922191873, 2.499999999999999556 ) ) ;
#6685 = CARTESIAN_POINT ( 'NONE',  ( 27.89062500061451289, 6.054752690667223547, 3.707466751127219781E-16 ) ) ;
#6686 = CARTESIAN_POINT ( 'NONE',  ( 26.81250000000000000, 2.886751345948126879, 4.999999999999999112 ) ) ;
#6687 = CARTESIAN_POINT ( 'NONE',  ( -3.999999999999999556, 17.82500000122903572, -32.30940107675850470 ) ) ;
#6688 = CARTESIAN_POINT ( 'NONE',  ( 29.80312500061451431, 0.000000000000000000, 5.243569643749999010 ) ) ;
#6689 = CARTESIAN_POINT ( 'NONE',  ( 10.22812500061451679, 6.421520780324663323E-16, -5.243569643749999010 ) ) ;
#6690 = ORIENTED_EDGE ( 'NONE', *, *, #68921, .T. ) ;
#6691 = CARTESIAN_POINT ( 'NONE',  ( 7.490625000614516082, -3.027376345333610441, -5.243569643749999898 ) ) ;
#6692 = CARTESIAN_POINT ( 'NONE',  ( 6.965625000614518392, -6.054752690667223547, -1.112240025338166033E-15 ) ) ;
#6693 = VECTOR ( 'NONE', #67358, 1000.000000000000000 ) ;
#6694 = CARTESIAN_POINT ( 'NONE',  ( 16.50937500061451502, -4.119189519843965641, -2.378215178125001383 ) ) ;
#6695 = CARTESIAN_POINT ( 'NONE',  ( 4.676989713315623298, -1.768073502771440486, 4.936522198724768273 ) ) ;
#6696 = CARTESIAN_POINT ( 'NONE',  ( 14.40000000000000036, -4.330127018922190985, -2.500000000000001332 ) ) ;
#6697 = CARTESIAN_POINT ( 'NONE',  ( 16.65937500061452070, 4.541064518000418104, -2.621784821874998173 ) ) ;
#6698 = CARTESIAN_POINT ( 'NONE',  ( 11.96250000122903501, 4.330127018922192761, -2.499999999999997780 ) ) ;
#6699 = CARTESIAN_POINT ( 'NONE',  ( 16.65937500061452070, 4.541064518000418104, -2.621784821874998173 ) ) ;
#6700 = CARTESIAN_POINT ( 'NONE',  ( 17.81250000000000355, 2.886751345948126879, 4.999999999999999112 ) ) ;
#6701 = CARTESIAN_POINT ( 'NONE',  ( 20.33437500061451786, 4.541064518000418104, 2.621784821874999949 ) ) ;
#6702 = CARTESIAN_POINT ( 'NONE',  ( 4.243569643749999898, 13.69062500061451537, -27.54997392385601529 ) ) ;
#6703 = CARTESIAN_POINT ( 'NONE',  ( 1.592000809091587073E-14, 16.73750000000000071, 26.00000000000000000 ) ) ;
#6704 = CARTESIAN_POINT ( 'NONE',  ( 24.23437500061451289, 5.492252693125287522, 3.363034840372157021E-16 ) ) ;
#6705 = CARTESIAN_POINT ( 'NONE',  ( 4.000000000000000000, 15.14374999877096606, 30.00000000000000000 ) ) ;
#6706 = CARTESIAN_POINT ( 'NONE',  ( 24.17812500061451786, 6.421520780324663323E-16, -5.243569643749999010 ) ) ;
#6707 = CARTESIAN_POINT ( 'NONE',  ( 28.43437500061451573, 4.541064518000418104, 2.621784821874999949 ) ) ;
#6708 = ADVANCED_FACE ( 'NONE', ( #6584 ), #68642, .T. ) ;
#6709 = CARTESIAN_POINT ( 'NONE',  ( 23.09999999999999787, 4.330127018922192761, -2.499999999999997780 ) ) ;
#6710 = CARTESIAN_POINT ( 'NONE',  ( 7.303125000614516082, 0.000000000000000000, 5.243569643749999010 ) ) ;
#6711 = CARTESIAN_POINT ( 'NONE',  ( 25.05937500061451573, 2.746126346562645981, -4.756430356249997438 ) ) ;
#6712 = CARTESIAN_POINT ( 'NONE',  ( 19.17187500061451999, -6.054752690667223547, -1.112240025338166033E-15 ) ) ;
#6713 = CARTESIAN_POINT ( 'NONE',  ( 12.23437500061451821, -2.746126346562646425, 4.756430356249996549 ) ) ;
#6714 = CARTESIAN_POINT ( 'NONE',  ( 4.528125000614516615, 4.541064518000418104, 2.621784821874999949 ) ) ;
#6715 = CARTESIAN_POINT ( 'NONE',  ( 8.821875000614518569, -6.054752690667223547, -1.112240025338166033E-15 ) ) ;
#6716 = VERTEX_POINT ( 'NONE', #12484 ) ;
#6717 = CARTESIAN_POINT ( 'NONE',  ( 19.43437500061451928, 4.541064518000418104, 2.621784821874999949 ) ) ;
#6718 = CARTESIAN_POINT ( 'NONE',  ( 16.64999999999999858, -4.330127018922190985, -2.500000000000001332 ) ) ;
#6719 = CARTESIAN_POINT ( 'NONE',  ( 30.00000000000000000, 0.000000000000000000, 4.999999999999998224 ) ) ;
#6720 = CARTESIAN_POINT ( 'NONE',  ( 3.075000000000001510, -4.330127018922194537, 2.499999999999995559 ) ) ;
#6721 = CARTESIAN_POINT ( 'NONE',  ( 1.626862140677534273E-15, 10.21250000000000036, -26.00000000000000355 ) ) ;
#6722 = CARTESIAN_POINT ( 'NONE',  ( 15.93750000000000000, 5.773502691896255534, 3.535250795749688401E-16 ) ) ;
#6723 = ORIENTED_EDGE ( 'NONE', *, *, #26985, .F. ) ;
#6724 = CARTESIAN_POINT ( 'NONE',  ( 10.53750000000000320, 5.773502691896255534, 3.535250795749688894E-16 ) ) ;
#6725 = CARTESIAN_POINT ( 'NONE',  ( 12.57187500061451502, 4.119189519843966529, 2.378215178124999607 ) ) ;
#6726 = CARTESIAN_POINT ( 'NONE',  ( 23.27812500061451573, 6.421520780324663323E-16, -5.243569643749999010 ) ) ;
#6727 = CARTESIAN_POINT ( 'NONE',  ( 13.50000000000000178, -4.330127018922190985, -2.500000000000001332 ) ) ;
#6728 = CARTESIAN_POINT ( 'NONE',  ( 10.80000000122903536, -2.886751345948129988, 4.999999999999997335 ) ) ;
#6729 = CARTESIAN_POINT ( 'NONE',  ( 9.628125000614517148, -4.541064518000419881, 2.621784821874995952 ) ) ;
#6730 = CARTESIAN_POINT ( 'NONE',  ( 23.13749999999999929, 5.773502691896255534, 3.535250795749688894E-16 ) ) ;
#6731 = CARTESIAN_POINT ( 'NONE',  ( 20.87812500061451715, -4.541064518000419881, 2.621784821874995952 ) ) ;
#6732 = FACE_OUTER_BOUND ( 'NONE', #279, .T. ) ;
#6733 = CARTESIAN_POINT ( 'NONE',  ( 28.53750000122903074, 6.123233995736764310E-16, -4.999999999999998224 ) ) ;
#6734 = CARTESIAN_POINT ( 'NONE',  ( 3.756430356249998770, 16.20312499938548356, 32.16877607737301759 ) ) ;
#6735 = CARTESIAN_POINT ( 'NONE',  ( 6.450000000000001066, 4.330127018922192761, -2.499999999999997780 ) ) ;
#6736 = ORIENTED_EDGE ( 'NONE', *, *, #58814, .F. ) ;
#6737 = CARTESIAN_POINT ( 'NONE',  ( 22.30312500061451431, -4.541064518000417216, -2.621784821875001281 ) ) ;
#6738 = CARTESIAN_POINT ( 'NONE',  ( 28.00312500061451715, 0.000000000000000000, 5.243569643749999010 ) ) ;
#6739 = CARTESIAN_POINT ( 'NONE',  ( 26.07187500061451857, 3.027376345333613106, -5.243569643749998122 ) ) ;
#6740 = CARTESIAN_POINT ( 'NONE',  ( 18.12187500061451573, 3.027376345333611329, 5.243569643749999010 ) ) ;
#6741 = CARTESIAN_POINT ( 'NONE',  ( 14.01562500061451644, 3.027376345333611329, 5.243569643749999010 ) ) ;
#6742 = CARTESIAN_POINT ( 'NONE',  ( 11.47499999999999964, 4.330127018922191873, 2.499999999999999556 ) ) ;
#6743 = AXIS2_PLACEMENT_3D ( 'NONE', #56627, #17804, #17455 ) ;
#6744 = CARTESIAN_POINT ( 'NONE',  ( 25.95000000122903216, 5.773502691896255534, 3.535250795749688894E-16 ) ) ;
#6745 = CARTESIAN_POINT ( 'NONE',  ( 21.90937500061451715, -4.119189519843965641, -2.378215178125001383 ) ) ;
#6746 = CARTESIAN_POINT ( 'NONE',  ( 15.85312500061451857, 0.000000000000000000, 5.243569643749999010 ) ) ;
#6747 = CARTESIAN_POINT ( 'NONE',  ( -5.810221930991193690E-16, 11.45000000122903216, -34.00000000000000000 ) ) ;
#6748 = CARTESIAN_POINT ( 'NONE',  ( 3.000000001229032875, 5.773502691896255534, 3.535250795749688894E-16 ) ) ;
#6749 = CARTESIAN_POINT ( 'NONE',  ( 12.57187500061451857, 3.027376345333613106, -5.243569643749998122 ) ) ;
#6750 = CARTESIAN_POINT ( 'NONE',  ( 12.38437500061451857, -4.541064518000419881, 2.621784821874995952 ) ) ;
#6751 = CARTESIAN_POINT ( 'NONE',  ( 19.17187500061451999, -6.054752690667223547, -1.112240025338166033E-15 ) ) ;
#6752 = ORIENTED_EDGE ( 'NONE', *, *, #66773, .T. ) ;
#6753 = CARTESIAN_POINT ( 'NONE',  ( 29.47499999999999787, 4.330127018922191873, 2.499999999999999556 ) ) ;
#6754 = CARTESIAN_POINT ( 'NONE',  ( 24.44062500061451715, -3.027376345333614438, 5.243569643749998122 ) ) ;
#6755 = CARTESIAN_POINT ( 'NONE',  ( 19.39687500061451786, 6.054752690667223547, 3.707466751127219781E-16 ) ) ;
#6756 = CARTESIAN_POINT ( 'NONE',  ( 23.76562500061451644, 3.027376345333613106, -5.243569643749998122 ) ) ;
#6757 = CARTESIAN_POINT ( 'NONE',  ( -1.999999999999997113, 16.92500000000000426, 33.46410161513775705 ) ) ;
#6758 = CARTESIAN_POINT ( 'NONE',  ( 28.79062500061451502, 6.054752690667223547, 3.707466751127219781E-16 ) ) ;
#6759 = CARTESIAN_POINT ( 'NONE',  ( 10.27500000122903323, 2.886751345948126879, 4.999999999999999112 ) ) ;
#6760 = CARTESIAN_POINT ( 'NONE',  ( 6.750000001229033764, -2.886751345948129988, 4.999999999999997335 ) ) ;
#6761 = LINE ( 'NONE', #62899, #31585 ) ;
#6762 = CARTESIAN_POINT ( 'NONE',  ( 26.25000000122903288, -2.886751345948125991, -5.000000000000000000 ) ) ;
#6763 = CARTESIAN_POINT ( 'NONE',  ( 3.756430356249998770, 13.16562499938548392, 32.16877607737302469 ) ) ;
#6764 = CARTESIAN_POINT ( 'NONE',  ( 17.11875000122903145, -5.773502691896255534, -1.060575238724906372E-15 ) ) ;
#6765 = CARTESIAN_POINT ( 'NONE',  ( 8.521875000614516082, 3.027376345333613106, -5.243569643749998122 ) ) ;
#6766 = CARTESIAN_POINT ( 'NONE',  ( 34.99999999999999289, 4.500000000000001776, 5.500000000000000000 ) ) ;
#6767 = EDGE_CURVE ( 'NONE', #64526, #8633, #16230, .T. ) ;
#6768 = CARTESIAN_POINT ( 'NONE',  ( 17.35312500061451502, -4.541064518000417216, -2.621784821875001281 ) ) ;
#6769 = CARTESIAN_POINT ( 'NONE',  ( 10.43437500061451750, 4.541064518000418104, 2.621784821874999949 ) ) ;
#6770 = CARTESIAN_POINT ( 'NONE',  ( 28.35000000122903430, -2.886751345948129988, 4.999999999999997335 ) ) ;
#6771 = ADVANCED_FACE ( 'NONE', ( #25009 ), #8756, .T. ) ;
#6772 = CARTESIAN_POINT ( 'NONE',  ( 19.39687500061451786, 6.054752690667223547, 3.707466751127219781E-16 ) ) ;
#6773 = CARTESIAN_POINT ( 'NONE',  ( 7.359375000614516438, 0.000000000000000000, 5.243569643749999010 ) ) ;
#6774 = CARTESIAN_POINT ( 'NONE',  ( 3.740625000614516527, -3.027376345333614438, 5.243569643749998122 ) ) ;
#6775 = CARTESIAN_POINT ( 'NONE',  ( 13.35000000000000142, 0.000000000000000000, 4.999999999999998224 ) ) ;
#6776 = CARTESIAN_POINT ( 'NONE',  ( 7.565625000614518036, 3.027376345333613106, -5.243569643749998122 ) ) ;
#6777 = CARTESIAN_POINT ( 'NONE',  ( 17.12812500061451715, 4.541064518000418104, 2.621784821874999949 ) ) ;
#6778 = VERTEX_POINT ( 'NONE', #42015 ) ;
#6779 = CARTESIAN_POINT ( 'NONE',  ( 5.962500001229033231, -4.330127018922190985, -2.500000000000001332 ) ) ;
#6780 = CARTESIAN_POINT ( 'NONE',  ( 15.36562500061451608, 3.027376345333611329, 5.243569643749999010 ) ) ;
#6781 = CARTESIAN_POINT ( 'NONE',  ( 12.44062500061451537, -3.027376345333610441, -5.243569643749999898 ) ) ;
#6782 = CARTESIAN_POINT ( 'NONE',  ( 23.10937500061451644, 0.000000000000000000, 4.756430356249998326 ) ) ;
#6783 = CARTESIAN_POINT ( 'NONE',  ( 12.59999999999999964, -4.330127018922190985, -2.500000000000001332 ) ) ;
#6784 = CARTESIAN_POINT ( 'NONE',  ( 8.475000001229034297, 2.886751345948126879, 4.999999999999999112 ) ) ;
#6785 = CARTESIAN_POINT ( 'NONE',  ( 4.715625000614516615, -6.054752690667223547, -1.112240025338166033E-15 ) ) ;
#6786 = CARTESIAN_POINT ( 'NONE',  ( 18.22500000122903430, 2.886751345948129099, -4.999999999999998224 ) ) ;
#6787 = CARTESIAN_POINT ( 'NONE',  ( 24.71250000000000213, -5.773502691896255534, -1.060575238724906372E-15 ) ) ;
#6788 = CARTESIAN_POINT ( 'NONE',  ( 4.243569643749999010, 12.02187500061451786, -32.45002607614398471 ) ) ;
#6789 = DIRECTION ( 'NONE',  ( 1.000000000000000000, 0.000000000000000000, 0.000000000000000000 ) ) ;
#6790 = DIRECTION ( 'NONE',  ( -0.000000000000000000, -1.000000000000000000, -0.000000000000000000 ) ) ;
#6791 = CARTESIAN_POINT ( 'NONE',  ( 45.00000000000000000, 0.000000000000000000, 0.000000000000000000 ) ) ;
#6792 = CARTESIAN_POINT ( 'NONE',  ( 19.05937500061451928, 0.000000000000000000, 5.243569643749999010 ) ) ;
#6793 =( BOUNDED_CURVE ( )  B_SPLINE_CURVE ( 2, ( #10664, #39844, #16199, #55733, #33194, #50200, #67196 ),
 .UNSPECIFIED., .F., .F. ) 
 B_SPLINE_CURVE_WITH_KNOTS ( ( 3, 2, 2, 3 ),
 ( 0.4249999999999999889, 0.4277777777777777568, 0.4305555555555555802, 0.4333333333333333481 ),
 .UNSPECIFIED. ) 
 CURVE ( )  GEOMETRIC_REPRESENTATION_ITEM ( )  RATIONAL_B_SPLINE_CURVE ( ( 1.000000000000000000, 0.8660254037844387076, 1.000000000000000000, 0.8660254037844387076, 1.000000000000000000, 0.8660254037844387076, 1.000000000000000000 ) ) 
 REPRESENTATION_ITEM ( '' )  );
#6794 = CARTESIAN_POINT ( 'NONE',  ( -3.999999999999999112, 16.51250000122903216, 30.00000000000000000 ) ) ;
#6795 = CARTESIAN_POINT ( 'NONE',  ( 13.22812500061451502, -4.541064518000419881, 2.621784821874995952 ) ) ;
#6796 = CARTESIAN_POINT ( 'NONE',  ( 9.018750001229033586, -5.773502691896255534, -1.060575238724906372E-15 ) ) ;
#6797 = CARTESIAN_POINT ( 'NONE',  ( 4.898587196589411843E-16, 20.00000000000000000, -26.00000000000000000 ) ) ;
#6798 = CARTESIAN_POINT ( 'NONE',  ( 25.95937500061451431, -4.541064518000417216, -2.621784821875001281 ) ) ;
#6799 = CARTESIAN_POINT ( 'NONE',  ( 18.83437500061451786, 5.492252693125287522, 3.363034840372157021E-16 ) ) ;
#6800 = CARTESIAN_POINT ( 'NONE',  ( 12.92812500061451786, 6.421520780324663323E-16, -5.243569643749999010 ) ) ;
#6801 = CARTESIAN_POINT ( 'NONE',  ( 10.99687500061451750, -3.027376345333614438, 5.243569643749998122 ) ) ;
#6802 = VERTEX_POINT ( 'NONE', #8027 ) ;
#6803 = CARTESIAN_POINT ( 'NONE',  ( 26.84062500061451573, -3.027376345333610441, -5.243569643749999898 ) ) ;
#6804 = CARTESIAN_POINT ( 'NONE',  ( 21.47812500061451502, 6.421520780324663323E-16, -5.243569643749999010 ) ) ;
#6805 = CARTESIAN_POINT ( 'NONE',  ( 29.27812500061451573, 4.541064518000418104, 2.621784821874999949 ) ) ;
#6806 = CARTESIAN_POINT ( 'NONE',  ( -1.071796769724487453, 18.22009619066136565, 26.00000000000000000 ) ) ;
#6807 = CARTESIAN_POINT ( 'NONE',  ( 10.98750000000000071, 5.773502691896255534, 3.535250795749688894E-16 ) ) ;
#6808 = CARTESIAN_POINT ( 'NONE',  ( 18.45000000122903216, -2.886751345948129988, 4.999999999999997335 ) ) ;
#6809 = CARTESIAN_POINT ( 'NONE',  ( 23.36250000122903359, 0.000000000000000000, 4.999999999999998224 ) ) ;
#6810 = CARTESIAN_POINT ( 'NONE',  ( 11.25937500061451679, 2.746126346562643317, 4.756430356249998326 ) ) ;
#6811 = VERTEX_POINT ( 'NONE', #53090 ) ;
#6812 = CARTESIAN_POINT ( 'NONE',  ( 18.03749999999999787, -2.886751345948125991, -5.000000000000000000 ) ) ;
#6813 = CARTESIAN_POINT ( 'NONE',  ( 20.47500000000000142, 4.330127018922191873, 2.499999999999999556 ) ) ;
#6814 = CARTESIAN_POINT ( 'NONE',  ( 18.53437500061451715, 4.541064518000418104, 2.621784821874999949 ) ) ;
#6815 = CARTESIAN_POINT ( 'NONE',  ( 26.05312500061451431, 4.541064518000418104, -2.621784821874998173 ) ) ;
#6816 = EDGE_LOOP ( 'NONE', ( #69077, #71287, #68155, #926 ) ) ;
#6817 = CARTESIAN_POINT ( 'NONE',  ( 13.61250000000000071, 2.886751345948129099, -4.999999999999997335 ) ) ;
#6818 = CARTESIAN_POINT ( 'NONE',  ( 8.240625000614516082, -3.027376345333614438, 5.243569643749998122 ) ) ;
#6819 = CARTESIAN_POINT ( 'NONE',  ( 1.999999999999998668, 15.46250000122903501, 26.53589838486224650 ) ) ;
#6820 = CARTESIAN_POINT ( 'NONE',  ( 14.84999999999999964, -4.330127018922190985, -2.500000000000001332 ) ) ;
#6821 = CARTESIAN_POINT ( 'NONE',  ( 4.243569643749999898, 17.74062500061451786, 32.45002607614398471 ) ) ;
#6822 = CARTESIAN_POINT ( 'NONE',  ( 29.35312500061451502, 0.000000000000000000, 5.243569643749999010 ) ) ;
#6823 = CARTESIAN_POINT ( 'NONE',  ( 10.05000000000000071, 4.330127018922192761, -2.499999999999997780 ) ) ;
#6824 = CARTESIAN_POINT ( 'NONE',  ( -1.878215178124999163, 15.94062499938548427, 26.74683588394047007 ) ) ;
#6825 = CARTESIAN_POINT ( 'NONE',  ( 25.32187500061451857, 3.027376345333611329, 5.243569643749999010 ) ) ;
#6826 = ORIENTED_EDGE ( 'NONE', *, *, #48303, .F. ) ;
#6827 = CARTESIAN_POINT ( 'NONE',  ( 22.41562500061451502, 3.027376345333613106, -5.243569643749998122 ) ) ;
#6828 = CARTESIAN_POINT ( 'NONE',  ( 23.40937500061451715, 4.541064518000418104, -2.621784821874998173 ) ) ;
#6829 = CARTESIAN_POINT ( 'NONE',  ( -4.243569643749998122, 17.14062500061459460, -27.54997392385601174 ) ) ;
#6830 = CARTESIAN_POINT ( 'NONE',  ( 11.81250000000000000, 2.886751345948129099, -4.999999999999998224 ) ) ;
#6831 = CARTESIAN_POINT ( 'NONE',  ( 9.590625000614517504, -3.027376345333614438, 5.243569643749998122 ) ) ;
#6832 = CARTESIAN_POINT ( 'NONE',  ( 28.95937500061451431, 0.000000000000000000, 4.756430356249998326 ) ) ;
#6833 = CARTESIAN_POINT ( 'NONE',  ( 23.24062500061451786, -3.027376345333610441, -5.243569643749999898 ) ) ;
#6834 = CARTESIAN_POINT ( 'NONE',  ( 28.17187500061451289, 5.824947211148865298E-16, -4.756430356249998326 ) ) ;
#6835 = CARTESIAN_POINT ( 'NONE',  ( 13.65937500061451715, 0.000000000000000000, 4.756430356249998326 ) ) ;
#6836 = CARTESIAN_POINT ( 'NONE',  ( 19.24687500061452283, -3.027376345333610441, -5.243569643749999898 ) ) ;
#6837 = CARTESIAN_POINT ( 'NONE',  ( 4.243569643749999898, 12.39687500061451608, 32.45002607614398471 ) ) ;
#6838 = CARTESIAN_POINT ( 'NONE',  ( 18.08437500061451431, 4.541064518000418104, 2.621784821874999949 ) ) ;
#6839 = CARTESIAN_POINT ( 'NONE',  ( 26.59687500061451360, 6.054752690667223547, 3.707466751127219781E-16 ) ) ;
#6840 = CARTESIAN_POINT ( 'NONE',  ( 9.001249775931846008E-16, 17.72187500061451715, 34.90005215228797653 ) ) ;
#6841 = CARTESIAN_POINT ( 'NONE',  ( 7.415625000614516793, -6.054752690667223547, -1.112240025338166033E-15 ) ) ;
#6842 = CARTESIAN_POINT ( 'NONE',  ( 45.00000000000000000, 6.123233995736764310E-16, -4.999999999999998224 ) ) ;
#6843 = CARTESIAN_POINT ( 'NONE',  ( 3.684375000614518836, 4.541064518000418104, 2.621784821874999949 ) ) ;
#6844 = DIRECTION ( 'NONE',  ( 0.000000000000000000, 0.000000000000000000, -1.000000000000000000 ) ) ;
#6845 = CARTESIAN_POINT ( 'NONE',  ( 5.090625000614516615, -3.027376345333614438, 5.243569643749998122 ) ) ;
#6846 = CARTESIAN_POINT ( 'NONE',  ( 8.821875000614518569, -6.054752690667223547, -1.112240025338166033E-15 ) ) ;
#6847 =( NAMED_UNIT ( * ) SI_UNIT ( $, .STERADIAN. ) SOLID_ANGLE_UNIT ( ) );
#6848 = CARTESIAN_POINT ( 'NONE',  ( 15.75000000122902932, -2.886751345948129988, 4.999999999999997335 ) ) ;
#6849 = CARTESIAN_POINT ( 'NONE',  ( 5.259375000614518569, -4.541064518000417216, -2.621784821875001281 ) ) ;
#6850 = CARTESIAN_POINT ( 'NONE',  ( 7.565625000614518036, 3.027376345333613106, -5.243569643749998122 ) ) ;
#6851 = DIRECTION ( 'NONE',  ( -1.000000000000000000, -0.000000000000000000, -0.000000000000000000 ) ) ;
#6852 = CARTESIAN_POINT ( 'NONE',  ( 23.11875000122903145, 2.886751345948129099, -4.999999999999998224 ) ) ;
#6853 = CARTESIAN_POINT ( 'NONE',  ( 16.09687500061452070, -3.027376345333610441, -5.243569643749999898 ) ) ;
#6854 = DIRECTION ( 'NONE',  ( -1.000000000000000000, -0.000000000000000000, -0.000000000000000000 ) ) ;
#6855 = ORIENTED_EDGE ( 'NONE', *, *, #59537, .F. ) ;
#6856 = CARTESIAN_POINT ( 'NONE',  ( 25.22812500061451502, 4.541064518000418104, 2.621784821874999949 ) ) ;
#6857 = CARTESIAN_POINT ( 'NONE',  ( 9.478125000614515017, 4.541064518000418104, 2.621784821874999949 ) ) ;
#6858 = AXIS2_PLACEMENT_3D ( 'NONE', #13773, #36314, #58829 ) ;
#6859 = CARTESIAN_POINT ( 'NONE',  ( 26.44687500061451502, -3.027376345333610441, -5.243569643749999898 ) ) ;
#6860 = CARTESIAN_POINT ( 'NONE',  ( 9.403125000614517504, 4.541064518000418104, -2.621784821874998173 ) ) ;
#6861 = CARTESIAN_POINT ( 'NONE',  ( 4.437985916418120347, -2.303102473984535603, -4.640431841391475132 ) ) ;
#6862 = CARTESIAN_POINT ( 'NONE',  ( 10.72500000122903252, 2.886751345948126879, 4.999999999999999112 ) ) ;
#6863 = ADVANCED_FACE ( 'NONE', ( #46468 ), #36100, .F. ) ;
#6864 = CARTESIAN_POINT ( 'NONE',  ( 26.35312500061451857, -4.541064518000417216, -2.621784821875001281 ) ) ;
#6865 = CARTESIAN_POINT ( 'NONE',  ( 9.001249775931846008E-16, 11.81562500061451715, -25.09994784771203058 ) ) ;
#6866 = CARTESIAN_POINT ( 'NONE',  ( 12.03750000122903430, 4.330127018922191873, 2.499999999999999556 ) ) ;
#6867 = CARTESIAN_POINT ( 'NONE',  ( 21.40312500061451573, -4.541064518000417216, -2.621784821875001281 ) ) ;
#6868 = CARTESIAN_POINT ( 'NONE',  ( 11.06250000000000000, 2.886751345948126879, 4.999999999999999112 ) ) ;
#6869 = CARTESIAN_POINT ( 'NONE',  ( 20.95312500061451999, -4.541064518000417216, -2.621784821875001281 ) ) ;
#6870 = CARTESIAN_POINT ( 'NONE',  ( 5.634375000614519458, -4.541064518000419881, 2.621784821874995952 ) ) ;
#6871 = CARTESIAN_POINT ( 'NONE',  ( 21.22500000000000142, 6.123233995736764310E-16, -4.999999999999998224 ) ) ;
#6872 = CARTESIAN_POINT ( 'NONE',  ( 8.287500001229034297, 6.123233995736764310E-16, -4.999999999999998224 ) ) ;
#6873 = CARTESIAN_POINT ( 'NONE',  ( 16.35000000122903430, -2.886751345948125991, -5.000000000000000000 ) ) ;
#6874 = CARTESIAN_POINT ( 'NONE',  ( 13.45312500061451466, 4.541064518000418104, -2.621784821874998173 ) ) ;
#6875 = CARTESIAN_POINT ( 'NONE',  ( 15.62812500061451537, 6.421520780324663323E-16, -5.243569643749999010 ) ) ;
#6876 = CARTESIAN_POINT ( 'NONE',  ( 26.36250000122903003, 4.330127018922192761, -2.499999999999997780 ) ) ;
#6877 = CARTESIAN_POINT ( 'NONE',  ( 20.28750000000000142, -2.886751345948125991, -5.000000000000000000 ) ) ;
#6878 = CARTESIAN_POINT ( 'NONE',  ( 24.49687500061451573, -3.027376345333614438, 5.243569643749998122 ) ) ;
#6879 = LINE ( 'NONE', #30495, #35949 ) ;
#6880 = CARTESIAN_POINT ( 'NONE',  ( 10.23750000122903359, 4.330127018922191873, 2.499999999999999556 ) ) ;
#6881 = CARTESIAN_POINT ( 'NONE',  ( 8.934375000614517504, 6.421520780324663323E-16, -5.243569643749999010 ) ) ;
#6882 = CARTESIAN_POINT ( 'NONE',  ( 26.37187500061451217, -6.054752690667223547, -1.112240025338166033E-15 ) ) ;
#6883 = ADVANCED_FACE ( 'NONE', ( #70080 ), #18367, .F. ) ;
#6884 = CARTESIAN_POINT ( 'NONE',  ( 21.74062500061451431, -3.027376345333614438, 5.243569643749998122 ) ) ;
#6885 = CARTESIAN_POINT ( 'NONE',  ( 27.79687500061451999, -3.027376345333610441, -5.243569643749999898 ) ) ;
#6886 = CARTESIAN_POINT ( 'NONE',  ( 3.756430356250000102, 16.35312499938548569, 30.00000000000000000 ) ) ;
#6887 = CARTESIAN_POINT ( 'NONE',  ( 7.912499999999999645, 2.886751345948126879, 4.999999999999998224 ) ) ;
#6888 = CARTESIAN_POINT ( 'NONE',  ( 6.796875000614516438, 6.054752690667223547, 3.707466751127219781E-16 ) ) ;
#6889 = CARTESIAN_POINT ( 'NONE',  ( 19.22812500061451502, 6.421520780324663323E-16, -5.243569643749999010 ) ) ;
#6890 = ORIENTED_EDGE ( 'NONE', *, *, #55011, .F. ) ;
#6891 = DIRECTION ( 'NONE',  ( 0.000000000000000000, 0.000000000000000000, 1.000000000000000000 ) ) ;
#6892 = CARTESIAN_POINT ( 'NONE',  ( 27.55312500061451786, 0.000000000000000000, 5.243569643749999010 ) ) ;
#6893 = CARTESIAN_POINT ( 'NONE',  ( 4.059375000614519280, 4.541064518000418104, -2.621784821874998173 ) ) ;
#6894 = CARTESIAN_POINT ( 'NONE',  ( 26.39999999999999858, 0.000000000000000000, 4.999999999999998224 ) ) ;
#6895 = CARTESIAN_POINT ( 'NONE',  ( 3.972658874145789110, 3.036112888163414514, -4.275165627105516286 ) ) ;
#6896 = CARTESIAN_POINT ( 'NONE',  ( 16.72500000000000142, 6.123233995736764310E-16, -4.999999999999998224 ) ) ;
#6897 = ORIENTED_EDGE ( 'NONE', *, *, #42828, .T. ) ;
#6898 = CARTESIAN_POINT ( 'NONE',  ( 24.48749999999999716, 5.773502691896255534, 3.535250795749688894E-16 ) ) ;
#6899 = CARTESIAN_POINT ( 'NONE',  ( 26.40937500061451715, -4.541064518000417216, -2.621784821875001281 ) ) ;
#6900 = ORIENTED_EDGE ( 'NONE', *, *, #54265, .T. ) ;
#6901 = CARTESIAN_POINT ( 'NONE',  ( 14.39062500061451821, 6.054752690667223547, 3.707466751127219781E-16 ) ) ;
#6902 = CARTESIAN_POINT ( 'NONE',  ( 5.953125000614519102, 0.000000000000000000, 5.243569643749999010 ) ) ;
#6903 = CARTESIAN_POINT ( 'NONE',  ( 18.30937500061451573, 2.746126346562645981, -4.756430356249997438 ) ) ;
#6904 = CARTESIAN_POINT ( 'NONE',  ( 3.009375000614516793, -4.541064518000417216, -2.621784821875001281 ) ) ;
#6905 = CARTESIAN_POINT ( 'NONE',  ( 15.71250000122903501, 0.000000000000000000, 4.999999999999998224 ) ) ;
#6906 = CARTESIAN_POINT ( 'NONE',  ( 20.81250000000000000, 2.886751345948129099, -4.999999999999998224 ) ) ;
#6907 = CARTESIAN_POINT ( 'NONE',  ( 28.38749999999999929, -2.886751345948125991, -5.000000000000000000 ) ) ;
#6908 = CARTESIAN_POINT ( 'NONE',  ( 5.446875000614518569, 6.054752690667223547, 3.707466751127219781E-16 ) ) ;
#6909 = CARTESIAN_POINT ( 'NONE',  ( 9.759375000614516793, -4.541064518000417216, -2.621784821875001281 ) ) ;
#6910 = CARTESIAN_POINT ( 'NONE',  ( 20.48437500061451289, -4.541064518000419881, 2.621784821874995952 ) ) ;
#6911 = DIRECTION ( 'NONE',  ( 0.000000000000000000, 0.000000000000000000, 1.000000000000000000 ) ) ;
#6912 = VERTEX_POINT ( 'NONE', #64903 ) ;
#6913 = CARTESIAN_POINT ( 'NONE',  ( 4.659375000614518925, 0.000000000000000000, 5.243569643749999010 ) ) ;
#6914 = CARTESIAN_POINT ( 'NONE',  ( 6.225000000000001421, -4.330127018922194537, 2.499999999999995559 ) ) ;
#6915 = CARTESIAN_POINT ( 'NONE',  ( 5.709375000614517859, -4.541064518000417216, -2.621784821875001281 ) ) ;
#6916 = CARTESIAN_POINT ( 'NONE',  ( 19.12500000000000000, 4.330127018922191873, 2.499999999999999556 ) ) ;
#6917 = CARTESIAN_POINT ( 'NONE',  ( 16.79062500061451857, -3.027376345333614438, 5.243569643749998122 ) ) ;
#6918 = CARTESIAN_POINT ( 'NONE',  ( 4.000000000000000000, 19.25000000000000000, 30.00000000000000000 ) ) ;
#6919 = LINE ( 'NONE', #29449, #18576 ) ;
#6920 = CARTESIAN_POINT ( 'NONE',  ( 19.99687500061451573, -2.746126346562646425, 4.756430356249996549 ) ) ;
#6921 = CARTESIAN_POINT ( 'NONE',  ( 9.665625000614515017, -6.054752690667223547, -1.112240025338166033E-15 ) ) ;
#6922 = CARTESIAN_POINT ( 'NONE',  ( 26.55937500061451573, 4.541064518000418104, -2.621784821874998173 ) ) ;
#6923 = DIRECTION ( 'NONE',  ( 0.000000000000000000, 0.000000000000000000, 1.000000000000000000 ) ) ;
#6924 = CARTESIAN_POINT ( 'NONE',  ( 26.97187500061451360, 3.027376345333613106, -5.243569643749998122 ) ) ;
#6925 = CARTESIAN_POINT ( 'NONE',  ( 8.474999999999999645, -4.330127018922194537, 2.499999999999995559 ) ) ;
#6926 = CARTESIAN_POINT ( 'NONE',  ( 2.000000000000001332, 12.16250000122903430, 33.46410161513774995 ) ) ;
#6927 = CARTESIAN_POINT ( 'NONE',  ( 15.51562500061451644, -6.054752690667223547, -1.112240025338166033E-15 ) ) ;
#6928 = CARTESIAN_POINT ( 'NONE',  ( 7.425000001229034474, 2.886751345948129099, -4.999999999999998224 ) ) ;
#6929 = CARTESIAN_POINT ( 'NONE',  ( 17.70937500061451431, 0.000000000000000000, 5.243569643749999010 ) ) ;
#6930 = CARTESIAN_POINT ( 'NONE',  ( 11.74687500061451573, 6.054752690667223547, 3.707466751127219781E-16 ) ) ;
#6931 = LINE ( 'NONE', #52357, #28901 ) ;
#6932 = ORIENTED_EDGE ( 'NONE', *, *, #6481, .F. ) ;
#6933 = CARTESIAN_POINT ( 'NONE',  ( 12.89062500061451821, -3.027376345333610441, -5.243569643749999898 ) ) ;
#6934 = CARTESIAN_POINT ( 'NONE',  ( 26.92500000122903359, 2.886751345948126879, 4.999999999999999112 ) ) ;
#6935 = CARTESIAN_POINT ( 'NONE',  ( 12.15937500061451892, 4.541064518000418104, -2.621784821874998173 ) ) ;
#6936 = LINE ( 'NONE', #29467, #2860 ) ;
#6937 = CARTESIAN_POINT ( 'NONE',  ( 14.35312500061451679, 4.541064518000418104, -2.621784821874998173 ) ) ;
#6938 = DIRECTION ( 'NONE',  ( 0.000000000000000000, 0.000000000000000000, -1.000000000000000000 ) ) ;
#6939 = CARTESIAN_POINT ( 'NONE',  ( 23.78437500061451360, 6.421520780324663323E-16, -5.243569643749999010 ) ) ;
#6940 = CARTESIAN_POINT ( 'NONE',  ( 1.626862140677534273E-15, 10.21250000000000036, -26.00000000000000355 ) ) ;
#6941 = CARTESIAN_POINT ( 'NONE',  ( 12.67500000122903536, -5.773502691896255534, -1.060575238724906372E-15 ) ) ;
#6942 = CARTESIAN_POINT ( 'NONE',  ( 8.671875000614518214, 2.746126346562643317, 4.756430356249998326 ) ) ;
#6943 = CARTESIAN_POINT ( 'NONE',  ( 5.475000000000000533, 6.123233995736764310E-16, -4.999999999999998224 ) ) ;
#6944 = CARTESIAN_POINT ( 'NONE',  ( 2.121784821875001281, 16.85937500061451999, -26.32496088578401938 ) ) ;
#6945 = CARTESIAN_POINT ( 'NONE',  ( 18.64687500061451786, -3.027376345333614438, 5.243569643749998122 ) ) ;
#6946 = CARTESIAN_POINT ( 'NONE',  ( 21.03750000122903074, 4.330127018922191873, 2.499999999999999556 ) ) ;
#6947 = CARTESIAN_POINT ( 'NONE',  ( 13.50937500061451679, 4.541064518000418104, -2.621784821874998173 ) ) ;
#6948 = CARTESIAN_POINT ( 'NONE',  ( 4.243569643749999898, 11.08437500061451786, 30.00000000000000000 ) ) ;
#6949 = CARTESIAN_POINT ( 'NONE',  ( 19.35000000122903430, -2.886751345948129988, 4.999999999999997335 ) ) ;
#6950 = CARTESIAN_POINT ( 'NONE',  ( 16.00312500061451715, -4.541064518000417216, -2.621784821875001281 ) ) ;
#6951 = ORIENTED_EDGE ( 'NONE', *, *, #55418, .F. ) ;
#6952 = ORIENTED_EDGE ( 'NONE', *, *, #30275, .F. ) ;
#6953 = CARTESIAN_POINT ( 'NONE',  ( 18.86249999999999716, -5.773502691896255534, -1.060575238724906372E-15 ) ) ;
#6954 = CARTESIAN_POINT ( 'NONE',  ( 4.000000000000000000, 15.59374999877096535, 30.00000000000000000 ) ) ;
#6955 = CARTESIAN_POINT ( 'NONE',  ( 3.853125000614517681, -4.541064518000417216, -2.621784821875001281 ) ) ;
#6956 = CARTESIAN_POINT ( 'NONE',  ( 14.36250000122903359, 0.000000000000000000, 4.999999999999998224 ) ) ;
#6957 = CARTESIAN_POINT ( 'NONE',  ( 26.14687500061451431, 6.054752690667223547, 3.707466751127219781E-16 ) ) ;
#6958 = CARTESIAN_POINT ( 'NONE',  ( 19.60312500061451502, -4.541064518000417216, -2.621784821875001281 ) ) ;
#6959 =( BOUNDED_CURVE ( )  B_SPLINE_CURVE ( 2, ( #69793, #36171, #48363, #47997, #19159, #58689, #9197 ),
 .UNSPECIFIED., .F., .F. ) 
 B_SPLINE_CURVE_WITH_KNOTS ( ( 3, 2, 2, 3 ),
 ( 0.3416666666666666186, 0.3444444444444444420, 0.3472222222222222099, 0.3500000000000000333 ),
 .UNSPECIFIED. ) 
 CURVE ( )  GEOMETRIC_REPRESENTATION_ITEM ( )  RATIONAL_B_SPLINE_CURVE ( ( 1.000000000000002665, 0.8660254037844360431, 1.000000000000000000, 0.8660254037844387076, 1.000000000000000000, 0.8660254037844360431, 1.000000000000002665 ) ) 
 REPRESENTATION_ITEM ( '' )  );
#6960 = CARTESIAN_POINT ( 'NONE',  ( 22.67812500061451431, -4.541064518000419881, 2.621784821874995952 ) ) ;
#6961 = CARTESIAN_POINT ( 'NONE',  ( 3.628125000614518036, 4.541064518000418104, 2.621784821874999949 ) ) ;
#6962 = CARTESIAN_POINT ( 'NONE',  ( 26.62500000000000000, 6.123233995736764310E-16, -4.999999999999998224 ) ) ;
#6963 = CARTESIAN_POINT ( 'NONE',  ( 27.91875000122902861, -5.773502691896255534, -1.060575238724906372E-15 ) ) ;
#6964 = CARTESIAN_POINT ( 'NONE',  ( 8.296875000614516438, -2.746126346562646425, 4.756430356249996549 ) ) ;
#6965 = CARTESIAN_POINT ( 'NONE',  ( 45.00000000000000000, 6.123233995736764310E-16, -4.999999999999998224 ) ) ;
#6966 = CARTESIAN_POINT ( 'NONE',  ( 3.999999999999998668, 10.02500000122903501, -32.30940107675850470 ) ) ;
#6967 = CARTESIAN_POINT ( 'NONE',  ( 4.243569643749999898, 15.99687500061451573, -27.54997392385601529 ) ) ;
#6968 = CARTESIAN_POINT ( 'NONE',  ( 5.512500001229033941, -4.330127018922190985, -2.500000000000001332 ) ) ;
#6969 = CARTESIAN_POINT ( 'NONE',  ( 5.400000000000002132, -4.330127018922190985, -2.500000000000001332 ) ) ;
#6970 = EDGE_CURVE ( 'NONE', #29785, #60995, #19829, .T. ) ;
#6971 = CARTESIAN_POINT ( 'NONE',  ( 4.462500001229035007, 0.000000000000000000, 4.999999999999998224 ) ) ;
#6972 = CARTESIAN_POINT ( 'NONE',  ( 8.821875000614518569, -6.054752690667223547, -1.112240025338166033E-15 ) ) ;
#6973 = CARTESIAN_POINT ( 'NONE',  ( 28.86562500061451786, 3.027376345333611329, 5.243569643749999010 ) ) ;
#6974 = CARTESIAN_POINT ( 'NONE',  ( 15.58125000122903181, 4.330127018922191873, 2.499999999999999556 ) ) ;
#6975 = CARTESIAN_POINT ( 'NONE',  ( 18.41250000122903430, 0.000000000000000000, 4.999999999999998224 ) ) ;
#6976 = CARTESIAN_POINT ( 'NONE',  ( 3.486133158594716510E-16, 19.55000000122903359, -34.00000000000000000 ) ) ;
#6977 = CARTESIAN_POINT ( 'NONE',  ( 7.696875000614516793, 6.054752690667223547, 3.707466751127219781E-16 ) ) ;
#6978 = CARTESIAN_POINT ( 'NONE',  ( 10.28437500061451715, 6.421520780324663323E-16, -5.243569643749999010 ) ) ;
#6979 = CARTESIAN_POINT ( 'NONE',  ( 6.225000000000001421, -4.330127018922194537, 2.499999999999995559 ) ) ;
#6980 = CARTESIAN_POINT ( 'NONE',  ( 4.243569643749999898, 15.94062500061459176, 32.45002607614398471 ) ) ;
#6981 = CARTESIAN_POINT ( 'NONE',  ( 22.32187500061451502, -6.054752690667223547, -1.112240025338166033E-15 ) ) ;
#6982 = CARTESIAN_POINT ( 'NONE',  ( 1.071796769724493892, 18.06740381056766864, 26.00000000000000711 ) ) ;
#6983 = CARTESIAN_POINT ( 'NONE',  ( 5.737499999999998934, -2.886751345948129988, 4.999999999999997335 ) ) ;
#6984 = CARTESIAN_POINT ( 'NONE',  ( 27.22500000122903430, 2.886751345948129099, -4.999999999999998224 ) ) ;
#6985 = CARTESIAN_POINT ( 'NONE',  ( 18.08437500061451075, -2.746126346562646425, 4.756430356249996549 ) ) ;
#6986 = CARTESIAN_POINT ( 'NONE',  ( 21.59062500061451928, 6.054752690667223547, 3.707466751127219781E-16 ) ) ;
#6987 = CARTESIAN_POINT ( 'NONE',  ( 12.74062500061451786, -3.027376345333614438, 5.243569643749998122 ) ) ;
#6988 = CARTESIAN_POINT ( 'NONE',  ( 26.82187500061451502, 5.824947211148865298E-16, -4.756430356249998326 ) ) ;
#6989 = CARTESIAN_POINT ( 'NONE',  ( 10.92187500061451644, 3.027376345333611329, 5.243569643749999010 ) ) ;
#6990 = CARTESIAN_POINT ( 'NONE',  ( 28.83749999999999858, -2.886751345948125991, -5.000000000000000000 ) ) ;
#6991 = CARTESIAN_POINT ( 'NONE',  ( 22.20000000122903216, -2.886751345948125991, -5.000000000000000000 ) ) ;
#6992 = CARTESIAN_POINT ( 'NONE',  ( -3.999999999999999112, 18.27500000122903501, -32.30940107675850470 ) ) ;
#6993 = CARTESIAN_POINT ( 'NONE',  ( 12.57187500061451857, 3.027376345333613106, -5.243569643749998122 ) ) ;
#6994 = CARTESIAN_POINT ( 'NONE',  ( 27.94687500061451502, 6.054752690667223547, 3.707466751127219781E-16 ) ) ;
#6995 = CARTESIAN_POINT ( 'NONE',  ( 21.73125000122903216, 6.123233995736764310E-16, -4.999999999999998224 ) ) ;
#6996 = CARTESIAN_POINT ( 'NONE',  ( -1.071796769724504328, 14.69240381056766687, 33.99999999999999289 ) ) ;
#6997 = CARTESIAN_POINT ( 'NONE',  ( 23.25937500061451857, -4.541064518000417216, -2.621784821875001281 ) ) ;
#6998 = CARTESIAN_POINT ( 'NONE',  ( 15.12187500061451750, -6.054752690667223547, -1.112240025338166033E-15 ) ) ;
#6999 = CARTESIAN_POINT ( 'NONE',  ( -1.878215178125001827, 18.90312499938548285, 33.25316411605952283 ) ) ;
#7000 = CARTESIAN_POINT ( 'NONE',  ( 25.19999999999999929, -4.330127018922190985, -2.500000000000001332 ) ) ;
#7001 = CARTESIAN_POINT ( 'NONE',  ( 3.756430356249998770, 20.25312499938547717, 32.16877607737302469 ) ) ;
#7002 = CARTESIAN_POINT ( 'NONE',  ( 27.49687500061451217, 5.492252693125287522, 3.363034840372157021E-16 ) ) ;
#7003 = CARTESIAN_POINT ( 'NONE',  ( 17.54062500061451502, 6.054752690667223547, 3.707466751127219781E-16 ) ) ;
#7004 = CARTESIAN_POINT ( 'NONE',  ( 7.387500000000001066, 5.773502691896255534, 3.535250795749688894E-16 ) ) ;
#7005 = CARTESIAN_POINT ( 'NONE',  ( 45.00000000000000000, 0.000000000000000000, 4.999999999999998224 ) ) ;
#7006 =( BOUNDED_CURVE ( )  B_SPLINE_CURVE ( 2, ( #19775, #70761, #70399, #41240, #20136, #53777, #42326 ),
 .UNSPECIFIED., .F., .F. ) 
 B_SPLINE_CURVE_WITH_KNOTS ( ( 3, 2, 2, 3 ),
 ( 0.07999999999999998779, 0.08333333333333331483, 0.08666666666666664187, 0.08999999999999996891 ),
 .UNSPECIFIED. ) 
 CURVE ( )  GEOMETRIC_REPRESENTATION_ITEM ( )  RATIONAL_B_SPLINE_CURVE ( ( 1.000000000000000666, 0.8660254037844381525, 1.000000000000000000, 0.8660254037844387076, 1.000000000000000000, 0.8660254037844398178, 0.9999999999999988898 ) ) 
 REPRESENTATION_ITEM ( '' )  );
#7007 = CARTESIAN_POINT ( 'NONE',  ( 15.33750000000000036, -2.886751345948125991, -5.000000000000000000 ) ) ;
#7008 = CARTESIAN_POINT ( 'NONE',  ( 2.121784821874999061, 10.65312500061451750, 26.32496088578401583 ) ) ;
#7009 = CARTESIAN_POINT ( 'NONE',  ( 25.20937500061451431, 4.541064518000418104, -2.621784821874998173 ) ) ;
#7010 = ORIENTED_EDGE ( 'NONE', *, *, #39141, .T. ) ;
#7011 = CARTESIAN_POINT ( 'NONE',  ( 20.61562500061451431, 3.027376345333613106, -5.243569643749998122 ) ) ;
#7012 = CARTESIAN_POINT ( 'NONE',  ( 21.04687500061451644, -3.027376345333610441, -5.243569643749999898 ) ) ;
#7013 = CARTESIAN_POINT ( 'NONE',  ( 3.675000000000001155, 6.123233995736764310E-16, -4.999999999999998224 ) ) ;
#7014 = CARTESIAN_POINT ( 'NONE',  ( 6.853125000614516793, 0.000000000000000000, 5.243569643749999010 ) ) ;
#7015 = CARTESIAN_POINT ( 'NONE',  ( 20.84062500061451573, -3.027376345333614438, 5.243569643749998122 ) ) ;
#7016 = CARTESIAN_POINT ( 'NONE',  ( 12.42187500061451821, -6.054752690667223547, -1.112240025338166033E-15 ) ) ;
#7017 = CARTESIAN_POINT ( 'NONE',  ( 16.73437500061451644, 4.541064518000418104, 2.621784821874999949 ) ) ;
#7018 = CARTESIAN_POINT ( 'NONE',  ( 4.243569643749999010, 18.26562500061451644, 27.54997392385601174 ) ) ;
#7019 = CARTESIAN_POINT ( 'NONE',  ( 18.22500000122903430, 2.886751345948129099, -4.999999999999998224 ) ) ;
#7020 = CARTESIAN_POINT ( 'NONE',  ( 14.18437500061451750, -4.119189519843968306, 2.378215178124996054 ) ) ;
#7021 = CARTESIAN_POINT ( 'NONE',  ( 10.22812500061451679, 6.421520780324663323E-16, -5.243569643749999010 ) ) ;
#7022 = CARTESIAN_POINT ( 'NONE',  ( 4.209375000614516971, 0.000000000000000000, 5.243569643749999010 ) ) ;
#7023 = CARTESIAN_POINT ( 'NONE',  ( 4.846875000614519813, -3.027376345333610441, -5.243569643749999898 ) ) ;
#7024 = CARTESIAN_POINT ( 'NONE',  ( 25.32187500061451857, 3.027376345333611329, 5.243569643749999010 ) ) ;
#7025 = CARTESIAN_POINT ( 'NONE',  ( 17.42812500061451786, 6.421520780324663323E-16, -5.243569643749999010 ) ) ;
#7026 = CARTESIAN_POINT ( 'NONE',  ( 26.21250000122903501, -4.330127018922190985, -2.500000000000001332 ) ) ;
#7027 = EDGE_CURVE ( 'NONE', #25241, #16013, #25579, .T. ) ;
#7028 = CARTESIAN_POINT ( 'NONE',  ( 25.64062500061451644, 6.054752690667223547, 3.707466751127219781E-16 ) ) ;
#7029 = CARTESIAN_POINT ( 'NONE',  ( 21.57187500061451502, 3.027376345333613106, -5.243569643749998122 ) ) ;
#7030 = CARTESIAN_POINT ( 'NONE',  ( 17.24062500061451786, -3.027376345333614438, 5.243569643749998122 ) ) ;
#7031 = CARTESIAN_POINT ( 'NONE',  ( -4.243569643749997233, 16.74687500061451928, 32.45002607614398471 ) ) ;
#7032 = EDGE_CURVE ( 'NONE', #41820, #427, #28388, .T. ) ;
#7033 = CARTESIAN_POINT ( 'NONE',  ( 21.89062500061451289, -3.027376345333610441, -5.243569643749999898 ) ) ;
#7034 = CARTESIAN_POINT ( 'NONE',  ( 2.962500001229034119, 4.330127018922192761, -2.499999999999997780 ) ) ;
#7035 = ORIENTED_EDGE ( 'NONE', *, *, #58291, .F. ) ;
#7036 = CARTESIAN_POINT ( 'NONE',  ( 24.82499999999999929, 6.123233995736764310E-16, -4.999999999999998224 ) ) ;
#7037 = CARTESIAN_POINT ( 'NONE',  ( 2.000000000000001332, 13.40000000000000213, -26.53589838486224650 ) ) ;
#7038 = CARTESIAN_POINT ( 'NONE',  ( 1.878215178124997609, 18.97812499938548214, 33.25316411605952993 ) ) ;
#7039 = CARTESIAN_POINT ( 'NONE',  ( 29.39062500061451289, -3.027376345333614438, 5.243569643749998122 ) ) ;
#7040 = CARTESIAN_POINT ( 'NONE',  ( 9.890625000614516438, 6.054752690667223547, 3.707466751127219781E-16 ) ) ;
#7041 = CARTESIAN_POINT ( 'NONE',  ( 22.65000000122903856, -2.886751345948125991, -5.000000000000000000 ) ) ;
#7042 = CARTESIAN_POINT ( 'NONE',  ( 26.61562500061451786, 3.027376345333611329, 5.243569643749999010 ) ) ;
#7043 = CARTESIAN_POINT ( 'NONE',  ( 24.93750000000000355, 5.773502691896255534, 3.535250795749688894E-16 ) ) ;
#7044 = CARTESIAN_POINT ( 'NONE',  ( 2.000000000000001332, 16.21250000122903501, -26.53589838486224650 ) ) ;
#7045 = EDGE_CURVE ( 'NONE', #27917, #71509, #35924, .T. ) ;
#7046 = CARTESIAN_POINT ( 'NONE',  ( 29.50312500061451360, -4.541064518000417216, -2.621784821875001281 ) ) ;
#7047 = CARTESIAN_POINT ( 'NONE',  ( 10.15312500061451750, -4.541064518000417216, -2.621784821875001281 ) ) ;
#7048 = ORIENTED_EDGE ( 'NONE', *, *, #38793, .T. ) ;
#7049 = CARTESIAN_POINT ( 'NONE',  ( 26.16562500061451502, 3.027376345333611329, 5.243569643749999010 ) ) ;
#7050 = CARTESIAN_POINT ( 'NONE',  ( 7.640625000614517326, 6.054752690667223547, 3.707466751127219781E-16 ) ) ;
#7051 = UNCERTAINTY_MEASURE_WITH_UNIT (LENGTH_MEASURE( 1.000000000000000082E-05 ), #33832, 'distance_accuracy_value', 'NONE');
#7052 = CARTESIAN_POINT ( 'NONE',  ( 5.353125000614515905, 4.541064518000418104, -2.621784821874998173 ) ) ;
#7053 = CARTESIAN_POINT ( 'NONE',  ( 15.72187500061451892, 2.746126346562645981, -4.756430356249997438 ) ) ;
#7054 = EDGE_CURVE ( 'NONE', #29691, #41395, #51037, .T. ) ;
#7055 = CARTESIAN_POINT ( 'NONE',  ( 4.664282881542661130, -1.801239906550150316, 4.924485496770981463 ) ) ;
#7056 = CARTESIAN_POINT ( 'NONE',  ( 13.50000000000000178, -4.330127018922190985, -2.500000000000001332 ) ) ;
#7057 = CARTESIAN_POINT ( 'NONE',  ( 13.92187500061451644, 3.027376345333613106, -5.243569643749998122 ) ) ;
#7058 = CARTESIAN_POINT ( 'NONE',  ( 12.26250000122903394, -4.330127018922190985, -2.500000000000001332 ) ) ;
#7059 = CARTESIAN_POINT ( 'NONE',  ( 16.73437500061451644, 4.541064518000418104, 2.621784821874999949 ) ) ;
#7060 = CARTESIAN_POINT ( 'NONE',  ( 17.13749999999999929, -2.886751345948125991, -5.000000000000000000 ) ) ;
#7061 = CARTESIAN_POINT ( 'NONE',  ( 8.221875000614518925, 3.027376345333611329, 5.243569643749999010 ) ) ;
#7062 = CARTESIAN_POINT ( 'NONE',  ( 2.121784821875001281, 10.95312500061451821, -26.32496088578401938 ) ) ;
#7063 = CARTESIAN_POINT ( 'NONE',  ( 0.000000000000000000, 27.50000000000000000, 30.00000000000000000 ) ) ;
#7064 = CARTESIAN_POINT ( 'NONE',  ( 23.70937500061451786, 2.746126346562645981, -4.756430356249997438 ) ) ;
#7065 = CARTESIAN_POINT ( 'NONE',  ( 1.071796769724476572, 11.58259618943233349, -25.99999999999999289 ) ) ;
#7066 = CARTESIAN_POINT ( 'NONE',  ( 23.87812500061451715, 4.541064518000418104, 2.621784821874999949 ) ) ;
#7067 =( NAMED_UNIT ( * ) PLANE_ANGLE_UNIT ( ) SI_UNIT ( $, .RADIAN. ) );
#7068 = CARTESIAN_POINT ( 'NONE',  ( 29.48437500061451644, -4.541064518000419881, 2.621784821874995952 ) ) ;
#7069 = CARTESIAN_POINT ( 'NONE',  ( 24.93750000000000355, 5.773502691896255534, 3.535250795749688894E-16 ) ) ;
#7070 = CARTESIAN_POINT ( 'NONE',  ( 7.115625000614516082, 3.027376345333613106, -5.243569643749998122 ) ) ;
#7071 = CARTESIAN_POINT ( 'NONE',  ( 25.88437500061451857, -2.746126346562642428, -4.756430356249999214 ) ) ;
#7072 = CARTESIAN_POINT ( 'NONE',  ( 18.90937500061451360, 4.541064518000418104, -2.621784821874998173 ) ) ;
#7073 = CARTESIAN_POINT ( 'NONE',  ( 11.59687500061451537, 4.119189519843966529, -2.378215178124998275 ) ) ;
#7074 = CARTESIAN_POINT ( 'NONE',  ( 2.840625000614518392, -3.027376345333614438, 5.243569643749998122 ) ) ;
#7075 = CARTESIAN_POINT ( 'NONE',  ( 8.146875000614516082, 6.054752690667223547, 3.707466751127219781E-16 ) ) ;
#7076 = EDGE_LOOP ( 'NONE', ( #16722, #40633, #37631, #31100 ) ) ;
#7077 = CARTESIAN_POINT ( 'NONE',  ( 19.35937500061451644, 4.541064518000418104, -2.621784821874998173 ) ) ;
#7078 = DIRECTION ( 'NONE',  ( -1.000000000000000000, -0.000000000000000000, -0.000000000000000000 ) ) ;
#7079 = CARTESIAN_POINT ( 'NONE',  ( 26.92499999999999716, -4.330127018922194537, 2.499999999999995559 ) ) ;
#7080 = CARTESIAN_POINT ( 'NONE',  ( 28.62187500061451573, -6.054752690667223547, -1.112240025338166033E-15 ) ) ;
#7081 = CARTESIAN_POINT ( 'NONE',  ( 29.58749999999999858, -2.886751345948150860, 4.999999999999960920 ) ) ;
#7082 = CARTESIAN_POINT ( 'NONE',  ( 15.97499999999999964, 4.330127018922191873, 2.499999999999999556 ) ) ;
#7083 = VERTEX_POINT ( 'NONE', #46833 ) ;
#7084 = CARTESIAN_POINT ( 'NONE',  ( 10.65000000000000036, 0.000000000000000000, 4.999999999999998224 ) ) ;
#7085 = CARTESIAN_POINT ( 'NONE',  ( 10.80937500061451573, 2.746126346562643317, 4.756430356249998326 ) ) ;
#7086 = CARTESIAN_POINT ( 'NONE',  ( 25.34062500061451217, -3.027376345333614438, 5.243569643749998122 ) ) ;
#7087 = CARTESIAN_POINT ( 'NONE',  ( 14.73749999999999893, -2.886751345948129988, 4.999999999999997335 ) ) ;
#7088 = CARTESIAN_POINT ( 'NONE',  ( 9.862500001229033586, 0.000000000000000000, 4.999999999999998224 ) ) ;
#7089 = CARTESIAN_POINT ( 'NONE',  ( 8.053125000614516082, 4.541064518000418104, -2.621784821874998173 ) ) ;
#7090 = CARTESIAN_POINT ( 'NONE',  ( 22.94999999999999929, -4.330127018922190985, -2.500000000000001332 ) ) ;
#7091 = CARTESIAN_POINT ( 'NONE',  ( 19.86562500061451786, 3.027376345333611329, 5.243569643749999010 ) ) ;
#7092 = LINE ( 'NONE', #34795, #1877 ) ;
#7093 = CARTESIAN_POINT ( 'NONE',  ( 26.13750000122903216, -4.330127018922194537, 2.499999999999995559 ) ) ;
#7094 = CARTESIAN_POINT ( 'NONE',  ( -1.878215178124999163, 17.74062499938548498, 26.74683588394047007 ) ) ;
#7095 = CARTESIAN_POINT ( 'NONE',  ( 5.250000000000000888, 0.000000000000000000, 4.999999999999998224 ) ) ;
#7096 = VERTEX_POINT ( 'NONE', #36831 ) ;
#7097 = CARTESIAN_POINT ( 'NONE',  ( 22.97812500061451857, 4.541064518000418104, 2.621784821874999949 ) ) ;
#7098 = CARTESIAN_POINT ( 'NONE',  ( 29.12812500061451715, 6.421520780324663323E-16, -5.243569643749999010 ) ) ;
#7099 = CARTESIAN_POINT ( 'NONE',  ( 28.28437500061451715, 6.421520780324663323E-16, -5.243569643749999010 ) ) ;
#7100 = CARTESIAN_POINT ( 'NONE',  ( 18.19687500061451502, -3.027376345333614438, 5.243569643749998122 ) ) ;
#7101 = CARTESIAN_POINT ( 'NONE',  ( 14.87812500061451537, 4.541064518000418104, 2.621784821874999949 ) ) ;
#7102 = CARTESIAN_POINT ( 'NONE',  ( 12.09375000122903288, -2.886751345948074920, 5.000000000000092371 ) ) ;
#7103 = CARTESIAN_POINT ( 'NONE',  ( 27.22500000122903430, 2.886751345948129099, -4.999999999999998224 ) ) ;
#7104 = CARTESIAN_POINT ( 'NONE',  ( 23.10937500061451644, 0.000000000000000000, 4.756430356249998326 ) ) ;
#7105 = CARTESIAN_POINT ( 'NONE',  ( 17.69062500061451715, -3.027376345333614438, 5.243569643749998122 ) ) ;
#7106 = LINE ( 'NONE', #22997, #42126 ) ;
#7107 = CARTESIAN_POINT ( 'NONE',  ( 3.075000001229035718, 2.886751345948126879, 4.999999999999999112 ) ) ;
#7108 = CARTESIAN_POINT ( 'NONE',  ( 11.63437500061451857, 6.421520780324663323E-16, -5.243569643749999010 ) ) ;
#7109 = CARTESIAN_POINT ( 'NONE',  ( 11.33437500061451608, 4.541064518000418104, 2.621784821874999949 ) ) ;
#7110 = CARTESIAN_POINT ( 'NONE',  ( 19.24687500061452283, -3.027376345333610441, -5.243569643749999898 ) ) ;
#7111 = VERTEX_POINT ( 'NONE', #2134 ) ;
#7112 = CARTESIAN_POINT ( 'NONE',  ( 9.825000000000001066, -4.330127018922194537, 2.499999999999995559 ) ) ;
#7113 = CARTESIAN_POINT ( 'NONE',  ( 25.07812500061451644, 6.421520780324663323E-16, -5.243569643749999010 ) ) ;
#7114 = CARTESIAN_POINT ( 'NONE',  ( 18.53437500061451715, 4.541064518000418104, 2.621784821874999949 ) ) ;
#7115 = CARTESIAN_POINT ( 'NONE',  ( 24.25312500061451715, 4.541064518000418104, -2.621784821874998173 ) ) ;
#7116 = CARTESIAN_POINT ( 'NONE',  ( 9.000000000000001776, -4.330127018922190985, -2.500000000000001332 ) ) ;
#7117 = CARTESIAN_POINT ( 'NONE',  ( -3.999999999999999112, 15.50000000000000000, 30.00000000000000000 ) ) ;
#7118 = CARTESIAN_POINT ( 'NONE',  ( 29.69062500061451715, 6.054752690667223547, 3.707466751127219781E-16 ) ) ;
#7119 = CARTESIAN_POINT ( 'NONE',  ( 10.42500000122903536, -5.773502691896255534, -1.060575238724906372E-15 ) ) ;
#7120 = CARTESIAN_POINT ( 'NONE',  ( 3.487500001229035362, 4.330127018922191873, 2.499999999999999556 ) ) ;
#7121 = DIRECTION ( 'NONE',  ( -1.000000000000000000, -0.000000000000000000, -0.000000000000000000 ) ) ;
#7122 = CARTESIAN_POINT ( 'NONE',  ( 26.43750000122903288, 4.330127018922191873, 2.499999999999999556 ) ) ;
#7123 = CARTESIAN_POINT ( 'NONE',  ( 2.655984681222220721E-16, 13.76562499938548179, 25.66244784525396483 ) ) ;
#7124 = CARTESIAN_POINT ( 'NONE',  ( 9.196875000614518569, -3.027376345333614438, 5.243569643749998122 ) ) ;
#7125 = CARTESIAN_POINT ( 'NONE',  ( 4.000000000000000000, 9.950000001229033941, 32.30940107675849760 ) ) ;
#7126 = CARTESIAN_POINT ( 'NONE',  ( 17.54062500061451502, 6.054752690667223547, 3.707466751127219781E-16 ) ) ;
#7127 = CARTESIAN_POINT ( 'NONE',  ( 11.03437500061451715, -4.541064518000419881, 2.621784821874995952 ) ) ;
#7128 = CARTESIAN_POINT ( 'NONE',  ( 2.803125000614518747, 0.000000000000000000, 5.243569643749999010 ) ) ;
#7129 = CARTESIAN_POINT ( 'NONE',  ( 18.90937500061451360, 4.541064518000418104, -2.621784821874998173 ) ) ;
#7130 = CARTESIAN_POINT ( 'NONE',  ( 7.209375000614519635, 4.541064518000418104, -2.621784821874998173 ) ) ;
#7131 = CARTESIAN_POINT ( 'NONE',  ( 3.028125000614518392, 6.421520780324663323E-16, -5.243569643749999010 ) ) ;
#7132 = CARTESIAN_POINT ( 'NONE',  ( 11.85000000122903430, -2.886751345948193048, -4.999999999999883649 ) ) ;
#7133 = EDGE_CURVE ( 'NONE', #65361, #57985, #69722, .T. ) ;
#7134 = CARTESIAN_POINT ( 'NONE',  ( 6.740625000614516082, 6.054752690667223547, 3.707466751127219781E-16 ) ) ;
#7135 = CARTESIAN_POINT ( 'NONE',  ( 17.99062500061451786, 6.054752690667223547, 3.707466751127219781E-16 ) ) ;
#7136 = ORIENTED_EDGE ( 'NONE', *, *, #1559, .F. ) ;
#7137 = CARTESIAN_POINT ( 'NONE',  ( 5.587500001229033231, 6.123233995736764310E-16, -4.999999999999998224 ) ) ;
#7138 = CARTESIAN_POINT ( 'NONE',  ( 14.76562500061451821, 3.027376345333613106, -5.243569643749998122 ) ) ;
#7139 = CARTESIAN_POINT ( 'NONE',  ( 12.74062500061451786, -3.027376345333614438, 5.243569643749998122 ) ) ;
#7140 = CARTESIAN_POINT ( 'NONE',  ( 23.97187500061451360, 2.746126346562643317, 4.756430356249998326 ) ) ;
#7141 = CARTESIAN_POINT ( 'NONE',  ( 14.55000000000000071, 4.330127018922192761, -2.499999999999997780 ) ) ;
#7142 = CARTESIAN_POINT ( 'NONE',  ( 5.587500001229033231, 6.123233995736764310E-16, -4.999999999999998224 ) ) ;
#7143 = CARTESIAN_POINT ( 'NONE',  ( 29.28749999999999787, -2.886751345948096237, -5.000000000000050626 ) ) ;
#7144 = CARTESIAN_POINT ( 'NONE',  ( 19.01250000122903216, -4.330127018922190985, -2.500000000000001332 ) ) ;
#7145 = CARTESIAN_POINT ( 'NONE',  ( 24.37500000000000000, 6.123233995736764310E-16, -4.999999999999998224 ) ) ;
#7146 = CARTESIAN_POINT ( 'NONE',  ( -4.243569643749999898, 9.959375000614517859, -30.00000000000000000 ) ) ;
#7147 = CARTESIAN_POINT ( 'NONE',  ( 4.158798725700454391, -2.776528725802326125, -4.158798725700454391 ) ) ;
#7148 = CARTESIAN_POINT ( 'NONE',  ( 23.58750000122903145, 6.123233995736764310E-16, -4.999999999999998224 ) ) ;
#7149 = EDGE_CURVE ( 'NONE', #20263, #39861, #3747, .T. ) ;
#7150 = CARTESIAN_POINT ( 'NONE',  ( 6.412500000000001421, 2.886751345948129099, -4.999999999999997335 ) ) ;
#7151 = CARTESIAN_POINT ( 'NONE',  ( 4.509375000614518569, 4.541064518000418104, -2.621784821874998173 ) ) ;
#7152 = CARTESIAN_POINT ( 'NONE',  ( 19.62187500061451573, -6.054752690667223547, -1.112240025338166033E-15 ) ) ;
#7153 = CARTESIAN_POINT ( 'NONE',  ( -1.071796769724496556, 16.60490381179669939, 33.99999999999998579 ) ) ;
#7154 = CARTESIAN_POINT ( 'NONE',  ( 14.76562500061451821, 3.027376345333613106, -5.243569643749998122 ) ) ;
#7155 = CARTESIAN_POINT ( 'NONE',  ( 9.056250001229033231, -4.330127018922190985, -2.500000000000001332 ) ) ;
#7156 = PRODUCT_DEFINITION_SHAPE ( 'NONE', 'NONE',  #73121 ) ;
#7157 = CARTESIAN_POINT ( 'NONE',  ( 15.82500000122903216, -5.773502691896255534, -1.060575238724906372E-15 ) ) ;
#7158 = CARTESIAN_POINT ( 'NONE',  ( 25.50937500061451502, -4.541064518000417216, -2.621784821875001281 ) ) ;
#7159 = CARTESIAN_POINT ( 'NONE',  ( 19.20937500061451786, 2.746126346562645981, -4.756430356249997438 ) ) ;
#7160 = CARTESIAN_POINT ( 'NONE',  ( 10.71562500061451928, 3.027376345333613106, -5.243569643749998122 ) ) ;
#7161 = CARTESIAN_POINT ( 'NONE',  ( 16.09687500061452070, -3.027376345333610441, -5.243569643749999898 ) ) ;
#7162 = ORIENTED_EDGE ( 'NONE', *, *, #29219, .T. ) ;
#7163 = CARTESIAN_POINT ( 'NONE',  ( 27.55312500061451786, 0.000000000000000000, 5.243569643749999010 ) ) ;
#7164 = CARTESIAN_POINT ( 'NONE',  ( 19.64062500061451644, -3.027376345333610441, -5.243569643749999898 ) ) ;
#7165 = CARTESIAN_POINT ( 'NONE',  ( 4.000000000000000000, 13.10000000122903430, -27.69059892324149885 ) ) ;
#7166 = CARTESIAN_POINT ( 'NONE',  ( -1.999999999999997113, 14.33750000122903323, -26.53589838486224295 ) ) ;
#7167 = EDGE_CURVE ( 'NONE', #52378, #23627, #60959, .T. ) ;
#7168 = CARTESIAN_POINT ( 'NONE',  ( 10.95000000000000107, 4.330127018922192761, -2.499999999999997780 ) ) ;
#7169 = CARTESIAN_POINT ( 'NONE',  ( 19.46250000122903145, -4.330127018922190985, -2.500000000000001332 ) ) ;
#7170 = DIRECTION ( 'NONE',  ( -0.000000000000000000, -1.000000000000000000, -0.000000000000000000 ) ) ;
#7171 = CARTESIAN_POINT ( 'NONE',  ( 9.871875000614517504, 4.119189519843966529, 2.378215178124999607 ) ) ;
#7172 = EDGE_LOOP ( 'NONE', ( #5379, #56471, #55522, #12450 ) ) ;
#7173 = CARTESIAN_POINT ( 'NONE',  ( 17.55000000000000071, -4.330127018922190985, -2.500000000000001332 ) ) ;
#7174 = CARTESIAN_POINT ( 'NONE',  ( 21.37499999999999645, 4.330127018922191873, 2.499999999999999556 ) ) ;
#7175 = CARTESIAN_POINT ( 'NONE',  ( 19.35937500061451644, 4.541064518000418104, -2.621784821874998173 ) ) ;
#7176 = CARTESIAN_POINT ( 'NONE',  ( 24.21562500061451573, 3.027376345333613106, -5.243569643749998122 ) ) ;
#7177 = EDGE_LOOP ( 'NONE', ( #11101, #3235, #72498, #29360 ) ) ;
#7178 = CARTESIAN_POINT ( 'NONE',  ( 19.79999999999999716, -4.330127018922190985, -2.500000000000001332 ) ) ;
#7179 = CARTESIAN_POINT ( 'NONE',  ( 5.878125000614517148, 4.541064518000418104, 2.621784821874999949 ) ) ;
#7180 = CARTESIAN_POINT ( 'NONE',  ( 9.018750001229033586, -5.773502691896255534, -1.060575238724906372E-15 ) ) ;
#7181 = CARTESIAN_POINT ( 'NONE',  ( 14.62500000000000000, 4.330127018922191873, 2.499999999999999556 ) ) ;
#7182 = CARTESIAN_POINT ( 'NONE',  ( -4.243569643749997233, 18.04062500061451857, 32.45002607614398471 ) ) ;
#7183 = CARTESIAN_POINT ( 'NONE',  ( 3.159375000614518036, 4.541064518000418104, -2.621784821874998173 ) ) ;
#7184 = CARTESIAN_POINT ( 'NONE',  ( 10.68750000000000000, -2.886751345948129988, 4.999999999999997335 ) ) ;
#7185 = CARTESIAN_POINT ( 'NONE',  ( 3.756430356249998770, 18.00312499938548427, 32.16877607737302469 ) ) ;
#7186 = CARTESIAN_POINT ( 'NONE',  ( 25.35937500061451644, 0.000000000000000000, 5.243569643749999010 ) ) ;
#7187 = ORIENTED_EDGE ( 'NONE', *, *, #38408, .T. ) ;
#7188 = CARTESIAN_POINT ( 'NONE',  ( 20.35312500061451502, 0.000000000000000000, 5.243569643749999010 ) ) ;
#7189 = CARTESIAN_POINT ( 'NONE',  ( 23.37187500061451573, 3.027376345333613106, -5.243569643749998122 ) ) ;
#7190 = CARTESIAN_POINT ( 'NONE',  ( -2.121784821874999949, 16.57812500061459460, -33.67503911421598417 ) ) ;
#7191 = CARTESIAN_POINT ( 'NONE',  ( 6.590625000614518392, -3.027376345333610441, -5.243569643749999898 ) ) ;
#7192 = CARTESIAN_POINT ( 'NONE',  ( 28.50937500061451502, 0.000000000000000000, 4.756430356249998326 ) ) ;
#7193 = CARTESIAN_POINT ( 'NONE',  ( 23.87812500061451715, 4.541064518000418104, 2.621784821874999949 ) ) ;
#7194 = CARTESIAN_POINT ( 'NONE',  ( 28.47187500061451715, -4.119189519843968306, 2.378215178124996054 ) ) ;
#7195 = CARTESIAN_POINT ( 'NONE',  ( 12.15937500061451892, 4.119189519843966529, -2.378215178124998275 ) ) ;
#7196 = CARTESIAN_POINT ( 'NONE',  ( 17.70937500061451431, 0.000000000000000000, 5.243569643749999010 ) ) ;
#7197 = CARTESIAN_POINT ( 'NONE',  ( 19.62187500061451573, -6.054752690667223547, -1.112240025338166033E-15 ) ) ;
#7198 = CARTESIAN_POINT ( 'NONE',  ( 26.48437500061451644, 6.421520780324663323E-16, -5.243569643749999010 ) ) ;
#7199 = CARTESIAN_POINT ( 'NONE',  ( 2.121784821874999061, 17.45937500061451786, 26.32496088578401583 ) ) ;
#7200 = CARTESIAN_POINT ( 'NONE',  ( 7.603125000614517681, 4.541064518000418104, -2.621784821874998173 ) ) ;
#7201 = CARTESIAN_POINT ( 'NONE',  ( 45.00000000000000000, 0.000000000000000000, 0.000000000000000000 ) ) ;
#7202 = CARTESIAN_POINT ( 'NONE',  ( 5.259375000614518569, -4.541064518000417216, -2.621784821875001281 ) ) ;
#7203 = CARTESIAN_POINT ( 'NONE',  ( 0.000000000000000000, 27.50000000000000000, 30.00000000000000000 ) ) ;
#7204 = CARTESIAN_POINT ( 'NONE',  ( 5.803125000614517859, 4.541064518000418104, -2.621784821874998173 ) ) ;
#7205 = CARTESIAN_POINT ( 'NONE',  ( 9.009375000614518569, 4.541064518000418104, -2.621784821874998173 ) ) ;
#7206 = SHAPE_REPRESENTATION_RELATIONSHIP ( 'NONE' , 'NONE' ,  #46217, #30285 ) ;
#7207 = CARTESIAN_POINT ( 'NONE',  ( 17.55000000122903359, -2.886751345948129988, 4.999999999999997335 ) ) ;
#7208 = CARTESIAN_POINT ( 'NONE',  ( 4.734375000614518214, -4.541064518000419881, 2.621784821874995952 ) ) ;
#7209 = CARTESIAN_POINT ( 'NONE',  ( 6.328125000614515550, 4.541064518000418104, 2.621784821874999949 ) ) ;
#7210 = CARTESIAN_POINT ( 'NONE',  ( -1.999999999999999112, 14.39374999877096606, 26.53589838486224650 ) ) ;
#7211 = CARTESIAN_POINT ( 'NONE',  ( 22.63125000122903430, 6.123233995736764310E-16, -4.999999999999998224 ) ) ;
#7212 = CARTESIAN_POINT ( 'NONE',  ( 16.02187500061451786, -6.054752690667223547, -1.112240025338166033E-15 ) ) ;
#7213 = DIRECTION ( 'NONE',  ( 0.000000000000000000, 0.000000000000000000, 1.000000000000000000 ) ) ;
#7214 = ORIENTED_EDGE ( 'NONE', *, *, #17788, .F. ) ;
#7215 = CARTESIAN_POINT ( 'NONE',  ( 23.91562500061451502, 3.027376345333611329, 5.243569643749999010 ) ) ;
#7216 = CARTESIAN_POINT ( 'NONE',  ( 8.690625000614515372, -3.027376345333614438, 5.243569643749998122 ) ) ;
#7217 = CARTESIAN_POINT ( 'NONE',  ( 26.85937500061451644, -4.541064518000417216, -2.621784821875001281 ) ) ;
#7218 = CARTESIAN_POINT ( 'NONE',  ( 9.328125000614518214, 6.421520780324663323E-16, -5.243569643749999010 ) ) ;
#7219 = CARTESIAN_POINT ( 'NONE',  ( 25.51875000122903003, 2.886751345948098901, 5.000000000000047073 ) ) ;
#7220 = CARTESIAN_POINT ( 'NONE',  ( 11.51250000122903216, 4.330127018922192761, -2.499999999999997780 ) ) ;
#7221 = ADVANCED_FACE ( 'NONE', ( #9493 ), #17110, .T. ) ;
#7222 = CARTESIAN_POINT ( 'NONE',  ( 25.45312500061451644, -4.541064518000417216, -2.621784821875001281 ) ) ;
#7223 = CARTESIAN_POINT ( 'NONE',  ( 4.243569643749999898, 13.24062500061451786, -27.54997392385601529 ) ) ;
#7224 = CARTESIAN_POINT ( 'NONE',  ( 11.77500000122903501, -5.773502691896255534, -1.060575238724906372E-15 ) ) ;
#7225 = CARTESIAN_POINT ( 'NONE',  ( 23.12812500061451360, -4.541064518000419881, 2.621784821874995952 ) ) ;
#7226 = CARTESIAN_POINT ( 'NONE',  ( 10.27499999999999858, -4.330127018922194537, 2.499999999999995559 ) ) ;
#7227 = CARTESIAN_POINT ( 'NONE',  ( 19.97812500061451502, -4.541064518000419881, 2.621784821874995952 ) ) ;
#7228 = CARTESIAN_POINT ( 'NONE',  ( 5.934375000614517504, 4.541064518000418104, 2.621784821874999949 ) ) ;
#7229 = CARTESIAN_POINT ( 'NONE',  ( 20.54999999999999716, 0.000000000000000000, 4.999999999999998224 ) ) ;
#7230 = CARTESIAN_POINT ( 'NONE',  ( 14.55000000122903181, -2.886751345948125991, -5.000000000000000000 ) ) ;
#7231 = CARTESIAN_POINT ( 'NONE',  ( 10.07812500061451644, -4.541064518000419881, 2.621784821874995952 ) ) ;
#7232 = CARTESIAN_POINT ( 'NONE',  ( 14.65312500061451573, -4.541064518000417216, -2.621784821875001281 ) ) ;
#7233 =( BOUNDED_CURVE ( )  B_SPLINE_CURVE ( 2, ( #26791, #9789, #55952, #43781, #22328, #44880, #50052, #5348, #60752 ),
 .UNSPECIFIED., .F., .F. ) 
 B_SPLINE_CURVE_WITH_KNOTS ( ( 3, 2, 2, 2, 3 ),
 ( 0.4673913043478261087, 0.4710144927536231707, 0.4782608695652174058, 0.4855072463768115854, 0.4891304347826087029 ),
 .UNSPECIFIED. ) 
 CURVE ( )  GEOMETRIC_REPRESENTATION_ITEM ( )  RATIONAL_B_SPLINE_CURVE ( ( 0.9330127018922194093, 0.9330127018922198534, 1.000000000000000000, 0.8660254037844387076, 1.000000000000000000, 0.8660254037844387076, 1.000000000000000000, 0.9330127018922194093, 0.9330127018922194093 ) ) 
 REPRESENTATION_ITEM ( '' )  );
#7234 = CARTESIAN_POINT ( 'NONE',  ( 25.27500000122903145, -5.773502691896255534, -1.060575238724906372E-15 ) ) ;
#7235 = CARTESIAN_POINT ( 'NONE',  ( 21.07499999999999929, -4.330127018922194537, 2.499999999999995559 ) ) ;
#7236 = CARTESIAN_POINT ( 'NONE',  ( 23.14687500061451786, -3.027376345333614438, 5.243569643749998122 ) ) ;
#7237 = CARTESIAN_POINT ( 'NONE',  ( 1.138803498474273873E-14, 15.98750000000000249, 34.00000000000000000 ) ) ;
#7238 = CARTESIAN_POINT ( 'NONE',  ( 6.637500001229035718, 4.330127018922191873, 2.499999999999999556 ) ) ;
#7239 = CARTESIAN_POINT ( 'NONE',  ( 7.921875000614517326, -6.054752690667223547, -1.112240025338166033E-15 ) ) ;
#7240 = CARTESIAN_POINT ( 'NONE',  ( 25.92187500061451999, -6.054752690667223547, -1.112240025338166033E-15 ) ) ;
#7241 = CARTESIAN_POINT ( 'NONE',  ( 23.81250000122903288, 0.000000000000000000, 4.999999999999998224 ) ) ;
#7242 = CARTESIAN_POINT ( 'NONE',  ( 21.70312500061451644, 0.000000000000000000, 5.243569643749999010 ) ) ;
#7243 = CARTESIAN_POINT ( 'NONE',  ( 25.62187500061451573, 3.027376345333613106, -5.243569643749998122 ) ) ;
#7244 = CARTESIAN_POINT ( 'NONE',  ( -7.967954043666661671E-16, 16.69062499938548427, 34.33755215474603517 ) ) ;
#7245 = CARTESIAN_POINT ( 'NONE',  ( 30.00000000000000000, 0.000000000000000000, 0.000000000000000000 ) ) ;
#7246 = CARTESIAN_POINT ( 'NONE',  ( 7.846875000614518036, -3.027376345333614438, 5.243569643749998122 ) ) ;
#7247 = CARTESIAN_POINT ( 'NONE',  ( 19.56562500061451715, -6.054752690667223547, -1.112240025338166033E-15 ) ) ;
#7248 = ORIENTED_EDGE ( 'NONE', *, *, #48306, .F. ) ;
#7249 = DIRECTION ( 'NONE',  ( 0.000000000000000000, 0.000000000000000000, -1.000000000000000000 ) ) ;
#7250 = CARTESIAN_POINT ( 'NONE',  ( 27.59062500061451573, -3.027376345333614438, 5.243569643749998122 ) ) ;
#7251 = CARTESIAN_POINT ( 'NONE',  ( 4.771875000614516971, -6.054752690667223547, -1.112240025338166033E-15 ) ) ;
#7252 = DIRECTION ( 'NONE',  ( -1.000000000000000000, -0.000000000000000000, -0.000000000000000000 ) ) ;
#7253 = EDGE_CURVE ( 'NONE', #16300, #9370, #66130, .T. ) ;
#7254 = CARTESIAN_POINT ( 'NONE',  ( 27.65625000122902932, 4.330127018922192761, -2.499999999999997780 ) ) ;
#7255 = CARTESIAN_POINT ( 'NONE',  ( 17.88749999999999929, -2.886751345948129988, 4.999999999999997335 ) ) ;
#7256 = CARTESIAN_POINT ( 'NONE',  ( 21.17812500061451431, 4.541064518000418104, 2.621784821874999949 ) ) ;
#7257 = EDGE_LOOP ( 'NONE', ( #67652, #45941, #46966, #14399 ) ) ;
#7258 = CARTESIAN_POINT ( 'NONE',  ( 23.92499999999999716, 6.123233995736764310E-16, -4.999999999999998224 ) ) ;
#7259 = CARTESIAN_POINT ( 'NONE',  ( 25.88437500061451502, -4.541064518000419881, 2.621784821874995952 ) ) ;
#7260 = ORIENTED_EDGE ( 'NONE', *, *, #51252, .T. ) ;
#7261 = CARTESIAN_POINT ( 'NONE',  ( 15.81562500061451537, 3.027376345333611329, 5.243569643749999010 ) ) ;
#7262 = CARTESIAN_POINT ( 'NONE',  ( 5.990625000614517859, -3.027376345333614438, 5.243569643749998122 ) ) ;
#7263 = CARTESIAN_POINT ( 'NONE',  ( 17.93437500061451573, 5.492252693125287522, 3.363034840372157021E-16 ) ) ;
#7264 = CARTESIAN_POINT ( 'NONE',  ( 28.86562500061451786, 3.027376345333611329, 5.243569643749999010 ) ) ;
#7265 = CARTESIAN_POINT ( 'NONE',  ( 15.30000000122903359, -2.886751345948129988, 4.999999999999997335 ) ) ;
#7266 = CARTESIAN_POINT ( 'NONE',  ( 21.37499999999999645, 4.330127018922191873, 2.499999999999999556 ) ) ;
#7267 = CARTESIAN_POINT ( 'NONE',  ( 16.50000000000000000, 0.000000000000000000, 4.999999999999998224 ) ) ;
#7268 = CARTESIAN_POINT ( 'NONE',  ( 5.221875000614519813, -6.054752690667223547, -1.112240025338166033E-15 ) ) ;
#7269 = CARTESIAN_POINT ( 'NONE',  ( 9.346875000614517148, -3.027376345333610441, -5.243569643749999898 ) ) ;
#7270 = CARTESIAN_POINT ( 'NONE',  ( 20.37187500061451573, 3.027376345333611329, 5.243569643749999010 ) ) ;
#7271 = FACE_OUTER_BOUND ( 'NONE', #7177, .T. ) ;
#7272 = VERTEX_POINT ( 'NONE', #53832 ) ;
#7273 = CARTESIAN_POINT ( 'NONE',  ( 27.85312500061451502, 4.541064518000418104, -2.621784821874998173 ) ) ;
#7274 = CARTESIAN_POINT ( 'NONE',  ( 29.74687500061451217, 6.054752690667223547, 3.707466751127219781E-16 ) ) ;
#7275 = CARTESIAN_POINT ( 'NONE',  ( 4.284375000614518925, -4.541064518000419881, 2.621784821874995952 ) ) ;
#7276 = CARTESIAN_POINT ( 'NONE',  ( 17.77499999999999858, 4.330127018922191873, 2.499999999999999556 ) ) ;
#7277 = CARTESIAN_POINT ( 'NONE',  ( 13.22812500061451502, -4.541064518000419881, 2.621784821874995952 ) ) ;
#7278 = CARTESIAN_POINT ( 'NONE',  ( 1.071796769724489895, 14.12990381179669797, 26.00000000000000355 ) ) ;
#7280 = DIRECTION ( 'NONE',  ( 0.000000000000000000, 0.000000000000000000, -1.000000000000000000 ) ) ;
#7279 = AXIS2_PLACEMENT_3D ( 'NONE', #70807, #42374, #18721 ) ;
#7281 = CARTESIAN_POINT ( 'NONE',  ( 45.00000000000000000, 0.000000000000000000, 0.000000000000000000 ) ) ;
#7282 = CARTESIAN_POINT ( 'NONE',  ( 19.35937500061451644, 4.119189519843966529, -2.378215178124998275 ) ) ;
#7283 = CARTESIAN_POINT ( 'NONE',  ( 7.190625000614518036, 6.054752690667223547, 3.707466751127219781E-16 ) ) ;
#7284 = CARTESIAN_POINT ( 'NONE',  ( 25.02187500061451431, -6.054752690667223547, -1.112240025338166033E-15 ) ) ;
#7285 = CARTESIAN_POINT ( 'NONE',  ( 4.243569643749999010, 18.32187500061451502, 27.54997392385601174 ) ) ;
#7286 = CARTESIAN_POINT ( 'NONE',  ( 26.48437500061451644, 6.421520780324663323E-16, -5.243569643749999010 ) ) ;
#7287 = CARTESIAN_POINT ( 'NONE',  ( 6.450000000000001066, 4.330127018922192761, -2.499999999999997780 ) ) ;
#7288 = CARTESIAN_POINT ( 'NONE',  ( 3.999999999999999112, 14.03750000122903430, 30.00000000000000000 ) ) ;
#7289 = CARTESIAN_POINT ( 'NONE',  ( 15.59062500061451573, -3.027376345333610441, -5.243569643749999898 ) ) ;
#7290 = CARTESIAN_POINT ( 'NONE',  ( 7.912500001229033408, 4.330127018922192761, -2.499999999999997780 ) ) ;
#7291 = CARTESIAN_POINT ( 'NONE',  ( 18.00937500061451502, 4.541064518000418104, -2.621784821874998173 ) ) ;
#7292 = CARTESIAN_POINT ( 'NONE',  ( 11.22187500061451892, 3.027376345333613106, -5.243569643749998122 ) ) ;
#7293 = ORIENTED_EDGE ( 'NONE', *, *, #41790, .F. ) ;
#7294 = CARTESIAN_POINT ( 'NONE',  ( 11.54062500061451857, -3.027376345333610441, -5.243569643749999898 ) ) ;
#7295 = CARTESIAN_POINT ( 'NONE',  ( 0.000000000000000000, 27.50000000000000000, 26.00000000000000000 ) ) ;
#7296 = CARTESIAN_POINT ( 'NONE',  ( 23.43750000122902932, -4.330127018922194537, 2.499999999999995559 ) ) ;
#7297 = CARTESIAN_POINT ( 'NONE',  ( 12.75937500061451857, 0.000000000000000000, 5.243569643749999010 ) ) ;
#7298 = CARTESIAN_POINT ( 'NONE',  ( 15.59062500061451573, -3.027376345333610441, -5.243569643749999898 ) ) ;
#7299 = CARTESIAN_POINT ( 'NONE',  ( 1.626862140677534273E-15, 16.51249999999999929, -26.00000000000000355 ) ) ;
#7300 = CARTESIAN_POINT ( 'NONE',  ( 24.19687500061451857, -3.027376345333610441, -5.243569643749999898 ) ) ;
#7301 = CARTESIAN_POINT ( 'NONE',  ( 12.45000000122903394, 5.773502691896255534, 3.535250795749688894E-16 ) ) ;
#7302 = DIRECTION ( 'NONE',  ( 0.000000000000000000, 0.000000000000000000, 1.000000000000000000 ) ) ;
#7303 = CARTESIAN_POINT ( 'NONE',  ( 22.66875000122903216, 2.886751345948129099, -4.999999999999997335 ) ) ;
#7304 = CARTESIAN_POINT ( 'NONE',  ( -4.243569643749998122, 16.29687500061451644, -27.54997392385601174 ) ) ;
#7305 = CARTESIAN_POINT ( 'NONE',  ( 19.20937500061451786, -4.541064518000417216, -2.621784821875001281 ) ) ;
#7306 = CARTESIAN_POINT ( 'NONE',  ( 18.18750000122903288, 6.123233995736764310E-16, -4.999999999999998224 ) ) ;
#7307 = EDGE_CURVE ( 'NONE', #13801, #14992, #60516, .T. ) ;
#7308 = CARTESIAN_POINT ( 'NONE',  ( 12.12187500061451573, 3.027376345333613106, -5.243569643749998122 ) ) ;
#7309 = CARTESIAN_POINT ( 'NONE',  ( 4.243569643749999010, 19.61562500061451431, -32.45002607614398471 ) ) ;
#7310 = CARTESIAN_POINT ( 'NONE',  ( 20.13750000122903216, 4.330127018922191873, 2.499999999999999556 ) ) ;
#7311 = CARTESIAN_POINT ( 'NONE',  ( 13.90312500061451750, 4.541064518000418104, -2.621784821874998173 ) ) ;
#7312 = ORIENTED_EDGE ( 'NONE', *, *, #16702, .F. ) ;
#7313 = ORIENTED_EDGE ( 'NONE', *, *, #34980, .T. ) ;
#7314 = CARTESIAN_POINT ( 'NONE',  ( 17.17500000000000071, 6.123233995736764310E-16, -4.999999999999998224 ) ) ;
#7315 = CARTESIAN_POINT ( 'NONE',  ( 1.999999999999997335, 14.22499999999999964, 33.46410161513775705 ) ) ;
#7316 = DIRECTION ( 'NONE',  ( -0.000000000000000000, -1.000000000000000000, -0.000000000000000000 ) ) ;
#7317 = CARTESIAN_POINT ( 'NONE',  ( 15.86250000122903181, -4.330127018922190985, -2.500000000000001332 ) ) ;
#7318 = CARTESIAN_POINT ( 'NONE',  ( 25.99687500061451928, -3.027376345333610441, -5.243569643749999898 ) ) ;
#7319 = CARTESIAN_POINT ( 'NONE',  ( 20.39062500061451644, -3.027376345333614438, 5.243569643749998122 ) ) ;
#7320 = CARTESIAN_POINT ( 'NONE',  ( 23.05312500061451431, 0.000000000000000000, 5.243569643749999010 ) ) ;
#7321 = CARTESIAN_POINT ( 'NONE',  ( 29.40000000122903145, -2.886751345948125991, -5.000000000000000000 ) ) ;
#7322 = CARTESIAN_POINT ( 'NONE',  ( 27.41250000000000142, -5.773502691896255534, -1.060575238724906372E-15 ) ) ;
#7323 = CARTESIAN_POINT ( 'NONE',  ( 17.68125000122903501, 6.123233995736764310E-16, -4.999999999999998224 ) ) ;
#7324 = CARTESIAN_POINT ( 'NONE',  ( 9.346875000614517148, -2.746126346562642428, -4.756430356249999214 ) ) ;
#7325 = CYLINDRICAL_SURFACE ( 'NONE', #45318, 3.999999999999996447 ) ;
#7326 = CARTESIAN_POINT ( 'NONE',  ( 3.999999999999999112, 9.987500001229033586, -30.00000000000000000 ) ) ;
#7327 = CARTESIAN_POINT ( 'NONE',  ( -4.243569643749999898, 15.35937500061451644, -30.00000000000000000 ) ) ;
#7328 = CARTESIAN_POINT ( 'NONE',  ( 6.900000001229035007, -2.886751345948125991, -5.000000000000000000 ) ) ;
#7329 = CARTESIAN_POINT ( 'NONE',  ( 5.025000000000002132, 6.123233995736764310E-16, -4.999999999999998224 ) ) ;
#7330 = CARTESIAN_POINT ( 'NONE',  ( 2.934375000614518392, -4.541064518000419881, 2.621784821874995952 ) ) ;
#7331 = CARTESIAN_POINT ( 'NONE',  ( 10.62187500061451928, -6.054752690667223547, -1.112240025338166033E-15 ) ) ;
#7332 = CIRCLE ( 'NONE', #48642, 9.000000000000000000 ) ;
#7333 = CARTESIAN_POINT ( 'NONE',  ( 28.79062500061451502, 6.054752690667223547, 3.707466751127219781E-16 ) ) ;
#7334 = DIRECTION ( 'NONE',  ( -0.000000000000000000, -1.000000000000000000, -0.000000000000000000 ) ) ;
#7335 = CARTESIAN_POINT ( 'NONE',  ( 3.619842856578028734, -3.449164782042274169, -3.619842856578066481 ) ) ;
#7336 = CARTESIAN_POINT ( 'NONE',  ( -3.999999999999999112, 19.17500000122903359, 27.69059892324149885 ) ) ;
#7337 = CARTESIAN_POINT ( 'NONE',  ( 7.734375000614517326, 4.541064518000418104, 2.621784821874999949 ) ) ;
#7338 = CARTESIAN_POINT ( 'NONE',  ( 11.70937500061451608, 4.541064518000418104, -2.621784821874998173 ) ) ;
#7339 = CARTESIAN_POINT ( 'NONE',  ( 6.075000000000000178, 4.330127018922191873, 2.499999999999999556 ) ) ;
#7340 = CARTESIAN_POINT ( 'NONE',  ( -4.243569643749999898, 13.95312500061459282, 30.00000000000000000 ) ) ;
#7341 = CARTESIAN_POINT ( 'NONE',  ( 3.973779386032386007, 25.00705285313813775, 30.52704257968602874 ) ) ;
#7342 = CARTESIAN_POINT ( 'NONE',  ( 5.812500000000001776, -5.773502691896255534, -1.060575238724906372E-15 ) ) ;
#7343 = CARTESIAN_POINT ( 'NONE',  ( 27.52500000122903145, -5.773502691896255534, -1.060575238724906372E-15 ) ) ;
#7344 = CARTESIAN_POINT ( 'NONE',  ( 17.70937500061451786, -5.492252693125287522, -1.008910452111647106E-15 ) ) ;
#7345 = CARTESIAN_POINT ( 'NONE',  ( 22.07812500061451644, 4.541064518000418104, 2.621784821874999949 ) ) ;
#7346 = CARTESIAN_POINT ( 'NONE',  ( 13.60312500061451679, 0.000000000000000000, 5.243569643749999010 ) ) ;
#7347 = CARTESIAN_POINT ( 'NONE',  ( 25.47187500061451360, 5.824947211148865298E-16, -4.756430356249998326 ) ) ;
#7348 = CARTESIAN_POINT ( 'NONE',  ( 10.17187500061451999, -6.054752690667223547, -1.112240025338166033E-15 ) ) ;
#7349 = CARTESIAN_POINT ( 'NONE',  ( 26.92499999999999716, -4.330127018922194537, 2.499999999999995559 ) ) ;
#7350 = CARTESIAN_POINT ( 'NONE',  ( 21.37500000122902932, 2.886751345948129099, -4.999999999999998224 ) ) ;
#7351 = CARTESIAN_POINT ( 'NONE',  ( 0.000000000000000000, -10.00000000000000000, 0.000000000000000000 ) ) ;
#7352 = CARTESIAN_POINT ( 'NONE',  ( 12.83437500061451786, -4.541064518000419881, 2.621784821874995952 ) ) ;
#7353 = CARTESIAN_POINT ( 'NONE',  ( 26.37187500061451217, -6.054752690667223547, -1.112240025338166033E-15 ) ) ;
#7354 = CARTESIAN_POINT ( 'NONE',  ( 3.196875000614516793, 6.054752690667223547, 3.707466751127219781E-16 ) ) ;
#7355 = CARTESIAN_POINT ( 'NONE',  ( 3.999999999999998668, 13.62500000122903465, -32.30940107675850470 ) ) ;
#7356 = CARTESIAN_POINT ( 'NONE',  ( 22.02187500061452141, 3.027376345333613106, -5.243569643749998122 ) ) ;
#7357 = CARTESIAN_POINT ( 'NONE',  ( 11.82187500061451679, 3.027376345333611329, 5.243569643749999010 ) ) ;
#7358 = CARTESIAN_POINT ( 'NONE',  ( -3.756430356249999214, 19.24062499938548143, 27.83122392262697531 ) ) ;
#7359 = CARTESIAN_POINT ( 'NONE',  ( 25.64999999999999858, -4.330127018922190985, -2.500000000000001332 ) ) ;
#7360 = CARTESIAN_POINT ( 'NONE',  ( 1.878215178125000495, 20.36562499938548143, 26.74683588394047007 ) ) ;
#7361 = CARTESIAN_POINT ( 'NONE',  ( -2.121784821874999949, 13.03437500061451715, -33.67503911421598417 ) ) ;
#7362 = CARTESIAN_POINT ( 'NONE',  ( 26.93437500061451573, 5.824947211148865298E-16, -4.756430356249998326 ) ) ;
#7363 = CARTESIAN_POINT ( 'NONE',  ( 13.71562500061451750, -6.054752690667223547, -1.112240025338166033E-15 ) ) ;
#7364 = CARTESIAN_POINT ( 'NONE',  ( 6.037500000000001421, 5.773502691896255534, 3.535250795749688894E-16 ) ) ;
#7365 = CARTESIAN_POINT ( 'NONE',  ( 0.000000000000000000, 20.00000000000000000, -30.00000000000000000 ) ) ;
#7366 = CARTESIAN_POINT ( 'NONE',  ( 15.37500000000000000, 6.123233995736764310E-16, -4.999999999999998224 ) ) ;
#7367 = CARTESIAN_POINT ( 'NONE',  ( -2.121784821874999949, 11.17812500061451786, 26.32496088578401938 ) ) ;
#7368 = CARTESIAN_POINT ( 'NONE',  ( 14.40000000122903323, -2.886751345948129988, 4.999999999999997335 ) ) ;
#7369 = CARTESIAN_POINT ( 'NONE',  ( 25.35937500061451644, 0.000000000000000000, 5.243569643749999010 ) ) ;
#7370 = ORIENTED_EDGE ( 'NONE', *, *, #56475, .F. ) ;
#7371 = CARTESIAN_POINT ( 'NONE',  ( 19.15312500061451573, -4.541064518000417216, -2.621784821875001281 ) ) ;
#7372 = CARTESIAN_POINT ( 'NONE',  ( 20.85937500061451644, 0.000000000000000000, 5.243569643749999010 ) ) ;
#7373 = CARTESIAN_POINT ( 'NONE',  ( 5.362500000000003375, -5.773502691896255534, -1.060575238724906372E-15 ) ) ;
#7374 = CARTESIAN_POINT ( 'NONE',  ( 7.490625000614516082, -3.027376345333610441, -5.243569643749999898 ) ) ;
#7375 = CARTESIAN_POINT ( 'NONE',  ( 21.70312500061451644, 0.000000000000000000, 5.243569643749999010 ) ) ;
#7376 = CARTESIAN_POINT ( 'NONE',  ( 15.98437500061451821, -4.541064518000419881, 2.621784821874995952 ) ) ;
#7377 = CARTESIAN_POINT ( 'NONE',  ( 2.121784821874999061, 14.70312500061451644, 26.32496088578401583 ) ) ;
#7378 = CARTESIAN_POINT ( 'NONE',  ( 19.08750000122903145, 6.123233995736764310E-16, -4.999999999999998224 ) ) ;
#7379 = CARTESIAN_POINT ( 'NONE',  ( 12.19687500061451857, 5.492252693125287522, 3.363034840372157021E-16 ) ) ;
#7380 = CARTESIAN_POINT ( 'NONE',  ( 8.540625000614518569, 6.054752690667223547, 3.707466751127219781E-16 ) ) ;
#7381 = CARTESIAN_POINT ( 'NONE',  ( 3.234375000614516438, 4.541064518000418104, 2.621784821874999949 ) ) ;
#7382 = CARTESIAN_POINT ( 'NONE',  ( 29.61562500061451431, 3.027376345333613106, -5.243569643749998122 ) ) ;
#7383 =( BOUNDED_CURVE ( )  B_SPLINE_CURVE ( 2, ( #57536, #25649, #36725, #62718, #35365, #12112, #30822 ),
 .UNSPECIFIED., .F., .F. ) 
 B_SPLINE_CURVE_WITH_KNOTS ( ( 3, 2, 2, 3 ),
 ( 0.9599923174713632656, 0.9611111111111111382, 0.9638888888888889062, 0.9649074199495660809 ),
 .UNSPECIFIED. ) 
 CURVE ( )  GEOMETRIC_REPRESENTATION_ITEM ( )  RATIONAL_B_SPLINE_CURVE ( ( 0.9355460294322659465, 0.9460396265918464831, 1.000000000000000000, 0.8660254037844387076, 1.000000000000000000, 0.9508753764685963228, 0.9377759204729740894 ) ) 
 REPRESENTATION_ITEM ( '' )  );
#7384 = CARTESIAN_POINT ( 'NONE',  ( 25.43437500061451573, -4.541064518000419881, 2.621784821874995952 ) ) ;
#7385 = CARTESIAN_POINT ( 'NONE',  ( 16.79062500061451857, -3.027376345333614438, 5.243569643749998122 ) ) ;
#7386 = CARTESIAN_POINT ( 'NONE',  ( 24.48750000122903359, 6.123233995736764310E-16, -4.999999999999998224 ) ) ;
#7387 = EDGE_CURVE ( 'NONE', #43953, #14078, #10905, .T. ) ;
#7388 = CARTESIAN_POINT ( 'NONE',  ( 25.15312500061451217, 4.541064518000418104, -2.621784821874998173 ) ) ;
#7389 = VECTOR ( 'NONE', #67578, 1000.000000000000000 ) ;
#7390 = CARTESIAN_POINT ( 'NONE',  ( 20.93437500061451573, -4.541064518000419881, 2.621784821874995952 ) ) ;
#7391 = CARTESIAN_POINT ( 'NONE',  ( 14.76562500061451821, 3.027376345333613106, -5.243569643749998122 ) ) ;
#7392 = CARTESIAN_POINT ( 'NONE',  ( -4.243569643749999898, 18.02187500061452141, 27.54997392385601529 ) ) ;
#7393 = CARTESIAN_POINT ( 'NONE',  ( 21.51562500061451644, 3.027376345333613106, -5.243569643749998122 ) ) ;
#7394 = LINE ( 'NONE', #41025, #64475 ) ;
#7395 = ORIENTED_EDGE ( 'NONE', *, *, #33218, .T. ) ;
#7396 = CARTESIAN_POINT ( 'NONE',  ( 24.75000000000000000, -4.330127018922190985, -2.500000000000001332 ) ) ;
#7397 = CARTESIAN_POINT ( 'NONE',  ( -3.999999999999999112, 12.80000000000000071, -30.00000000000000000 ) ) ;
#7398 = CARTESIAN_POINT ( 'NONE',  ( 3.756430356250000102, 19.50312499938548072, 30.00000000000000000 ) ) ;
#7399 = CARTESIAN_POINT ( 'NONE',  ( 3.421875000614516882, -6.054752690667223547, -1.112240025338166033E-15 ) ) ;
#7400 = CARTESIAN_POINT ( 'NONE',  ( 6.853125000614516793, 0.000000000000000000, 5.243569643749999010 ) ) ;
#7401 = CARTESIAN_POINT ( 'NONE',  ( 21.18750000122903288, -4.330127018922194537, 2.499999999999995559 ) ) ;
#7402 = CARTESIAN_POINT ( 'NONE',  ( 26.20312500061451644, 0.000000000000000000, 5.243569643749999010 ) ) ;
#7403 = CARTESIAN_POINT ( 'NONE',  ( 24.63749999999999574, -2.886751345948129988, 4.999999999999997335 ) ) ;
#7404 = CARTESIAN_POINT ( 'NONE',  ( -1.999999999999997113, 15.23750000122903536, -26.53589838486224295 ) ) ;
#7405 = CARTESIAN_POINT ( 'NONE',  ( 65.00000000000000000, 6.363961030679004871, 4.863961030678849440 ) ) ;
#7406 = CARTESIAN_POINT ( 'NONE',  ( 10.60312500061451679, -4.541064518000417216, -2.621784821875001281 ) ) ;
#7407 = ORIENTED_EDGE ( 'NONE', *, *, #29897, .F. ) ;
#7408 = CARTESIAN_POINT ( 'NONE',  ( 25.82812500061451644, -4.541064518000419881, 2.621784821874995952 ) ) ;
#7409 = CARTESIAN_POINT ( 'NONE',  ( 7.190625000614518036, 6.054752690667223547, 3.707466751127219781E-16 ) ) ;
#7410 = CARTESIAN_POINT ( 'NONE',  ( 3.815625000614518036, -6.054752690667223547, -1.112240025338166033E-15 ) ) ;
#7411 = CARTESIAN_POINT ( 'NONE',  ( 16.43437500061451573, -4.119189519843968306, 2.378215178124996054 ) ) ;
#7412 = CYLINDRICAL_SURFACE ( 'NONE', #32657, 4.999999999999998224 ) ;
#7413 = CARTESIAN_POINT ( 'NONE',  ( 13.35000000000000142, 0.000000000000000000, 4.999999999999998224 ) ) ;
#7414 = CARTESIAN_POINT ( 'NONE',  ( 12.87187500061451750, -6.054752690667223547, -1.112240025338166033E-15 ) ) ;
#7415 = CARTESIAN_POINT ( 'NONE',  ( 9.750000001229032875, 5.773502691896255534, 3.535250795749688894E-16 ) ) ;
#7416 = CARTESIAN_POINT ( 'NONE',  ( 16.13437500061451502, 6.421520780324663323E-16, -5.243569643749999010 ) ) ;
#7417 = CARTESIAN_POINT ( 'NONE',  ( 16.53750000000000142, -2.886751345948129988, 4.999999999999997335 ) ) ;
#7418 = CARTESIAN_POINT ( 'NONE',  ( 8.409375000614518925, -4.541064518000417216, -2.621784821875001281 ) ) ;
#7419 = CARTESIAN_POINT ( 'NONE',  ( -4.243569643749999898, 12.11562500061451608, -32.45002607614398471 ) ) ;
#7420 = CARTESIAN_POINT ( 'NONE',  ( -3.999999999999997335, 16.88749999999999929, 32.30940107675850470 ) ) ;
#7421 = CARTESIAN_POINT ( 'NONE',  ( 23.85937500061451644, 2.746126346562643317, 4.756430356249998326 ) ) ;
#7422 = EDGE_LOOP ( 'NONE', ( #35380, #4511, #41457, #34982 ) ) ;
#7423 = CARTESIAN_POINT ( 'NONE',  ( 23.65312500061451573, -4.541064518000417216, -2.621784821875001281 ) ) ;
#7424 = CARTESIAN_POINT ( 'NONE',  ( 0.000000000000000000, 20.00000000000000000, 30.00000000000000000 ) ) ;
#7425 = CARTESIAN_POINT ( 'NONE',  ( 29.25937500061451502, 4.541064518000418104, -2.621784821874998173 ) ) ;
#7426 =( BOUNDED_CURVE ( )  B_SPLINE_CURVE ( 2, ( #40616, #52061, #13978, #54249, #26169, #3646, #14708, #36516, #65689 ),
 .UNSPECIFIED., .F., .F. ) 
 B_SPLINE_CURVE_WITH_KNOTS ( ( 3, 2, 2, 2, 3 ),
 ( 0.1413043478260869734, 0.1449275362318840632, 0.1521739130434782705, 0.1594202898550724501, 0.1630434782608695676 ),
 .UNSPECIFIED. ) 
 CURVE ( )  GEOMETRIC_REPRESENTATION_ITEM ( )  RATIONAL_B_SPLINE_CURVE ( ( 0.9330127018922194093, 0.9330127018922196314, 1.000000000000000000, 0.8660254037844387076, 1.000000000000000000, 0.8660254037844387076, 1.000000000000000000, 0.9330127018922190762, 0.9330127018922194093 ) ) 
 REPRESENTATION_ITEM ( '' )  );
#7427 = CARTESIAN_POINT ( 'NONE',  ( 24.67500000000000071, -4.330127018922194537, 2.499999999999995559 ) ) ;
#7428 = CARTESIAN_POINT ( 'NONE',  ( 7.153125000614518392, 4.541064518000418104, -2.621784821874998173 ) ) ;
#7429 = B_SPLINE_CURVE_WITH_KNOTS ( 'NONE', 3,
 ( #59358, #1789, #24659, #53844, #24299, #46847, #69387, #13208, #26496, #71567 ),
 .UNSPECIFIED., .F., .F.,
 ( 4, 3, 3, 4 ),
 ( 0.000000000000000000, 0.0001572266096559048090, 0.0003144533513551280631, 0.0005416000942056856159 ),
 .UNSPECIFIED. ) ;
#7430 = CARTESIAN_POINT ( 'NONE',  ( 24.64687500061451431, 4.119189519843966529, -2.378215178124998275 ) ) ;
#7431 = CARTESIAN_POINT ( 'NONE',  ( 16.54687500061451644, -3.027376345333610441, -5.243569643749999898 ) ) ;
#7432 = CARTESIAN_POINT ( 'NONE',  ( 8.746875000614515727, -4.119189519843965641, -2.378215178125001383 ) ) ;
#7433 = CARTESIAN_POINT ( 'NONE',  ( 29.62500000122903288, 2.886751345948126879, 4.999999999999999112 ) ) ;
#7434 = CARTESIAN_POINT ( 'NONE',  ( 9.159375000614515372, 0.000000000000000000, 5.243569643749999010 ) ) ;
#7435 = ORIENTED_EDGE ( 'NONE', *, *, #5292, .T. ) ;
#7436 = CARTESIAN_POINT ( 'NONE',  ( 19.28437500061451360, 6.421520780324663323E-16, -5.243569643749999010 ) ) ;
#7437 = CARTESIAN_POINT ( 'NONE',  ( 4.898850051585143718E-16, 25.54316770519903557, 34.00000000000000000 ) ) ;
#7438 = CARTESIAN_POINT ( 'NONE',  ( 27.82499999999999929, -4.330127018922194537, 2.499999999999995559 ) ) ;
#7439 = CARTESIAN_POINT ( 'NONE',  ( 28.77187500061451431, 3.027376345333613106, -5.243569643749998122 ) ) ;
#7440 = DIRECTION ( 'NONE',  ( -1.000000000000000000, -0.000000000000000000, -0.000000000000000000 ) ) ;
#7441 = CARTESIAN_POINT ( 'NONE',  ( 27.78750000000000142, -2.886751345948155301, 4.999999999999952927 ) ) ;
#7442 = ORIENTED_EDGE ( 'NONE', *, *, #48670, .F. ) ;
#7443 = CARTESIAN_POINT ( 'NONE',  ( 11.02500000000000036, 4.330127018922191873, 2.499999999999999556 ) ) ;
#7444 = CARTESIAN_POINT ( 'NONE',  ( 12.53437500061451537, 5.492252693125287522, 3.363034840372157021E-16 ) ) ;
#7445 = CARTESIAN_POINT ( 'NONE',  ( 25.64062500061451644, 6.054752690667223547, 3.707466751127219781E-16 ) ) ;
#7446 = CARTESIAN_POINT ( 'NONE',  ( 14.47499999999999964, 6.123233995736764310E-16, -4.999999999999998224 ) ) ;
#7447 = CARTESIAN_POINT ( 'NONE',  ( 9.112500001229033586, -4.330127018922190985, -2.500000000000001332 ) ) ;
#7448 = CARTESIAN_POINT ( 'NONE',  ( 7.415625000614516793, -6.054752690667223547, -1.112240025338166033E-15 ) ) ;
#7449 = CARTESIAN_POINT ( 'NONE',  ( 21.75000000000000000, 4.330127018922192761, -2.499999999999997780 ) ) ;
#7450 = CARTESIAN_POINT ( 'NONE',  ( 21.25312500061451715, 0.000000000000000000, 5.243569643749999010 ) ) ;
#7451 = CARTESIAN_POINT ( 'NONE',  ( 23.66250000000000142, 2.886751345948126879, 4.999999999999998224 ) ) ;
#7452 = CARTESIAN_POINT ( 'NONE',  ( 24.75000000122902932, -2.886751345948129988, 4.999999999999997335 ) ) ;
#7453 = CARTESIAN_POINT ( 'NONE',  ( -1.878215178124999163, 18.19062499938548427, 26.74683588394047007 ) ) ;
#7454 = CARTESIAN_POINT ( 'NONE',  ( 6.000000000000001776, 4.330127018922192761, -2.499999999999997780 ) ) ;
#7455 = ORIENTED_EDGE ( 'NONE', *, *, #40125, .T. ) ;
#7456 = CARTESIAN_POINT ( 'NONE',  ( 21.17812500061451431, 4.541064518000418104, 2.621784821874999949 ) ) ;
#7457 = CARTESIAN_POINT ( 'NONE',  ( 27.92812500061451431, 4.541064518000418104, 2.621784821874999949 ) ) ;
#7458 = CARTESIAN_POINT ( 'NONE',  ( 27.23437500061451644, -4.541064518000419881, 2.621784821874995952 ) ) ;
#7459 = EDGE_CURVE ( 'NONE', #42612, #59877, #43498, .T. ) ;
#7460 = CARTESIAN_POINT ( 'NONE',  ( 14.16562500061451679, -6.054752690667223547, -1.112240025338166033E-15 ) ) ;
#7461 = CARTESIAN_POINT ( 'NONE',  ( 12.24375000122902968, -2.886751345948181946, -4.999999999999904077 ) ) ;
#7462 = CARTESIAN_POINT ( 'NONE',  ( 26.36250000122903003, 4.330127018922192761, -2.499999999999997780 ) ) ;
#7463 = CARTESIAN_POINT ( 'NONE',  ( 22.43437500061451573, 5.824947211148865298E-16, -4.756430356249998326 ) ) ;
#7464 = CARTESIAN_POINT ( 'NONE',  ( 17.24062500061451786, -3.027376345333614438, 5.243569643749998122 ) ) ;
#7465 = CARTESIAN_POINT ( 'NONE',  ( -2.000000000000001776, 15.50000000000000000, 33.46410161513775705 ) ) ;
#7466 = CARTESIAN_POINT ( 'NONE',  ( 5.850000001229035185, -2.886751345948130876, 4.999999999999996447 ) ) ;
#7467 = CARTESIAN_POINT ( 'NONE',  ( 10.95937500061451964, 0.000000000000000000, 5.243569643749999010 ) ) ;
#7468 = CARTESIAN_POINT ( 'NONE',  ( 9.496875000614517504, 6.054752690667223547, 3.707466751127219781E-16 ) ) ;
#7469 = CARTESIAN_POINT ( 'NONE',  ( 21.19687500061451502, 6.054752690667223547, 3.707466751127219781E-16 ) ) ;
#7470 = ORIENTED_EDGE ( 'NONE', *, *, #8067, .F. ) ;
#7471 = CARTESIAN_POINT ( 'NONE',  ( -1.974232797588184596, 9.810253314282338266, 24.32048149236734247 ) ) ;
#7472 = CARTESIAN_POINT ( 'NONE',  ( 23.01562500061451644, 3.027376345333611329, 5.243569643749999010 ) ) ;
#7473 = CARTESIAN_POINT ( 'NONE',  ( 19.73437500061451644, 6.421520780324663323E-16, -5.243569643749999010 ) ) ;
#7474 = CARTESIAN_POINT ( 'NONE',  ( 23.39062500061451289, 6.054752690667223547, 3.707466751127219781E-16 ) ) ;
#7475 = CARTESIAN_POINT ( 'NONE',  ( 4.057522967627288146, -2.921730200955767298, 4.057522967627288146 ) ) ;
#7476 = CARTESIAN_POINT ( 'NONE',  ( 1.999999999999998668, 14.00000000000000178, 26.53589838486224650 ) ) ;
#7477 = CARTESIAN_POINT ( 'NONE',  ( 3.009375000614516793, -4.541064518000417216, -2.621784821875001281 ) ) ;
#7478 = CARTESIAN_POINT ( 'NONE',  ( 9.037500001229034297, -4.330127018922194537, 2.499999999999995559 ) ) ;
#7479 = CARTESIAN_POINT ( 'NONE',  ( 5.475000001229035185, -5.773502691896255534, -1.060575238724906372E-15 ) ) ;
#7480 = CARTESIAN_POINT ( 'NONE',  ( -3.999999999999997335, 19.58749999999999858, -27.69059892324149175 ) ) ;
#7481 = CARTESIAN_POINT ( 'NONE',  ( 26.02500000122903145, 2.886751345948126879, 4.999999999999999112 ) ) ;
#7482 = CARTESIAN_POINT ( 'NONE',  ( -1.878215178125001827, 13.05312499938548321, 33.25316411605952283 ) ) ;
#7483 = CARTESIAN_POINT ( 'NONE',  ( 10.09687500061451715, -3.027376345333614438, 5.243569643749998122 ) ) ;
#7484 = CARTESIAN_POINT ( 'NONE',  ( 18.55312500061451431, 0.000000000000000000, 5.243569643749999010 ) ) ;
#7485 = CARTESIAN_POINT ( 'NONE',  ( 9.871875000614517504, 3.027376345333613106, -5.243569643749998122 ) ) ;
#7486 = CARTESIAN_POINT ( 'NONE',  ( 28.98750000122903359, 6.123233995736764310E-16, -4.999999999999998224 ) ) ;
#7487 = CARTESIAN_POINT ( 'NONE',  ( 19.43437500061451928, 4.541064518000418104, 2.621784821874999949 ) ) ;
#7488 = CARTESIAN_POINT ( 'NONE',  ( 7.059375000614518392, -4.541064518000417216, -2.621784821875001281 ) ) ;
#7489 = CARTESIAN_POINT ( 'NONE',  ( 3.138359732036306138, -3.892498296044141437, -3.200804231420348422 ) ) ;
#7490 = CARTESIAN_POINT ( 'NONE',  ( 1.592000809091587073E-14, 16.40000000122903501, 26.00000000000000000 ) ) ;
#7491 = CARTESIAN_POINT ( 'NONE',  ( 8.128125000614515372, 4.541064518000418104, 2.621784821874999949 ) ) ;
#7492 = CARTESIAN_POINT ( 'NONE',  ( 16.75312500061451715, 0.000000000000000000, 5.243569643749999010 ) ) ;
#7493 = EDGE_LOOP ( 'NONE', ( #44255, #52202, #2683, #33376 ) ) ;
#7494 = CARTESIAN_POINT ( 'NONE',  ( 5.700000001229033941, 5.773502691896255534, 3.535250795749688894E-16 ) ) ;
#7495 = CARTESIAN_POINT ( 'NONE',  ( 15.21562500061451750, 3.027376345333613106, -5.243569643749998122 ) ) ;
#7496 = CARTESIAN_POINT ( 'NONE',  ( 10.07812500061451644, -4.541064518000419881, 2.621784821874995952 ) ) ;
#7497 = CARTESIAN_POINT ( 'NONE',  ( 24.34687500061451715, 5.492252693125287522, 3.363034840372157021E-16 ) ) ;
#7498 = CARTESIAN_POINT ( 'NONE',  ( 11.13750000000000284, -2.886751345948129988, 4.999999999999997335 ) ) ;
#7499 = CARTESIAN_POINT ( 'NONE',  ( 5.475000001229035185, -5.773502691896255534, -1.060575238724906372E-15 ) ) ;
#7500 = CARTESIAN_POINT ( 'NONE',  ( 14.70937500061451786, -4.541064518000417216, -2.621784821875001281 ) ) ;
#7501 = CARTESIAN_POINT ( 'NONE',  ( 18.97500000122903074, -5.773502691896255534, -1.060575238724906372E-15 ) ) ;
#7502 = CARTESIAN_POINT ( 'NONE',  ( 24.18750000000000355, -2.886751345948129988, 4.999999999999997335 ) ) ;
#7503 = CARTESIAN_POINT ( 'NONE',  ( 4.243569643749999898, 17.74062500061451786, -27.54997392385601529 ) ) ;
#7504 = CARTESIAN_POINT ( 'NONE',  ( 4.120265700342371495, -2.833395342107308590, -4.120265700342371495 ) ) ;
#7505 = CARTESIAN_POINT ( 'NONE',  ( 12.91875000122903394, 2.886751345948126879, 4.999999999999998224 ) ) ;
#7506 = CARTESIAN_POINT ( 'NONE',  ( 9.450000001229033941, -2.886751345948130876, 4.999999999999996447 ) ) ;
#7507 = DIRECTION ( 'NONE',  ( -1.000000000000000000, -0.000000000000000000, -0.000000000000000000 ) ) ;
#7508 = CARTESIAN_POINT ( 'NONE',  ( 19.39687500061451786, 6.054752690667223547, 3.707466751127219781E-16 ) ) ;
#7509 = CARTESIAN_POINT ( 'NONE',  ( 21.37500000122903288, 2.886751345948129099, -4.999999999999997335 ) ) ;
#7510 = EDGE_CURVE ( 'NONE', #57706, #52280, #50603, .T. ) ;
#7511 = CARTESIAN_POINT ( 'NONE',  ( 14.61562500061451608, -6.054752690667223547, -1.112240025338166033E-15 ) ) ;
#7512 = CARTESIAN_POINT ( 'NONE',  ( 10.51875000122903536, 2.886751345948129099, -4.999999999999998224 ) ) ;
#7513 = CARTESIAN_POINT ( 'NONE',  ( 8.887499999999995737, -2.886751345948019409, 5.000000000000189182 ) ) ;
#7514 = CARTESIAN_POINT ( 'NONE',  ( 25.32187500061451857, 3.027376345333611329, 5.243569643749999010 ) ) ;
#7515 = CARTESIAN_POINT ( 'NONE',  ( 17.37187500061451573, 5.824947211148865298E-16, -4.756430356249998326 ) ) ;
#7516 = CARTESIAN_POINT ( 'NONE',  ( 10.11562500061451608, -6.054752690667223547, -1.112240025338166033E-15 ) ) ;
#7517 = CARTESIAN_POINT ( 'NONE',  ( 16.02187500061451786, -6.054752690667223547, -1.112240025338166033E-15 ) ) ;
#7518 = ORIENTED_EDGE ( 'NONE', *, *, #5067, .T. ) ;
#7519 = CARTESIAN_POINT ( 'NONE',  ( 25.09687500061451715, -3.027376345333610441, -5.243569643749999898 ) ) ;
#7520 = CARTESIAN_POINT ( 'NONE',  ( 26.50312500061451360, 4.541064518000418104, -2.621784821874998173 ) ) ;
#7521 = CARTESIAN_POINT ( 'NONE',  ( 19.94062500061451715, -3.027376345333614438, 5.243569643749998122 ) ) ;
#7522 = CARTESIAN_POINT ( 'NONE',  ( 29.65312500061451573, 4.541064518000418104, -2.621784821874998173 ) ) ;
#7523 = DIRECTION ( 'NONE',  ( 1.000000000000000000, 0.000000000000000000, 0.000000000000000000 ) ) ;
#7524 = CARTESIAN_POINT ( 'NONE',  ( 10.57500000000000107, 4.330127018922191873, 2.499999999999999556 ) ) ;
#7525 = CARTESIAN_POINT ( 'NONE',  ( 19.50000000122903288, -2.886751345948125991, -5.000000000000000000 ) ) ;
#7526 = CARTESIAN_POINT ( 'NONE',  ( 1.999999999999998668, 10.40000000000000213, 26.53589838486224650 ) ) ;
#7527 = CARTESIAN_POINT ( 'NONE',  ( 9.459375000614519635, 2.746126346562643317, 4.756430356249998326 ) ) ;
#7528 = VERTEX_POINT ( 'NONE', #40380 ) ;
#7529 = CARTESIAN_POINT ( 'NONE',  ( 18.71249999999999858, 2.886751345948126879, 4.999999999999999112 ) ) ;
#7530 = CARTESIAN_POINT ( 'NONE',  ( 22.38749999999999929, -2.886751345948129988, 4.999999999999997335 ) ) ;
#7531 = CARTESIAN_POINT ( 'NONE',  ( 19.02187500061451786, 3.027376345333611329, 5.243569643749999010 ) ) ;
#7532 = CARTESIAN_POINT ( 'NONE',  ( 13.67812500061451786, -4.541064518000419881, 2.621784821874995952 ) ) ;
#7533 = ORIENTED_EDGE ( 'NONE', *, *, #8440, .T. ) ;
#7534 = CARTESIAN_POINT ( 'NONE',  ( 1.999999999999998668, 18.61250000122903359, -33.46410161513775705 ) ) ;
#7535 = CARTESIAN_POINT ( 'NONE',  ( 6.515625000614516438, -6.054752690667223547, -1.112240025338166033E-15 ) ) ;
#7536 = CARTESIAN_POINT ( 'NONE',  ( 13.38750000000000107, -2.886751345948129988, 4.999999999999997335 ) ) ;
#7537 = CARTESIAN_POINT ( 'NONE',  ( 27.68437500061451573, -2.746126346562642428, -4.756430356249999214 ) ) ;
#7538 = CARTESIAN_POINT ( 'NONE',  ( -4.243569643749999898, 15.75312500061451537, 30.00000000000000000 ) ) ;
#7539 = CARTESIAN_POINT ( 'NONE',  ( 29.31562500061451715, 3.027376345333611329, 5.243569643749999010 ) ) ;
#7540 = CARTESIAN_POINT ( 'NONE',  ( 8.812500000000000000, 2.886751345948126879, 4.999999999999999112 ) ) ;
#7541 = CARTESIAN_POINT ( 'NONE',  ( 1.878215178124997609, 16.61562499938548143, 33.25316411605952993 ) ) ;
#7542 = CARTESIAN_POINT ( 'NONE',  ( 25.05937500061451573, -4.541064518000417216, -2.621784821875001281 ) ) ;
#7543 = ORIENTED_EDGE ( 'NONE', *, *, #17037, .F. ) ;
#7544 = CARTESIAN_POINT ( 'NONE',  ( 21.06562500061451715, 3.027376345333613106, -5.243569643749998122 ) ) ;
#7545 = CARTESIAN_POINT ( 'NONE',  ( 23.85937500061451644, 4.541064518000418104, -2.621784821874998173 ) ) ;
#7546 = CARTESIAN_POINT ( 'NONE',  ( 2.121784821874999061, 17.40312500061459389, -33.67503911421598417 ) ) ;
#7547 = CARTESIAN_POINT ( 'NONE',  ( 6.815625000614517148, 3.027376345333611329, 5.243569643749999010 ) ) ;
#7548 = CARTESIAN_POINT ( 'NONE',  ( 29.52187500061451431, -5.492252693125287522, -1.008910452111647106E-15 ) ) ;
#7549 = CARTESIAN_POINT ( 'NONE',  ( 25.04062500061451502, -3.027376345333610441, -5.243569643749999898 ) ) ;
#7550 = CARTESIAN_POINT ( 'NONE',  ( 27.42187500061451289, 4.119189519843966529, 2.378215178124999607 ) ) ;
#7551 = CARTESIAN_POINT ( 'NONE',  ( 9.946875000614516793, 5.492252693125287522, 3.363034840372157021E-16 ) ) ;
#7552 = CARTESIAN_POINT ( 'NONE',  ( 17.48437500061451999, 6.421520780324663323E-16, -5.243569643749999010 ) ) ;
#7553 = CARTESIAN_POINT ( 'NONE',  ( 18.38437500061451857, 6.421520780324663323E-16, -5.243569643749999010 ) ) ;
#7554 = CARTESIAN_POINT ( 'NONE',  ( 27.23437500061451644, -4.541064518000419881, 2.621784821874995952 ) ) ;
#7555 = CARTESIAN_POINT ( 'NONE',  ( 4.243569643749999010, 15.62187500061451928, 27.54997392385601174 ) ) ;
#7556 = CARTESIAN_POINT ( 'NONE',  ( 7.978125000614517681, 6.421520780324663323E-16, -5.243569643749999010 ) ) ;
#7557 = CARTESIAN_POINT ( 'NONE',  ( 1.626862140677534273E-15, 10.32500000122903572, -26.00000000000000355 ) ) ;
#7558 = CARTESIAN_POINT ( 'NONE',  ( 5.409375000614516260, 4.541064518000418104, -2.621784821874998173 ) ) ;
#7559 = CARTESIAN_POINT ( 'NONE',  ( 5.810221930991193690E-16, 17.56250000000000000, 26.00000000000000000 ) ) ;
#7560 = CARTESIAN_POINT ( 'NONE',  ( 4.565625000614516260, 3.027376345333611329, 5.243569643749999010 ) ) ;
#7561 = CARTESIAN_POINT ( 'NONE',  ( 9.384375000614518569, 6.421520780324663323E-16, -5.243569643749999010 ) ) ;
#7562 = CARTESIAN_POINT ( 'NONE',  ( 15.86250000122903181, -4.330127018922190985, -2.500000000000001332 ) ) ;
#7563 = CARTESIAN_POINT ( 'NONE',  ( 4.884375000614518569, 6.421520780324663323E-16, -5.243569643749999010 ) ) ;
#7564 = CARTESIAN_POINT ( 'NONE',  ( 8.578125000614518214, 4.541064518000418104, 2.621784821874999949 ) ) ;
#7565 = CARTESIAN_POINT ( 'NONE',  ( 2.000000000000000444, 13.86874999877096748, 26.53589838486224650 ) ) ;
#7566 = CARTESIAN_POINT ( 'NONE',  ( 23.49375000122903145, -2.886751345948125991, -5.000000000000000000 ) ) ;
#7567 = CARTESIAN_POINT ( 'NONE',  ( 17.59687500061451715, 6.054752690667223547, 3.707466751127219781E-16 ) ) ;
#7568 = CYLINDRICAL_SURFACE ( 'NONE', #29018, 3.999999999999996447 ) ;
#7569 = ORIENTED_EDGE ( 'NONE', *, *, #68436, .F. ) ;
#7570 = CARTESIAN_POINT ( 'NONE',  ( 23.99062500061451786, -3.027376345333614438, 5.243569643749998122 ) ) ;
#7571 = CARTESIAN_POINT ( 'NONE',  ( 10.75312500061451715, 4.541064518000418104, -2.621784821874998173 ) ) ;
#7572 = EDGE_CURVE ( 'NONE', #48607, #43803, #6761, .T. ) ;
#7573 = CARTESIAN_POINT ( 'NONE',  ( 26.18437500061451573, 4.541064518000418104, 2.621784821874999949 ) ) ;
#7574 = CARTESIAN_POINT ( 'NONE',  ( 8.878125000614515372, 6.421520780324663323E-16, -5.243569643749999010 ) ) ;
#7575 = CARTESIAN_POINT ( 'NONE',  ( 20.47500000000000142, 4.330127018922191873, 2.499999999999999556 ) ) ;
#7576 = CARTESIAN_POINT ( 'NONE',  ( 11.06250000122903288, 4.330127018922192761, -2.499999999999997780 ) ) ;
#7577 = CARTESIAN_POINT ( 'NONE',  ( 24.81562500061451715, 3.027376345333611329, 5.243569643749999010 ) ) ;
#7578 = CARTESIAN_POINT ( 'NONE',  ( 2.121784821875001281, 12.30312500061451608, -26.32496088578401938 ) ) ;
#7579 = CARTESIAN_POINT ( 'NONE',  ( 13.91250000122903252, 0.000000000000000000, 4.999999999999998224 ) ) ;
#7580 = CARTESIAN_POINT ( 'NONE',  ( 21.02812500061451573, 6.421520780324663323E-16, -5.243569643749999010 ) ) ;
#7581 = CARTESIAN_POINT ( 'NONE',  ( 11.81250000000000000, 2.886751345948129099, -4.999999999999998224 ) ) ;
#7582 = CARTESIAN_POINT ( 'NONE',  ( 19.45312500061451644, 0.000000000000000000, 5.243569643749999010 ) ) ;
#7583 = CARTESIAN_POINT ( 'NONE',  ( 5.746875000614517504, -3.027376345333610441, -5.243569643749999898 ) ) ;
#7584 = CARTESIAN_POINT ( 'NONE',  ( 20.85000000000000142, 4.330127018922192761, -2.499999999999997780 ) ) ;
#7585 = CARTESIAN_POINT ( 'NONE',  ( 13.46250000122903323, 0.000000000000000000, 4.999999999999998224 ) ) ;
#7586 = CARTESIAN_POINT ( 'NONE',  ( 11.27812500061451573, 4.541064518000418104, 2.621784821874999949 ) ) ;
#7587 = CARTESIAN_POINT ( 'NONE',  ( 13.86562500061451431, 3.027376345333613106, -5.243569643749998122 ) ) ;
#7588 = CARTESIAN_POINT ( 'NONE',  ( 26.32500000122903216, 2.886751345948129099, -4.999999999999998224 ) ) ;
#7589 = AXIS2_PLACEMENT_3D ( 'NONE', #71577, #49410, #37220 ) ;
#7590 = CARTESIAN_POINT ( 'NONE',  ( 21.08437500061451786, 6.421520780324663323E-16, -5.243569643749999010 ) ) ;
#7591 = CARTESIAN_POINT ( 'NONE',  ( 45.00000000000000000, 0.000000000000000000, 0.000000000000000000 ) ) ;
#7592 = CARTESIAN_POINT ( 'NONE',  ( 6.900000001229035007, -2.886751345948125991, -5.000000000000000000 ) ) ;
#7593 = CARTESIAN_POINT ( 'NONE',  ( 7.809375000614519280, 0.000000000000000000, 5.243569643749999010 ) ) ;
#7594 = CARTESIAN_POINT ( 'NONE',  ( 25.88437500061451502, -4.541064518000419881, 2.621784821874995952 ) ) ;
#7595 = CARTESIAN_POINT ( 'NONE',  ( 3.009375000614516793, -4.541064518000417216, -2.621784821875001281 ) ) ;
#7596 = CARTESIAN_POINT ( 'NONE',  ( 22.45312500061451644, 4.541064518000418104, -2.621784821874998173 ) ) ;
#7597 = CARTESIAN_POINT ( 'NONE',  ( 27.19687500061451857, -3.027376345333614438, 5.243569643749998122 ) ) ;
#7598 = CARTESIAN_POINT ( 'NONE',  ( 1.878215178125000495, 16.87812499938548072, 26.74683588394047007 ) ) ;
#7599 = DIRECTION ( 'NONE',  ( -1.000000000000000000, -0.000000000000000000, -0.000000000000000000 ) ) ;
#7600 = CARTESIAN_POINT ( 'NONE',  ( 8.634375000614518569, 4.541064518000418104, 2.621784821874999949 ) ) ;
#7601 = CARTESIAN_POINT ( 'NONE',  ( 17.09062500061451573, 6.054752690667223547, 3.707466751127219781E-16 ) ) ;
#7602 = AXIS2_PLACEMENT_3D ( 'NONE', #26977, #38416, #9613 ) ;
#7603 = ORIENTED_EDGE ( 'NONE', *, *, #11775, .F. ) ;
#7604 = CARTESIAN_POINT ( 'NONE',  ( 30.00000000000000000, 0.000000000000000000, 0.000000000000000000 ) ) ;
#7605 = CARTESIAN_POINT ( 'NONE',  ( 28.04062500061451502, -3.027376345333614438, 5.243569643749998122 ) ) ;
#7606 = CARTESIAN_POINT ( 'NONE',  ( 4.996875000614516615, 6.054752690667223547, 3.707466751127219781E-16 ) ) ;
#7607 = CARTESIAN_POINT ( 'NONE',  ( 10.20000000122903572, 5.773502691896255534, 3.535250795749688401E-16 ) ) ;
#7608 = LINE ( 'NONE', #60671, #34756 ) ;
#7609 = CARTESIAN_POINT ( 'NONE',  ( 16.94999999999999929, 0.000000000000000000, 4.999999999999998224 ) ) ;
#7610 = CARTESIAN_POINT ( 'NONE',  ( 20.69062500061451715, 6.054752690667223547, 3.707466751127219781E-16 ) ) ;
#7611 = ORIENTED_EDGE ( 'NONE', *, *, #61652, .T. ) ;
#7612 = CARTESIAN_POINT ( 'NONE',  ( 25.16249999999999432, -5.773502691896255534, -1.060575238724906372E-15 ) ) ;
#7613 = ADVANCED_FACE ( 'NONE', ( #29295 ), #35191, .T. ) ;
#7614 = CARTESIAN_POINT ( 'NONE',  ( 26.63437500061451857, 4.541064518000418104, 2.621784821874999949 ) ) ;
#7615 = EDGE_LOOP ( 'NONE', ( #13757, #34736 ) ) ;
#7616 = CARTESIAN_POINT ( 'NONE',  ( 14.24062500061451608, -3.027376345333610441, -5.243569643749999898 ) ) ;
#7617 = CARTESIAN_POINT ( 'NONE',  ( 6.290625000614517681, 6.054752690667223547, 3.707466751127219781E-16 ) ) ;
#7618 = CARTESIAN_POINT ( 'NONE',  ( 15.53437500061451360, -2.746126346562642428, -4.756430356249999214 ) ) ;
#7619 = CARTESIAN_POINT ( 'NONE',  ( 29.65312500061451573, 4.541064518000418104, -2.621784821874998173 ) ) ;
#7620 = CARTESIAN_POINT ( 'NONE',  ( 15.97500000122903430, 2.886751345948129099, -4.999999999999998224 ) ) ;
#7621 = CARTESIAN_POINT ( 'NONE',  ( 19.94999999999999929, 4.330127018922192761, -2.499999999999997780 ) ) ;
#7622 = CARTESIAN_POINT ( 'NONE',  ( 28.04999999999999716, 4.330127018922192761, -2.499999999999997780 ) ) ;
#7623 = CARTESIAN_POINT ( 'NONE',  ( 3.759375000614517681, 0.000000000000000000, 5.243569643749999010 ) ) ;
#7624 = CARTESIAN_POINT ( 'NONE',  ( 9.309375000614517504, -4.541064518000417216, -2.621784821875001281 ) ) ;
#7625 = CARTESIAN_POINT ( 'NONE',  ( 18.60937500061451644, 0.000000000000000000, 5.243569643749999010 ) ) ;
#7626 = CARTESIAN_POINT ( 'NONE',  ( 18.86250000122903359, 0.000000000000000000, 4.999999999999998224 ) ) ;
#7627 = VERTEX_POINT ( 'NONE', #13013 ) ;
#7628 = CARTESIAN_POINT ( 'NONE',  ( 28.26562500061451289, 3.027376345333613106, -5.243569643749998122 ) ) ;
#7629 = CARTESIAN_POINT ( 'NONE',  ( 29.44687500061451857, -3.027376345333614438, 5.243569643749998122 ) ) ;
#7630 =( BOUNDED_CURVE ( )  B_SPLINE_CURVE ( 2, ( #72622, #5749, #60420, #28283, #26831, #22006, #27924 ),
 .UNSPECIFIED., .F., .F. ) 
 B_SPLINE_CURVE_WITH_KNOTS ( ( 3, 2, 2, 3 ),
 ( 0.3833333333333333037, 0.3861111111111111271, 0.3888888888888889506, 0.3916666666666667740 ),
 .UNSPECIFIED. ) 
 CURVE ( )  GEOMETRIC_REPRESENTATION_ITEM ( )  RATIONAL_B_SPLINE_CURVE ( ( 1.000000000000002665, 0.8660254037844360431, 1.000000000000000000, 0.8660254037844387076, 1.000000000000000000, 0.8660254037844333785, 1.000000000000005329 ) ) 
 REPRESENTATION_ITEM ( '' )  );
#7631 = CARTESIAN_POINT ( 'NONE',  ( 4.059375000614519280, 4.541064518000418104, -2.621784821874998173 ) ) ;
#7632 = CARTESIAN_POINT ( 'NONE',  ( 16.08749999999999503, -2.886751345948129988, 4.999999999999997335 ) ) ;
#7633 = CARTESIAN_POINT ( 'NONE',  ( 12.89062500061451821, -3.027376345333610441, -5.243569643749999898 ) ) ;
#7634 = CARTESIAN_POINT ( 'NONE',  ( 2.000000000000000444, 20.22500000000000142, 26.53589838486224650 ) ) ;
#7635 = CARTESIAN_POINT ( 'NONE',  ( 8.381250001229034297, 4.330127018922191873, 2.499999999999999556 ) ) ;
#7636 = CARTESIAN_POINT ( 'NONE',  ( 18.45000000122903216, -2.886751345948129988, 4.999999999999997335 ) ) ;
#7637 = DIRECTION ( 'NONE',  ( 0.000000000000000000, 0.000000000000000000, 1.000000000000000000 ) ) ;
#7638 = CARTESIAN_POINT ( 'NONE',  ( 17.97187500061451715, 2.746126346562645981, -4.756430356249997438 ) ) ;
#7639 = CARTESIAN_POINT ( 'NONE',  ( 6.478125000614516793, -4.541064518000419881, 2.621784821874995952 ) ) ;
#7640 = CARTESIAN_POINT ( 'NONE',  ( 25.32187500061451857, 3.027376345333611329, 5.243569643749999010 ) ) ;
#7641 = CARTESIAN_POINT ( 'NONE',  ( 2.121784821875001281, 18.65937500061451715, 33.67503911421598417 ) ) ;
#7642 = CARTESIAN_POINT ( 'NONE',  ( 25.54687500061451644, -3.027376345333610441, -5.243569643749999898 ) ) ;
#7643 = CARTESIAN_POINT ( 'NONE',  ( 8.137500000000002842, -2.886751345948125991, -5.000000000000000000 ) ) ;
#7644 = CARTESIAN_POINT ( 'NONE',  ( -1.999999999999997113, 14.33750000122903323, 33.46410161513775705 ) ) ;
#7645 = CARTESIAN_POINT ( 'NONE',  ( 14.87812500061451537, 4.541064518000418104, 2.621784821874999949 ) ) ;
#7646 = CARTESIAN_POINT ( 'NONE',  ( 5.775000001229033231, 2.886751345948126879, 4.999999999999999112 ) ) ;
#7647 = CARTESIAN_POINT ( 'NONE',  ( 12.15937500061451892, 4.541064518000418104, -2.621784821874998173 ) ) ;
#7648 = CYLINDRICAL_SURFACE ( 'NONE', #66672, 4.999999999999998224 ) ;
#7649 = VERTEX_POINT ( 'NONE', #504 ) ;
#7650 = AXIS2_PLACEMENT_3D ( 'NONE', #65481, #59561, #60656 ) ;
#7651 = CARTESIAN_POINT ( 'NONE',  ( 12.77812500061451750, -4.541064518000419881, 2.621784821874995952 ) ) ;
#7652 = DIRECTION ( 'NONE',  ( -0.000000000000000000, -1.000000000000000000, -0.000000000000000000 ) ) ;
#7653 = CARTESIAN_POINT ( 'NONE',  ( 24.37500000122903288, -5.773502691896255534, -1.060575238724906372E-15 ) ) ;
#7654 = CARTESIAN_POINT ( 'NONE',  ( 12.68437500061451573, 4.541064518000418104, 2.621784821874999949 ) ) ;
#7655 = CARTESIAN_POINT ( 'NONE',  ( 15.25312500061451715, 4.541064518000418104, -2.621784821874998173 ) ) ;
#7656 = CARTESIAN_POINT ( 'NONE',  ( 26.28750000122903430, 6.123233995736764310E-16, -4.999999999999998224 ) ) ;
#7657 = CARTESIAN_POINT ( 'NONE',  ( 24.87187500061451573, 3.027376345333611329, 5.243569643749999010 ) ) ;
#7658 = AXIS2_PLACEMENT_3D ( 'NONE', #10070, #15960, #55499 ) ;
#7659 = CARTESIAN_POINT ( 'NONE',  ( -1.394453263437886604E-15, 19.66249999999999787, 33.99999999999999289 ) ) ;
#7660 = CARTESIAN_POINT ( 'NONE',  ( -2.121784821874999949, 17.98437500061451999, -33.67503911421598417 ) ) ;
#7661 = CARTESIAN_POINT ( 'NONE',  ( 16.62187500061451573, 3.027376345333613106, -5.243569643749998122 ) ) ;
#7662 = CARTESIAN_POINT ( 'NONE',  ( 17.88750000122903216, 4.330127018922191873, 2.499999999999999556 ) ) ;
#7663 =( BOUNDED_CURVE ( )  B_SPLINE_CURVE ( 2, ( #56473, #4781, #62375, #15845, #33209, #33568, #44314 ),
 .UNSPECIFIED., .F., .F. ) 
 B_SPLINE_CURVE_WITH_KNOTS ( ( 3, 2, 2, 3 ),
 ( 0.4583333333333332593, 0.4611111111111111382, 0.4638888888888889062, 0.4666666666666667296 ),
 .UNSPECIFIED. ) 
 CURVE ( )  GEOMETRIC_REPRESENTATION_ITEM ( )  RATIONAL_B_SPLINE_CURVE ( ( 1.000000000000002665, 0.8660254037844360431, 1.000000000000000000, 0.8660254037844387076, 1.000000000000000000, 0.8660254037844360431, 1.000000000000002665 ) ) 
 REPRESENTATION_ITEM ( '' )  );
#7664 = CARTESIAN_POINT ( 'NONE',  ( 12.75937500061451857, 0.000000000000000000, 5.243569643749999010 ) ) ;
#7665 = CARTESIAN_POINT ( 'NONE',  ( 4.243569643749999898, 19.09062500061451573, -27.54997392385601529 ) ) ;
#7666 = CARTESIAN_POINT ( 'NONE',  ( 19.46250000122903145, -4.330127018922190985, -2.500000000000001332 ) ) ;
#7667 = CARTESIAN_POINT ( 'NONE',  ( 12.51562500061451821, 3.027376345333613106, -5.243569643749998122 ) ) ;
#7668 = ORIENTED_EDGE ( 'NONE', *, *, #35039, .T. ) ;
#7669 = ORIENTED_EDGE ( 'NONE', *, *, #37449, .F. ) ;
#7670 = AXIS2_PLACEMENT_3D ( 'NONE', #1717, #24229, #53774 ) ;
#7671 = CARTESIAN_POINT ( 'NONE',  ( 17.66249999999999787, 2.886751345948129099, -4.999999999999998224 ) ) ;
#7672 = CARTESIAN_POINT ( 'NONE',  ( 27.41250000000000142, -5.773502691896255534, -1.060575238724906372E-15 ) ) ;
#7673 = CARTESIAN_POINT ( 'NONE',  ( 13.58437500061451786, 4.541064518000418104, 2.621784821874999949 ) ) ;
#7674 = CARTESIAN_POINT ( 'NONE',  ( 30.00000000000000000, 0.000000000000000000, 0.000000000000000000 ) ) ;
#7675 = ADVANCED_FACE ( 'NONE', ( #34464 ), #48223, .T. ) ;
#7676 = CARTESIAN_POINT ( 'NONE',  ( 13.46250000122903323, 0.000000000000000000, 4.999999999999998224 ) ) ;
#7677 = CARTESIAN_POINT ( 'NONE',  ( 21.48750000122903003, 4.330127018922191873, 2.499999999999999556 ) ) ;
#7678 = CARTESIAN_POINT ( 'NONE',  ( 18.10312500061451502, 0.000000000000000000, 5.243569643749999010 ) ) ;
#7679 = CARTESIAN_POINT ( 'NONE',  ( 23.01562500061451644, 3.027376345333611329, 5.243569643749999010 ) ) ;
#7680 = CARTESIAN_POINT ( 'NONE',  ( 29.66250000122903074, 0.000000000000000000, 4.999999999999998224 ) ) ;
#7681 = CARTESIAN_POINT ( 'NONE',  ( 28.68749999999999645, -2.886751345948129988, 4.999999999999997335 ) ) ;
#7682 = CYLINDRICAL_SURFACE ( 'NONE', #45433, 4.999999999999998224 ) ;
#7683 =( BOUNDED_CURVE ( )  B_SPLINE_CURVE ( 2, ( #66036, #15414, #42415, #19862, #9524, #70848, #64935 ),
 .UNSPECIFIED., .F., .F. ) 
 B_SPLINE_CURVE_WITH_KNOTS ( ( 3, 2, 2, 3 ),
 ( 0.9000000000000001332, 0.9027777777777779011, 0.9055555555555556690, 0.9083333333333334370 ),
 .UNSPECIFIED. ) 
 CURVE ( )  GEOMETRIC_REPRESENTATION_ITEM ( )  RATIONAL_B_SPLINE_CURVE ( ( 0.9999999999999946709, 0.8660254037844440367, 1.000000000000000000, 0.8660254037844387076, 1.000000000000000000, 0.8660254037844333785, 1.000000000000005329 ) ) 
 REPRESENTATION_ITEM ( '' )  );
#7684 = CARTESIAN_POINT ( 'NONE',  ( 29.88749999999999929, 5.773502691896255534, 3.535250795749688894E-16 ) ) ;
#7685 = CARTESIAN_POINT ( 'NONE',  ( 2.000000000000001332, 9.912500001229034297, -26.53589838486224650 ) ) ;
#7686 = CARTESIAN_POINT ( 'NONE',  ( -4.243569643749999898, 16.22187500061452070, -32.45002607614398471 ) ) ;
#7687 = CARTESIAN_POINT ( 'NONE',  ( 3.975000001229033852, 2.886751345948126879, 4.999999999999999112 ) ) ;
#7688 = CARTESIAN_POINT ( 'NONE',  ( 7.012500000000001066, 2.886751345948126879, 4.999999999999999112 ) ) ;
#7689 = CYLINDRICAL_SURFACE ( 'NONE', #53791, 4.999999999999998224 ) ;
#7690 = CARTESIAN_POINT ( 'NONE',  ( 10.32187500061451679, 3.027376345333613106, -5.243569643749998122 ) ) ;
#7691 = CARTESIAN_POINT ( 'NONE',  ( 27.29062500061451502, -3.027376345333610441, -5.243569643749999898 ) ) ;
#7692 = DIRECTION ( 'NONE',  ( 0.000000000000000000, 0.000000000000000000, 1.000000000000000000 ) ) ;
#7693 = CARTESIAN_POINT ( 'NONE',  ( -3.980704297455869511, 9.178376072143947795, -34.50551769337345576 ) ) ;
#7694 = AXIS2_PLACEMENT_3D ( 'NONE', #19530, #8460, #48727 ) ;
#7695 = CARTESIAN_POINT ( 'NONE',  ( 0.000000000000000000, 27.50000000000000000, 30.00000000000000000 ) ) ;
#7696 = CARTESIAN_POINT ( 'NONE',  ( 8.559375000614515727, 4.541064518000418104, -2.621784821874998173 ) ) ;
#7697 = CARTESIAN_POINT ( 'NONE',  ( 11.78437500061451892, 4.541064518000418104, 2.621784821874999949 ) ) ;
#7698 = CARTESIAN_POINT ( 'NONE',  ( 7.425000000000000711, 4.330127018922191873, 2.499999999999999556 ) ) ;
#7699 = CARTESIAN_POINT ( 'NONE',  ( -3.000416591977282496E-16, 14.74062500061459424, 25.09994784771203058 ) ) ;
#7700 = EDGE_CURVE ( 'NONE', #30519, #66542, #33133, .T. ) ;
#7701 = CARTESIAN_POINT ( 'NONE',  ( 1.777890502354250168, 25.43624258734061883, 26.40726507414123958 ) ) ;
#7702 = CARTESIAN_POINT ( 'NONE',  ( 7.612500000000000711, -5.773502691896255534, -1.060575238724906372E-15 ) ) ;
#7703 = VECTOR ( 'NONE', #36777, 1000.000000000000000 ) ;
#7704 = CARTESIAN_POINT ( 'NONE',  ( 15.15937500061451537, 2.746126346562645981, -4.756430356249997438 ) ) ;
#7705 = B_SPLINE_CURVE_WITH_KNOTS ( 'NONE', 3,
 ( #54802, #15997, #59965, #54442, #65886, #16359, #26736, #61433, #15626, #4208 ),
 .UNSPECIFIED., .F., .F.,
 ( 4, 3, 3, 4 ),
 ( 1.799357552115988686E-16, 0.0001572276214405268226, 0.0003144552949517756741, 0.0005183884262692322036 ),
 .UNSPECIFIED. ) ;
#7706 = CARTESIAN_POINT ( 'NONE',  ( 21.40312500061451573, -4.541064518000417216, -2.621784821875001281 ) ) ;
#7707 = CARTESIAN_POINT ( 'NONE',  ( 12.51562500061451821, 3.027376345333613106, -5.243569643749998122 ) ) ;
#7708 = CARTESIAN_POINT ( 'NONE',  ( 24.49687500061451573, -4.119189519843965641, -2.378215178125001383 ) ) ;
#7709 = CARTESIAN_POINT ( 'NONE',  ( 10.32187500061451679, 3.027376345333613106, -5.243569643749998122 ) ) ;
#7710 = CARTESIAN_POINT ( 'NONE',  ( 25.87500000000000000, 4.330127018922191873, 2.499999999999999556 ) ) ;
#7711 = CARTESIAN_POINT ( 'NONE',  ( 22.91250000122903430, 0.000000000000000000, 4.999999999999998224 ) ) ;
#7712 = CARTESIAN_POINT ( 'NONE',  ( 17.17500000000000071, 6.123233995736764310E-16, -4.999999999999998224 ) ) ;
#7713 = CIRCLE ( 'NONE', #28956, 9.000000000000000000 ) ;
#7714 = CARTESIAN_POINT ( 'NONE',  ( 12.08437500061451608, 6.421520780324663323E-16, -5.243569643749999010 ) ) ;
#7715 = CARTESIAN_POINT ( 'NONE',  ( 25.58437500061451431, 6.421520780324663323E-16, -5.243569643749999010 ) ) ;
#7716 = CARTESIAN_POINT ( 'NONE',  ( 28.18125000122903145, 4.330127018922191873, 2.499999999999999556 ) ) ;
#7717 = CARTESIAN_POINT ( 'NONE',  ( 24.45000000122903572, -2.886751345948109559, -5.000000000000028422 ) ) ;
#7718 = CARTESIAN_POINT ( 'NONE',  ( 20.89687500061452141, -3.027376345333614438, 5.243569643749998122 ) ) ;
#7719 = CARTESIAN_POINT ( 'NONE',  ( 11.44687500061451857, -3.027376345333614438, 5.243569643749998122 ) ) ;
#7720 = CARTESIAN_POINT ( 'NONE',  ( 3.756430356250000102, 19.50312499938548072, 30.00000000000000000 ) ) ;
#7721 = CARTESIAN_POINT ( 'NONE',  ( 23.28750000000000142, -2.886751345948129988, 4.999999999999997335 ) ) ;
#7722 = CARTESIAN_POINT ( 'NONE',  ( -7.967954043666661671E-16, 20.17812499938548143, 34.33755215474603517 ) ) ;
#7723 = CARTESIAN_POINT ( 'NONE',  ( -2.121784821874999949, 12.58437500061451786, -33.67503911421598417 ) ) ;
#7724 = CARTESIAN_POINT ( 'NONE',  ( 27.79687500061451999, -2.746126346562642428, -4.756430356249999214 ) ) ;
#7725 = CARTESIAN_POINT ( 'NONE',  ( 14.27812500061451573, 6.421520780324663323E-16, -5.243569643749999010 ) ) ;
#7726 = CARTESIAN_POINT ( 'NONE',  ( 5.662500000000000533, 2.886751345948126879, 4.999999999999999112 ) ) ;
#7727 = CARTESIAN_POINT ( 'NONE',  ( -1.999999999999999112, 18.05000000000000071, 26.53589838486224650 ) ) ;
#7728 = CARTESIAN_POINT ( 'NONE',  ( -3.999999999999999112, 13.21250000000000213, -32.30940107675850470 ) ) ;
#7729 = CARTESIAN_POINT ( 'NONE',  ( 13.95000000000000107, -4.330127018922190985, -2.500000000000001332 ) ) ;
#7730 = CARTESIAN_POINT ( 'NONE',  ( -2.121784821874999949, 10.72812500061451679, 26.32496088578401938 ) ) ;
#7731 = CARTESIAN_POINT ( 'NONE',  ( 14.17500000122903536, 2.886751345948129099, -4.999999999999998224 ) ) ;
#7732 = CARTESIAN_POINT ( 'NONE',  ( 25.92187500061451999, -6.054752690667223547, -1.112240025338166033E-15 ) ) ;
#7733 = EDGE_LOOP ( 'NONE', ( #39629, #49268, #24959, #39725 ) ) ;
#7734 = CARTESIAN_POINT ( 'NONE',  ( 19.00312500061451715, 0.000000000000000000, 5.243569643749999010 ) ) ;
#7735 = CARTESIAN_POINT ( 'NONE',  ( 4.490625000614516971, 6.054752690667223547, 3.707466751127219781E-16 ) ) ;
#7736 = CARTESIAN_POINT ( 'NONE',  ( 19.09687500061451360, -3.027376345333614438, 5.243569643749998122 ) ) ;
#7737 = CARTESIAN_POINT ( 'NONE',  ( 3.562500000000000444, -5.773502691896255534, -1.060575238724906372E-15 ) ) ;
#7738 = CARTESIAN_POINT ( 'NONE',  ( 8.278125000614515727, -4.541064518000419881, 2.621784821874995952 ) ) ;
#7739 = CARTESIAN_POINT ( 'NONE',  ( 20.72812500061451502, 4.541064518000418104, 2.621784821874999949 ) ) ;
#7740 = CARTESIAN_POINT ( 'NONE',  ( 4.243569643749999898, 14.17812500061451608, 30.00000000000000000 ) ) ;
#7741 = CARTESIAN_POINT ( 'NONE',  ( 19.80000000122903359, -2.886751345948129988, 4.999999999999997335 ) ) ;
#7742 = CARTESIAN_POINT ( 'NONE',  ( 12.94687500061451857, -2.746126346562641984, -4.756430356249999214 ) ) ;
#7743 = CARTESIAN_POINT ( 'NONE',  ( 9.215625000614515727, -6.054752690667223547, -1.112240025338166033E-15 ) ) ;
#7744 = CARTESIAN_POINT ( 'NONE',  ( 4.284375000614518925, -4.541064518000419881, 2.621784821874995952 ) ) ;
#7745 = CARTESIAN_POINT ( 'NONE',  ( 3.421875000614516882, -6.054752690667223547, -1.112240025338166033E-15 ) ) ;
#7746 = CARTESIAN_POINT ( 'NONE',  ( 23.74687500061451573, -3.027376345333610441, -5.243569643749999898 ) ) ;
#7747 = CARTESIAN_POINT ( 'NONE',  ( 14.16562500061451679, -6.054752690667223547, -1.112240025338166033E-15 ) ) ;
#7748 = CARTESIAN_POINT ( 'NONE',  ( 24.03750000122903430, 6.123233995736764310E-16, -4.999999999999998224 ) ) ;
#7749 = CARTESIAN_POINT ( 'NONE',  ( 26.01562500061451289, 3.027376345333613106, -5.243569643749998122 ) ) ;
#7750 = CARTESIAN_POINT ( 'NONE',  ( 19.09687500061451360, -3.027376345333614438, 5.243569643749998122 ) ) ;
#7751 = CARTESIAN_POINT ( 'NONE',  ( 14.65312500061451573, -4.541064518000417216, -2.621784821875001281 ) ) ;
#7752 = CARTESIAN_POINT ( 'NONE',  ( 2.121784821875001281, 17.30937500061451573, 33.67503911421598417 ) ) ;
#7753 = VECTOR ( 'NONE', #20551, 1000.000000000000000 ) ;
#7754 = CARTESIAN_POINT ( 'NONE',  ( 20.12812500061451715, 6.421520780324663323E-16, -5.243569643749999010 ) ) ;
#7755 = CARTESIAN_POINT ( 'NONE',  ( 3.337500001229034563, 6.123233995736764310E-16, -4.999999999999998224 ) ) ;
#7756 = ORIENTED_EDGE ( 'NONE', *, *, #41935, .T. ) ;
#7757 = CARTESIAN_POINT ( 'NONE',  ( 24.48749999999999716, 5.773502691896255534, 3.535250795749688894E-16 ) ) ;
#7758 = CARTESIAN_POINT ( 'NONE',  ( -3.999999999999997335, 11.48750000000000071, -27.69059892324149175 ) ) ;
#7759 = CARTESIAN_POINT ( 'NONE',  ( 2.655984681222220721E-16, 20.06562499938548427, 25.66244784525396483 ) ) ;
#7760 = CARTESIAN_POINT ( 'NONE',  ( 26.09062500061451573, 6.054752690667223547, 3.707466751127219781E-16 ) ) ;
#7761 = CARTESIAN_POINT ( 'NONE',  ( 6.665625000614515905, 3.027376345333613106, -5.243569643749998122 ) ) ;
#7762 = CARTESIAN_POINT ( 'NONE',  ( 18.90000000122902790, -2.886751345948129988, 4.999999999999997335 ) ) ;
#7763 = CARTESIAN_POINT ( 'NONE',  ( 24.74062500061451786, 6.054752690667223547, 3.707466751127219781E-16 ) ) ;
#7764 = CARTESIAN_POINT ( 'NONE',  ( 24.18750000000000355, -2.886751345948129988, 4.999999999999997335 ) ) ;
#7765 = CARTESIAN_POINT ( 'NONE',  ( -2.000000000000000000, 16.43750000122903643, -33.46410161513775705 ) ) ;
#7766 = EDGE_CURVE ( 'NONE', #62319, #29541, #14716, .T. ) ;
#7767 = CARTESIAN_POINT ( 'NONE',  ( 25.38750000122903216, 6.123233995736764310E-16, -4.999999999999998224 ) ) ;
#7768 = CARTESIAN_POINT ( 'NONE',  ( 10.79062500061451679, 6.054752690667223547, 3.707466751127219781E-16 ) ) ;
#7769 = ORIENTED_EDGE ( 'NONE', *, *, #36745, .F. ) ;
#7770 = VECTOR ( 'NONE', #37424, 1000.000000000000000 ) ;
#7771 = CARTESIAN_POINT ( 'NONE',  ( 25.30312500061451431, 0.000000000000000000, 5.243569643749999010 ) ) ;
#7772 = CARTESIAN_POINT ( 'NONE',  ( 8.503125000614515372, 4.541064518000418104, -2.621784821874998173 ) ) ;
#7773 = UNCERTAINTY_MEASURE_WITH_UNIT (LENGTH_MEASURE( 1.000000000000000082E-05 ), #51324, 'distance_accuracy_value', 'NONE');
#7774 = AXIS2_PLACEMENT_3D ( 'NONE', #45881, #34419, #57672 ) ;
#7775 = CARTESIAN_POINT ( 'NONE',  ( 4.640625000614518214, -3.027376345333614438, 5.243569643749998122 ) ) ;
#7776 = CARTESIAN_POINT ( 'NONE',  ( 13.50937500061451679, 4.119189519843966529, -2.378215178124998275 ) ) ;
#7777 = CARTESIAN_POINT ( 'NONE',  ( 14.13750000000000107, 5.773502691896255534, 3.535250795749688894E-16 ) ) ;
#7778 = CARTESIAN_POINT ( 'NONE',  ( 14.78437500061451715, 6.421520780324663323E-16, -5.243569643749999010 ) ) ;
#7779 = CARTESIAN_POINT ( 'NONE',  ( 8.512500001229033941, 0.000000000000000000, 4.999999999999998224 ) ) ;
#7780 = CARTESIAN_POINT ( 'NONE',  ( 18.19687500061451502, -3.027376345333614438, 5.243569643749998122 ) ) ;
#7781 = CARTESIAN_POINT ( 'NONE',  ( 17.39999999999999858, 0.000000000000000000, 4.999999999999998224 ) ) ;
#7782 = CARTESIAN_POINT ( 'NONE',  ( 8.521875000614516082, 3.027376345333613106, -5.243569643749998122 ) ) ;
#7783 = CARTESIAN_POINT ( 'NONE',  ( 4.243569643749999898, 11.44062500061451715, -27.54997392385601529 ) ) ;
#7784 = CARTESIAN_POINT ( 'NONE',  ( 30.00000000000000000, 0.000000000000000000, 0.000000000000000000 ) ) ;
#7785 = CARTESIAN_POINT ( 'NONE',  ( 22.95937500061451786, 2.746126346562643317, 4.756430356249998326 ) ) ;
#7786 = DIRECTION ( 'NONE',  ( 0.000000000000000000, 0.000000000000000000, 1.000000000000000000 ) ) ;
#7787 = CARTESIAN_POINT ( 'NONE',  ( 23.42812500061451786, 4.541064518000418104, 2.621784821874999949 ) ) ;
#7788 = CARTESIAN_POINT ( 'NONE',  ( 26.63437500061451857, 4.541064518000418104, 2.621784821874999949 ) ) ;
#7789 = CARTESIAN_POINT ( 'NONE',  ( 29.59687500061451715, -3.027376345333610441, -5.243569643749999898 ) ) ;
#7790 = CARTESIAN_POINT ( 'NONE',  ( 21.78750000000000142, 5.773502691896255534, 3.535250795749688894E-16 ) ) ;
#7791 = EDGE_CURVE ( 'NONE', #69714, #31816, #12842, .T. ) ;
#7792 = CARTESIAN_POINT ( 'NONE',  ( 6.253125000614517148, 4.541064518000418104, -2.621784821874998173 ) ) ;
#7793 = CARTESIAN_POINT ( 'NONE',  ( 21.60937500061451644, 2.746126346562643317, 4.756430356249998326 ) ) ;
#7794 = CARTESIAN_POINT ( 'NONE',  ( 15.64687500061451608, -3.027376345333610441, -5.243569643749999898 ) ) ;
#7795 = CARTESIAN_POINT ( 'NONE',  ( 8.221875000614515372, -4.119189519843968306, 2.378215178124996054 ) ) ;
#7796 = AXIS2_PLACEMENT_3D ( 'NONE', #48682, #60844, #54223 ) ;
#7797 = CARTESIAN_POINT ( 'NONE',  ( 4.040625000614517681, 6.054752690667223547, 3.707466751127219781E-16 ) ) ;
#7798 = CARTESIAN_POINT ( 'NONE',  ( 7.584375000614516082, 6.421520780324663323E-16, -5.243569643749999010 ) ) ;
#7799 = ORIENTED_EDGE ( 'NONE', *, *, #16945, .F. ) ;
#7800 = CARTESIAN_POINT ( 'NONE',  ( 18.30937500061451928, -4.541064518000417216, -2.621784821875001281 ) ) ;
#7801 = CARTESIAN_POINT ( 'NONE',  ( -1.778782919078051528, 25.43611513164544036, 26.40779114962846919 ) ) ;
#7802 = CARTESIAN_POINT ( 'NONE',  ( 27.44999999999999929, -4.330127018922190985, -2.500000000000001332 ) ) ;
#7803 = CARTESIAN_POINT ( 'NONE',  ( 27.53437500061451360, 4.541064518000418104, 2.621784821874999949 ) ) ;
#7804 = CYLINDRICAL_SURFACE ( 'NONE', #28972, 4.999999999999998224 ) ;
#7805 = PLANE ( 'NONE',  #3224 ) ;
#7806 = ORIENTED_EDGE ( 'NONE', *, *, #32061, .F. ) ;
#7807 = CARTESIAN_POINT ( 'NONE',  ( 11.51250000000000107, 2.886751345948126879, 4.999999999999999112 ) ) ;
#7808 = CARTESIAN_POINT ( 'NONE',  ( 12.38437500061451502, -2.746126346562642428, -4.756430356249999214 ) ) ;
#7809 = CARTESIAN_POINT ( 'NONE',  ( 22.30312500061451431, -4.541064518000417216, -2.621784821875001281 ) ) ;
#7810 = CARTESIAN_POINT ( 'NONE',  ( 12.56250000000000178, -5.773502691896255534, -1.060575238724906372E-15 ) ) ;
#7811 =( BOUNDED_CURVE ( )  B_SPLINE_CURVE ( 2, ( #20303, #20672, #48407, #36577, #49498, #53569, #9241, #8871, #65750 ),
 .UNSPECIFIED., .F., .T. ) 
 B_SPLINE_CURVE_WITH_KNOTS ( ( 3, 2, 2, 2, 3 ),
 ( 0.5978260869565217295, 0.6014492753623188470, 0.6086956521739130821, 0.6159420289855072062, 0.6195652173913043237 ),
 .UNSPECIFIED. ) 
 CURVE ( )  GEOMETRIC_REPRESENTATION_ITEM ( )  RATIONAL_B_SPLINE_CURVE ( ( 0.9330127018922194093, 0.9330127018922194093, 1.000000000000000000, 0.8660254037844387076, 1.000000000000000000, 0.8660254037844387076, 1.000000000000000000, 0.9330127018922194093, 0.9330127018922194093 ) ) 
 REPRESENTATION_ITEM ( '' )  );
#7812 = CARTESIAN_POINT ( 'NONE',  ( 8.325000001229033941, 2.886751345948129099, -4.999999999999998224 ) ) ;
#7813 = CARTESIAN_POINT ( 'NONE',  ( 6.403125000614517504, 0.000000000000000000, 5.243569643749999010 ) ) ;
#7814 = CARTESIAN_POINT ( 'NONE',  ( 21.86250000000000071, 2.886751345948126879, 4.999999999999999112 ) ) ;
#7815 = CARTESIAN_POINT ( 'NONE',  ( 20.16562500061451146, 3.027376345333613106, -5.243569643749998122 ) ) ;
#7816 = CARTESIAN_POINT ( 'NONE',  ( 45.00000000000000000, 6.123233995736764310E-16, -4.999999999999998224 ) ) ;
#7817 = CARTESIAN_POINT ( 'NONE',  ( 25.80000000122903714, -2.886751345948125991, -5.000000000000000000 ) ) ;
#7818 = CARTESIAN_POINT ( 'NONE',  ( 1.878215178124997609, 19.76562499938548356, 33.25316411605952993 ) ) ;
#7819 = CARTESIAN_POINT ( 'NONE',  ( 4.275000000000001243, 4.330127018922191873, 2.499999999999999556 ) ) ;
#7820 = VERTEX_POINT ( 'NONE', #49814 ) ;
#7821 = CARTESIAN_POINT ( 'NONE',  ( 18.66562500061451146, -6.054752690667223547, -1.112240025338166033E-15 ) ) ;
#7822 = CARTESIAN_POINT ( 'NONE',  ( 25.82812500061451644, -4.541064518000419881, 2.621784821874995952 ) ) ;
#7823 = CARTESIAN_POINT ( 'NONE',  ( 26.52187500061451431, 3.027376345333613106, -5.243569643749998122 ) ) ;
#7824 = CARTESIAN_POINT ( 'NONE',  ( 14.57812500061451644, -4.541064518000419881, 2.621784821874995952 ) ) ;
#7825 = CARTESIAN_POINT ( 'NONE',  ( 29.76562500061451644, 3.027376345333611329, 5.243569643749999010 ) ) ;
#7826 = CARTESIAN_POINT ( 'NONE',  ( 8.465625000614515727, 3.027376345333613106, -5.243569643749998122 ) ) ;
#7827 = CARTESIAN_POINT ( 'NONE',  ( 4.898587196589412829E-16, 27.50000000000000000, 34.00000000000000000 ) ) ;
#7828 = CARTESIAN_POINT ( 'NONE',  ( 27.18750000122903288, 6.123233995736764310E-16, -4.999999999999998224 ) ) ;
#7829 = CARTESIAN_POINT ( 'NONE',  ( 18.42187500061451999, 2.746126346562645981, -4.756430356249997438 ) ) ;
#7830 = CARTESIAN_POINT ( 'NONE',  ( 17.05312500061451786, 4.541064518000418104, -2.621784821874998173 ) ) ;
#7831 = CARTESIAN_POINT ( 'NONE',  ( 29.29687500061451644, 6.054752690667223547, 3.707466751127219781E-16 ) ) ;
#7832 = CARTESIAN_POINT ( 'NONE',  ( 9.534375000614517148, 4.541064518000418104, 2.621784821874999949 ) ) ;
#7833 = CARTESIAN_POINT ( 'NONE',  ( 8.934375000614517504, 6.421520780324663323E-16, -5.243569643749999010 ) ) ;
#7834 = CARTESIAN_POINT ( 'NONE',  ( 18.23437500061451999, -4.541064518000419881, 2.621784821874995952 ) ) ;
#7835 = ORIENTED_EDGE ( 'NONE', *, *, #561, .T. ) ;
#7836 = CARTESIAN_POINT ( 'NONE',  ( 29.43750000000000000, 5.773502691896255534, 3.535250795749688401E-16 ) ) ;
#7837 = CARTESIAN_POINT ( 'NONE',  ( 20.54062500061451502, -3.027376345333610441, -5.243569643749999898 ) ) ;
#7838 = CARTESIAN_POINT ( 'NONE',  ( 16.92187500061451999, -6.054752690667223547, -1.112240025338166033E-15 ) ) ;
#7839 = CARTESIAN_POINT ( 'NONE',  ( 22.37812500061451360, 6.421520780324663323E-16, -5.243569643749999010 ) ) ;
#7840 = CARTESIAN_POINT ( 'NONE',  ( -2.828200636599751609E-16, 15.38750000000000284, 25.38119784648299770 ) ) ;
#7841 = CARTESIAN_POINT ( 'NONE',  ( 28.60312500061451502, -4.541064518000417216, -2.621784821875001281 ) ) ;
#7842 = CARTESIAN_POINT ( 'NONE',  ( 9.375000001229036428, 2.886751345948126879, 4.999999999999999112 ) ) ;
#7843 = ORIENTED_EDGE ( 'NONE', *, *, #17293, .T. ) ;
#7844 = CARTESIAN_POINT ( 'NONE',  ( 3.712500001229034563, -4.330127018922190985, -2.500000000000001332 ) ) ;
#7845 = CARTESIAN_POINT ( 'NONE',  ( -3.999999999999999556, 18.61250000000000426, -32.30940107675850470 ) ) ;
#7846 = CIRCLE ( 'NONE', #49146, 4.000000000000000000 ) ;
#7847 = CARTESIAN_POINT ( 'NONE',  ( 23.92500000122903359, -5.773502691896255534, -1.060575238724906372E-15 ) ) ;
#7848 = CARTESIAN_POINT ( 'NONE',  ( 2.828200636599751609E-16, 19.75624999877096499, 25.38119784648299415 ) ) ;
#7849 = CARTESIAN_POINT ( 'NONE',  ( 10.35937500061451644, 4.541064518000418104, -2.621784821874998173 ) ) ;
#7850 = CARTESIAN_POINT ( 'NONE',  ( 24.56250000000000355, 2.886751345948093572, 5.000000000000056843 ) ) ;
#7851 = CARTESIAN_POINT ( 'NONE',  ( 13.97812500061451679, 4.541064518000418104, 2.621784821874999949 ) ) ;
#7852 = CARTESIAN_POINT ( 'NONE',  ( 10.62187500061451928, -6.054752690667223547, -1.112240025338166033E-15 ) ) ;
#7853 = CARTESIAN_POINT ( 'NONE',  ( 3.028125000614518392, 6.421520780324663323E-16, -5.243569643749999010 ) ) ;
#7854 = CARTESIAN_POINT ( 'NONE',  ( 18.00937500061451502, 4.541064518000418104, -2.621784821874998173 ) ) ;
#7855 = CARTESIAN_POINT ( 'NONE',  ( 8.071875000614518569, 3.027376345333613106, -5.243569643749998122 ) ) ;
#7856 = CARTESIAN_POINT ( 'NONE',  ( 4.000000000000000000, 18.83749999999999858, 27.69059892324149885 ) ) ;
#7857 = CARTESIAN_POINT ( 'NONE',  ( 6.890625000614516438, -3.027376345333614438, 5.243569643749998122 ) ) ;
#7858 = CARTESIAN_POINT ( 'NONE',  ( 18.70312500061451644, -4.541064518000417216, -2.621784821875001281 ) ) ;
#7859 = ORIENTED_EDGE ( 'NONE', *, *, #39854, .T. ) ;
#7860 = CARTESIAN_POINT ( 'NONE',  ( 15.66562500061451857, 3.027376345333613106, -5.243569643749998122 ) ) ;
#7861 = AXIS2_PLACEMENT_3D ( 'NONE', #13302, #57290, #8142 ) ;
#7862 = CARTESIAN_POINT ( 'NONE',  ( 11.09062500061451573, -3.027376345333610441, -5.243569643749999898 ) ) ;
#7863 = CARTESIAN_POINT ( 'NONE',  ( 22.88437500061451857, 5.824947211148865298E-16, -4.756430356249998326 ) ) ;
#7864 = CARTESIAN_POINT ( 'NONE',  ( 10.49999999999999822, 4.330127018922192761, -2.499999999999997780 ) ) ;
#7865 = CARTESIAN_POINT ( 'NONE',  ( 6.337500001229033231, -4.330127018922194537, 2.499999999999995559 ) ) ;
#7866 =( BOUNDED_CURVE ( )  B_SPLINE_CURVE ( 2, ( #44920, #72986, #27926, #17184, #16453, #11657, #23087 ),
 .UNSPECIFIED., .F., .F. ) 
 B_SPLINE_CURVE_WITH_KNOTS ( ( 3, 2, 2, 3 ),
 ( 0.6250000000000000000, 0.6277777777777777679, 0.6305555555555555358, 0.6333333333333333037 ),
 .UNSPECIFIED. ) 
 CURVE ( )  GEOMETRIC_REPRESENTATION_ITEM ( )  RATIONAL_B_SPLINE_CURVE ( ( 1.000000000000000000, 0.8660254037844387076, 1.000000000000000000, 0.8660254037844387076, 1.000000000000000000, 0.8660254037844387076, 1.000000000000000000 ) ) 
 REPRESENTATION_ITEM ( '' )  );
#7867 = CARTESIAN_POINT ( 'NONE',  ( 13.99687500061451928, 6.054752690667223547, 3.707466751127219781E-16 ) ) ;
#7868 = CARTESIAN_POINT ( 'NONE',  ( 17.17500000122903359, -5.773502691896255534, -1.060575238724906372E-15 ) ) ;
#7869 = CARTESIAN_POINT ( 'NONE',  ( 24.78750000000000497, -2.886751345948125991, -5.000000000000000000 ) ) ;
#7870 = CARTESIAN_POINT ( 'NONE',  ( 4.243569643749999898, 18.22812500061451502, -30.00000000000000000 ) ) ;
#7871 = CARTESIAN_POINT ( 'NONE',  ( 16.20000000122903216, -2.886751345948130876, 4.999999999999996447 ) ) ;
#7872 = CARTESIAN_POINT ( 'NONE',  ( 9.975000000000001421, 6.123233995736764310E-16, -4.999999999999998224 ) ) ;
#7873 = DIRECTION ( 'NONE',  ( -1.000000000000000000, -0.000000000000000000, -0.000000000000000000 ) ) ;
#7874 = CARTESIAN_POINT ( 'NONE',  ( 45.00000000000000000, 0.000000000000000000, 0.000000000000000000 ) ) ;
#7875 = CARTESIAN_POINT ( 'NONE',  ( 13.79999999999999893, 0.000000000000000000, 4.999999999999998224 ) ) ;
#7876 = CARTESIAN_POINT ( 'NONE',  ( 18.57187500061451857, 3.027376345333611329, 5.243569643749999010 ) ) ;
#7877 = CARTESIAN_POINT ( 'NONE',  ( 28.04999999999999716, 4.330127018922192761, -2.499999999999997780 ) ) ;
#7878 = EDGE_CURVE ( 'NONE', #36605, #18379, #58554, .T. ) ;
#7879 = CARTESIAN_POINT ( 'NONE',  ( 15.14062500061451644, -3.027376345333610441, -5.243569643749999898 ) ) ;
#7880 = CARTESIAN_POINT ( 'NONE',  ( 9.506250001229030744, -4.330127018922190985, -2.500000000000001332 ) ) ;
#7881 = CARTESIAN_POINT ( 'NONE',  ( 22.95937500061451431, 4.541064518000418104, -2.621784821874998173 ) ) ;
#7882 = CARTESIAN_POINT ( 'NONE',  ( 15.83437500061451253, -2.746126346562646425, 4.756430356249996549 ) ) ;
#7883 = CARTESIAN_POINT ( 'NONE',  ( 10.41562500061451679, 3.027376345333611329, 5.243569643749999010 ) ) ;
#7884 = CARTESIAN_POINT ( 'NONE',  ( 14.63437500061451679, -4.541064518000419881, 2.621784821874995952 ) ) ;
#7885 = EDGE_LOOP ( 'NONE', ( #27374, #49428, #51883 ) ) ;
#7886 = CARTESIAN_POINT ( 'NONE',  ( 25.47187500061451715, -6.054752690667223547, -1.112240025338166033E-15 ) ) ;
#7887 = CARTESIAN_POINT ( 'NONE',  ( 26.31562500061451715, -6.054752690667223547, -1.112240025338166033E-15 ) ) ;
#7888 = CARTESIAN_POINT ( 'NONE',  ( 17.57812500061451644, 4.541064518000418104, 2.621784821874999949 ) ) ;
#7889 = CARTESIAN_POINT ( 'NONE',  ( 29.76562500061451644, 3.027376345333611329, 5.243569643749999010 ) ) ;
#7890 = DIRECTION ( 'NONE',  ( 0.000000000000000000, 1.000000000000000000, -1.040834085586083941E-14 ) ) ;
#7891 = CARTESIAN_POINT ( 'NONE',  ( 10.49999999999999822, 4.330127018922192761, -2.499999999999997780 ) ) ;
#7892 = CARTESIAN_POINT ( 'NONE',  ( 20.55000000122903359, 5.773502691896255534, 3.535250795749688894E-16 ) ) ;
#7893 = CARTESIAN_POINT ( 'NONE',  ( 9.609375000614514661, -5.492252693125287522, -1.008910452111647106E-15 ) ) ;
#7894 = ORIENTED_EDGE ( 'NONE', *, *, #37794, .F. ) ;
#7895 = CARTESIAN_POINT ( 'NONE',  ( 16.98750000000000426, -2.886751345948129988, 4.999999999999997335 ) ) ;
#7896 = CARTESIAN_POINT ( 'NONE',  ( 22.46250000000000213, -5.773502691896255534, -1.060575238724906372E-15 ) ) ;
#7897 = CARTESIAN_POINT ( 'NONE',  ( 19.62187500061451573, -6.054752690667223547, -1.112240025338166033E-15 ) ) ;
#7898 = CARTESIAN_POINT ( 'NONE',  ( 13.71562500061451750, -6.054752690667223547, -1.112240025338166033E-15 ) ) ;
#7899 = ORIENTED_EDGE ( 'NONE', *, *, #3547, .F. ) ;
#7900 = CARTESIAN_POINT ( 'NONE',  ( 2.000000000000001332, 18.46250000122903501, -26.53589838486224650 ) ) ;
#7901 = CARTESIAN_POINT ( 'NONE',  ( 6.628125000614517148, 6.421520780324663323E-16, -5.243569643749999010 ) ) ;
#7902 = CARTESIAN_POINT ( 'NONE',  ( 13.23750000000000071, 5.773502691896255534, 3.535250795749688894E-16 ) ) ;
#7903 = CARTESIAN_POINT ( 'NONE',  ( 29.22187500061451360, 4.119189519843966529, 2.378215178124999607 ) ) ;
#7904 = CARTESIAN_POINT ( 'NONE',  ( -2.121784821874996840, 15.82812500061451644, 33.67503911421598417 ) ) ;
#7905 = CARTESIAN_POINT ( 'NONE',  ( 27.77812500061451573, 6.421520780324663323E-16, -5.243569643749999010 ) ) ;
#7906 = CARTESIAN_POINT ( 'NONE',  ( 8.137500000000002842, -2.886751345948125991, -5.000000000000000000 ) ) ;
#7907 = CARTESIAN_POINT ( 'NONE',  ( 1.878215178124997609, 17.96562499938548285, 33.25316411605952993 ) ) ;
#7908 = CARTESIAN_POINT ( 'NONE',  ( 23.48437500061451644, 4.541064518000418104, 2.621784821874999949 ) ) ;
#7909 = ORIENTED_EDGE ( 'NONE', *, *, #36869, .T. ) ;
#7910 = CARTESIAN_POINT ( 'NONE',  ( 21.02812500061451573, 6.421520780324663323E-16, -5.243569643749999010 ) ) ;
#7911 = CARTESIAN_POINT ( 'NONE',  ( 23.93437500061451573, 4.541064518000418104, 2.621784821874999949 ) ) ;
#7912 = PRODUCT_RELATED_PRODUCT_CATEGORY ( 'part', '', ( #9598 ) ) ;
#7913 = CARTESIAN_POINT ( 'NONE',  ( 4.243569643749999898, 16.42812500061459247, -30.00000000000000000 ) ) ;
#7914 = CARTESIAN_POINT ( 'NONE',  ( 5.503125000614516260, 0.000000000000000000, 5.243569643749999010 ) ) ;
#7915 = CARTESIAN_POINT ( 'NONE',  ( 26.29687500061451644, -2.746126346562646425, 4.756430356249996549 ) ) ;
#7916 = CARTESIAN_POINT ( 'NONE',  ( 24.40312500061451573, 0.000000000000000000, 5.243569643749999010 ) ) ;
#7917 = CARTESIAN_POINT ( 'NONE',  ( 11.48437500061451644, -4.119189519843968306, 2.378215178124996054 ) ) ;
#7918 = CARTESIAN_POINT ( 'NONE',  ( 3.756430356249998770, 15.30312499938548498, 32.16877607737302469 ) ) ;
#7919 = CARTESIAN_POINT ( 'NONE',  ( 17.78437500061451715, -4.541064518000419881, 2.621784821874995952 ) ) ;
#7920 = CARTESIAN_POINT ( 'NONE',  ( 24.87187500061451573, 3.027376345333611329, 5.243569643749999010 ) ) ;
#7921 = CARTESIAN_POINT ( 'NONE',  ( 9.001249775931846008E-16, 15.02187500061451608, 34.90005215228797653 ) ) ;
#7922 = CARTESIAN_POINT ( 'NONE',  ( 6.740625000614516082, 6.054752690667223547, 3.707466751127219781E-16 ) ) ;
#7923 = DIRECTION ( 'NONE',  ( 0.000000000000000000, 0.000000000000000000, 1.000000000000000000 ) ) ;
#7924 = CARTESIAN_POINT ( 'NONE',  ( 28.82812500061451644, 4.541064518000418104, 2.621784821874999949 ) ) ;
#7925 = DIRECTION ( 'NONE',  ( -0.000000000000000000, -1.000000000000000000, -0.000000000000000000 ) ) ;
#7926 = CARTESIAN_POINT ( 'NONE',  ( 5.240625000614516971, -3.027376345333610441, -5.243569643749999898 ) ) ;
#7927 = CARTESIAN_POINT ( 'NONE',  ( 10.69687500061451679, -3.027376345333610441, -5.243569643749999898 ) ) ;
#7928 = CARTESIAN_POINT ( 'NONE',  ( 17.43750000122903288, 4.330127018922191873, 2.499999999999999556 ) ) ;
#7929 = CARTESIAN_POINT ( 'NONE',  ( 29.09062500061451573, -3.027376345333610441, -5.243569643749999898 ) ) ;
#7930 = CARTESIAN_POINT ( 'NONE',  ( 4.115625000614516082, 3.027376345333611329, 5.243569643749999010 ) ) ;
#7931 = CARTESIAN_POINT ( 'NONE',  ( 2.000000000000000444, 14.31874999877096499, 26.53589838486224650 ) ) ;
#7932 = CARTESIAN_POINT ( 'NONE',  ( 20.56875000122903785, 2.886751345948126879, 4.999999999999999112 ) ) ;
#7933 = CARTESIAN_POINT ( 'NONE',  ( 16.88437500061451502, -4.541064518000419881, 2.621784821874995952 ) ) ;
#7934 = CARTESIAN_POINT ( 'NONE',  ( 1.071796769724500997, 19.10134618820330132, 33.99999999999999289 ) ) ;
#7935 = ORIENTED_EDGE ( 'NONE', *, *, #31576, .T. ) ;
#7936 = CARTESIAN_POINT ( 'NONE',  ( 23.09062500061451573, -3.027376345333614438, 5.243569643749998122 ) ) ;
#7937 = CARTESIAN_POINT ( 'NONE',  ( 9.590625000614517504, -3.027376345333614438, 5.243569643749998122 ) ) ;
#7938 = CARTESIAN_POINT ( 'NONE',  ( 25.88437500061451502, -4.541064518000419881, 2.621784821874995952 ) ) ;
#7939 = CARTESIAN_POINT ( 'NONE',  ( 10.41562500061451679, 3.027376345333611329, 5.243569643749999010 ) ) ;
#7940 = CARTESIAN_POINT ( 'NONE',  ( 20.43749999999999645, 5.773502691896255534, 3.535250795749688401E-16 ) ) ;
#7941 = CARTESIAN_POINT ( 'NONE',  ( 9.487500001229033586, -4.330127018922194537, 2.499999999999995559 ) ) ;
#7942 = EDGE_CURVE ( 'NONE', #65447, #18641, #562, .T. ) ;
#7943 = CARTESIAN_POINT ( 'NONE',  ( 25.75312500061451715, 0.000000000000000000, 5.243569643749999010 ) ) ;
#7944 = B_SPLINE_CURVE_WITH_KNOTS ( 'NONE', 3,
 ( #71028, #14138, #8603, #42588, #59562, #63651, #3066, #69573, #35940, #25596 ),
 .UNSPECIFIED., .F., .F.,
 ( 4, 3, 3, 4 ),
 ( 3.881383207071731149E-17, 7.861371910493904853E-05, 0.0001572271722546394167, 0.0002869866954567743423 ),
 .UNSPECIFIED. ) ;
#7945 = CARTESIAN_POINT ( 'NONE',  ( -1.473773219643375931, 9.816672173337614993, -34.04916878720240447 ) ) ;
#7946 = CARTESIAN_POINT ( 'NONE',  ( 12.15000000122903501, -2.886751345948129988, 4.999999999999997335 ) ) ;
#7947 = CARTESIAN_POINT ( 'NONE',  ( 22.11562500061451786, 3.027376345333611329, 5.243569643749999010 ) ) ;
#7948 = CARTESIAN_POINT ( 'NONE',  ( 18.44062500061451715, 6.054752690667223547, 3.707466751127219781E-16 ) ) ;
#7949 = CARTESIAN_POINT ( 'NONE',  ( 5.596875000614516260, -3.027376345333614438, 5.243569643749998122 ) ) ;
#7950 = CARTESIAN_POINT ( 'NONE',  ( 17.73750000000000071, 5.773502691896255534, 3.535250795749688894E-16 ) ) ;
#7951 = CARTESIAN_POINT ( 'NONE',  ( 12.90000000122903145, 5.773502691896255534, 3.535250795749688894E-16 ) ) ;
#7952 = VECTOR ( 'NONE', #48065, 1000.000000000000000 ) ;
#7953 = CARTESIAN_POINT ( 'NONE',  ( 10.75312500061451715, 4.541064518000418104, -2.621784821874998173 ) ) ;
#7954 = CARTESIAN_POINT ( 'NONE',  ( 13.30312500061451786, -4.541064518000417216, -2.621784821875001281 ) ) ;
#7955 = CARTESIAN_POINT ( 'NONE',  ( 23.02500000122903145, -5.773502691896255534, -1.060575238724906372E-15 ) ) ;
#7956 = CARTESIAN_POINT ( 'NONE',  ( 20.89687500061452141, -3.027376345333614438, 5.243569643749998122 ) ) ;
#7957 = CARTESIAN_POINT ( 'NONE',  ( 21.57187500061451502, 3.027376345333613106, -5.243569643749998122 ) ) ;
#7958 = DIRECTION ( 'NONE',  ( 0.000000000000000000, 0.000000000000000000, 1.000000000000000000 ) ) ;
#7959 = EDGE_CURVE ( 'NONE', #65810, #68516, #63056, .T. ) ;
#7960 = CARTESIAN_POINT ( 'NONE',  ( 7.087500001229034119, 4.330127018922191873, 2.499999999999999556 ) ) ;
#7961 = CARTESIAN_POINT ( 'NONE',  ( 7.584375000614516082, 6.421520780324663323E-16, -5.243569643749999010 ) ) ;
#7962 = CARTESIAN_POINT ( 'NONE',  ( 25.69687500061451502, 6.054752690667223547, 3.707466751127219781E-16 ) ) ;
#7963 = LINE ( 'NONE', #53027, #43346 ) ;
#7964 = CARTESIAN_POINT ( 'NONE',  ( 20.80312500061451431, 0.000000000000000000, 5.243569643749999010 ) ) ;
#7965 = CARTESIAN_POINT ( 'NONE',  ( 25.80937500061451928, 0.000000000000000000, 5.243569643749999010 ) ) ;
#7966 = CARTESIAN_POINT ( 'NONE',  ( 3.756430356250000546, 16.39062499938548356, 27.83122392262697886 ) ) ;
#7967 = CARTESIAN_POINT ( 'NONE',  ( 19.03125000122902932, 6.123233995736764310E-16, -4.999999999999998224 ) ) ;
#7968 = CARTESIAN_POINT ( 'NONE',  ( 16.33125000122903359, 6.123233995736764310E-16, -4.999999999999998224 ) ) ;
#7969 = CARTESIAN_POINT ( 'NONE',  ( 6.084375000614518747, -4.541064518000419881, 2.621784821874995952 ) ) ;
#7970 = CARTESIAN_POINT ( 'NONE',  ( 17.16562500061451502, 3.027376345333611329, 5.243569643749999010 ) ) ;
#7971 = EDGE_LOOP ( 'NONE', ( #22359, #27390, #564, #39187 ) ) ;
#7972 = CARTESIAN_POINT ( 'NONE',  ( 25.08749999999999858, -2.886751345948130876, 4.999999999999996447 ) ) ;
#7973 = CARTESIAN_POINT ( 'NONE',  ( 26.09062500061451573, 6.054752690667223547, 3.707466751127219781E-16 ) ) ;
#7974 = CARTESIAN_POINT ( 'NONE',  ( 3.609375000614516882, 4.541064518000418104, -2.621784821874998173 ) ) ;
#7975 = CARTESIAN_POINT ( 'NONE',  ( 10.08750000122903323, 6.123233995736764310E-16, -4.999999999999998224 ) ) ;
#7976 = CARTESIAN_POINT ( 'NONE',  ( 3.701615863222355252, 3.361311753005875591, -3.762615002631680916 ) ) ;
#7977 = CARTESIAN_POINT ( 'NONE',  ( 17.02499999999999858, -4.330127018922194537, 2.499999999999995559 ) ) ;
#7978 = CARTESIAN_POINT ( 'NONE',  ( 20.84062500061451573, -3.027376345333614438, 5.243569643749998122 ) ) ;
#7979 = ORIENTED_EDGE ( 'NONE', *, *, #1706, .F. ) ;
#7980 = CARTESIAN_POINT ( 'NONE',  ( 25.38749999999999929, 5.773502691896255534, 3.535250795749688894E-16 ) ) ;
#7981 = ADVANCED_FACE ( 'NONE', ( #34253 ), #39826, .F. ) ;
#7982 = CARTESIAN_POINT ( 'NONE',  ( 26.78437500061451360, -4.541064518000419881, 2.621784821874995952 ) ) ;
#7983 = VERTEX_POINT ( 'NONE', #17264 ) ;
#7984 = DIRECTION ( 'NONE',  ( -1.000000000000000000, -0.000000000000000000, -0.000000000000000000 ) ) ;
#7985 = CARTESIAN_POINT ( 'NONE',  ( 12.92812500061451786, 6.421520780324663323E-16, -5.243569643749999010 ) ) ;
#7986 = CARTESIAN_POINT ( 'NONE',  ( 6.103125000614515905, -4.541064518000417216, -2.621784821875001281 ) ) ;
#7987 = CARTESIAN_POINT ( 'NONE',  ( 16.77187500061451431, -4.119189519843968306, 2.378215178124996054 ) ) ;
#7988 = CARTESIAN_POINT ( 'NONE',  ( 28.71562500061451573, 3.027376345333613106, -5.243569643749998122 ) ) ;
#7989 = CARTESIAN_POINT ( 'NONE',  ( 16.38750000122903216, 6.123233995736764310E-16, -4.999999999999998224 ) ) ;
#7990 = CARTESIAN_POINT ( 'NONE',  ( 19.23749999999999716, -2.886751345948129988, 4.999999999999997335 ) ) ;
#7991 = CARTESIAN_POINT ( 'NONE',  ( 26.92499999999999716, -4.330127018922194537, 2.499999999999995559 ) ) ;
#7992 = CARTESIAN_POINT ( 'NONE',  ( 3.309375000614518836, 0.000000000000000000, 5.243569643749999010 ) ) ;
#7993 = CARTESIAN_POINT ( 'NONE',  ( 9.009375000614518569, 4.541064518000418104, -2.621784821874998173 ) ) ;
#7994 = CARTESIAN_POINT ( 'NONE',  ( 19.39687500061451786, 6.054752690667223547, 3.707466751127219781E-16 ) ) ;
#7995 = CARTESIAN_POINT ( 'NONE',  ( 19.87500000122903288, -5.773502691896255534, -1.060575238724906372E-15 ) ) ;
#7996 = ORIENTED_EDGE ( 'NONE', *, *, #42304, .T. ) ;
#7997 = CARTESIAN_POINT ( 'NONE',  ( 28.97812500061451502, -4.541064518000419881, 2.621784821874995952 ) ) ;
#7998 = CARTESIAN_POINT ( 'NONE',  ( 3.225000000000002309, 6.123233995736764310E-16, -4.999999999999998224 ) ) ;
#7999 = CARTESIAN_POINT ( 'NONE',  ( 5.109375000614518214, 0.000000000000000000, 5.243569643749999010 ) ) ;
#8000 = VECTOR ( 'NONE', #51648, 1000.000000000000000 ) ;
#8001 = CARTESIAN_POINT ( 'NONE',  ( 16.46249999999999503, 2.886751345948126879, 4.999999999999999112 ) ) ;
#8002 = CARTESIAN_POINT ( 'NONE',  ( 13.90312500061451750, 4.541064518000418104, -2.621784821874998173 ) ) ;
#8003 = CARTESIAN_POINT ( 'NONE',  ( 9.768750001229031810, 2.886751345948126879, 4.999999999999998224 ) ) ;
#8004 = CYLINDRICAL_SURFACE ( 'NONE', #54001, 4.999999999999998224 ) ;
#8005 = CARTESIAN_POINT ( 'NONE',  ( 18.33750000122903501, 4.330127018922191873, 2.499999999999999556 ) ) ;
#8006 = CARTESIAN_POINT ( 'NONE',  ( 4.000000000000000000, 12.89374999877096606, 30.00000000000000000 ) ) ;
#8007 = CARTESIAN_POINT ( 'NONE',  ( 18.53437500061451715, 4.119189519843966529, 2.378215178124999607 ) ) ;
#8008 = CARTESIAN_POINT ( 'NONE',  ( 8.015625000614518214, 3.027376345333613106, -5.243569643749998122 ) ) ;
#8009 = CARTESIAN_POINT ( 'NONE',  ( 23.63437500061451502, -4.541064518000419881, 2.621784821874995952 ) ) ;
#8010 = CARTESIAN_POINT ( 'NONE',  ( -4.243569643749999898, 18.92187500061451644, 27.54997392385601529 ) ) ;
#8011 = CARTESIAN_POINT ( 'NONE',  ( 23.67187500061451999, -6.054752690667223547, -1.112240025338166033E-15 ) ) ;
#8012 = CARTESIAN_POINT ( 'NONE',  ( 7.124999999999999112, -4.330127018922194537, 2.499999999999995559 ) ) ;
#8013 = CARTESIAN_POINT ( 'NONE',  ( -2.828200636599751609E-16, 14.15000000122903501, 25.38119784648299770 ) ) ;
#8014 = CARTESIAN_POINT ( 'NONE',  ( 13.67812500061451786, -4.541064518000419881, 2.621784821874995952 ) ) ;
#8015 = CARTESIAN_POINT ( 'NONE',  ( 7.125000001229033764, 2.886751345948126879, 4.999999999999999112 ) ) ;
#8016 = CARTESIAN_POINT ( 'NONE',  ( 10.77187500061451786, 3.027376345333613106, -5.243569643749998122 ) ) ;
#8017 = CARTESIAN_POINT ( 'NONE',  ( 34.99999999999999289, -6.363961030678871644, 6.363961030678982667 ) ) ;
#8018 = ORIENTED_EDGE ( 'NONE', *, *, #69480, .T. ) ;
#8019 = CARTESIAN_POINT ( 'NONE',  ( 13.11562500061451786, 3.027376345333611329, 5.243569643749999010 ) ) ;
#8020 = CARTESIAN_POINT ( 'NONE',  ( 13.91250000000000142, -5.773502691896255534, -1.060575238724906372E-15 ) ) ;
#8021 = CARTESIAN_POINT ( 'NONE',  ( 24.78750000122903074, -4.330127018922194537, 2.499999999999995559 ) ) ;
#8022 = CARTESIAN_POINT ( 'NONE',  ( 10.84687500061451892, 6.054752690667223547, 3.707466751127219781E-16 ) ) ;
#8023 = CARTESIAN_POINT ( 'NONE',  ( 15.40312500061451573, 0.000000000000000000, 5.243569643749999010 ) ) ;
#8024 = CARTESIAN_POINT ( 'NONE',  ( 27.84375000122903288, -2.886751345948129988, 4.999999999999997335 ) ) ;
#8025 = CARTESIAN_POINT ( 'NONE',  ( 22.88437500061451857, 6.421520780324663323E-16, -5.243569643749999010 ) ) ;
#8026 = CARTESIAN_POINT ( 'NONE',  ( 24.26250000122903216, 0.000000000000000000, 4.999999999999998224 ) ) ;
#8027 = CARTESIAN_POINT ( 'NONE',  ( 9.975000000000001421, 6.123233995736764310E-16, -4.999999999999998224 ) ) ;
#8028 = DIRECTION ( 'NONE',  ( -1.000000000000000000, -0.000000000000000000, -0.000000000000000000 ) ) ;
#8029 = CARTESIAN_POINT ( 'NONE',  ( -3.000416591977282496E-16, 15.24687500061451928, -34.90005215228797653 ) ) ;
#8030 =( BOUNDED_CURVE ( )  B_SPLINE_CURVE ( 2, ( #30191, #52720, #47184, #59338, #19084, #8749, #41639, #13546, #36093 ),
 .UNSPECIFIED., .F., .F. ) 
 B_SPLINE_CURVE_WITH_KNOTS ( ( 3, 2, 2, 2, 3 ),
 ( 0.8194444444444444198, 0.8240740740740740700, 0.8333333333333333703, 0.8425925925925925597, 0.8472222222222222099 ),
 .UNSPECIFIED. ) 
 CURVE ( )  GEOMETRIC_REPRESENTATION_ITEM ( )  RATIONAL_B_SPLINE_CURVE ( ( 0.9330127018922194093, 0.9330127018922194093, 1.000000000000000000, 0.8660254037844387076, 1.000000000000000000, 0.8660254037844387076, 1.000000000000000000, 0.9330127018922194093, 0.9330127018922194093 ) ) 
 REPRESENTATION_ITEM ( '' )  );
#8031 = CARTESIAN_POINT ( 'NONE',  ( 16.58437500061451786, 6.421520780324663323E-16, -5.243569643749999010 ) ) ;
#8032 = CARTESIAN_POINT ( 'NONE',  ( 17.40000000122903145, 5.773502691896255534, 3.535250795749688894E-16 ) ) ;
#8033 = CARTESIAN_POINT ( 'NONE',  ( 13.02187500061451608, 3.027376345333613106, -5.243569643749998122 ) ) ;
#8034 = CARTESIAN_POINT ( 'NONE',  ( -2.121784821874996840, 10.93437500061451928, 33.67503911421598417 ) ) ;
#8035 = CARTESIAN_POINT ( 'NONE',  ( 19.83750000122903145, -4.330127018922194537, 2.499999999999995559 ) ) ;
#8036 = CARTESIAN_POINT ( 'NONE',  ( 12.96562500061451750, 3.027376345333613106, -5.243569643749998122 ) ) ;
#8037 = ORIENTED_EDGE ( 'NONE', *, *, #53290, .F. ) ;
#8038 = ORIENTED_EDGE ( 'NONE', *, *, #72602, .F. ) ;
#8039 = CARTESIAN_POINT ( 'NONE',  ( 16.98750000000000426, -2.886751345948129988, 4.999999999999997335 ) ) ;
#8040 = CARTESIAN_POINT ( 'NONE',  ( 17.88749999999999574, -2.886751345948063374, 5.000000000000112799 ) ) ;
#8041 = CARTESIAN_POINT ( 'NONE',  ( 11.44687500061451679, -3.027376345333614438, 5.243569643749998122 ) ) ;
#8042 = CARTESIAN_POINT ( 'NONE',  ( 0.000000000000000000, 27.50000000000000000, 30.00000000000000000 ) ) ;
#8043 = CARTESIAN_POINT ( 'NONE',  ( 12.56250000122903465, 0.000000000000000000, 4.999999999999998224 ) ) ;
#8044 = CARTESIAN_POINT ( 'NONE',  ( 22.08750000122903501, -4.330127018922194537, 2.499999999999995559 ) ) ;
#8045 = CARTESIAN_POINT ( 'NONE',  ( 16.60312500061451857, 4.541064518000418104, -2.621784821874998173 ) ) ;
#8046 = ADVANCED_FACE ( 'NONE', ( #51260 ), #51627, .T. ) ;
#8047 = CARTESIAN_POINT ( 'NONE',  ( 21.29062500061451502, -3.027376345333614438, 5.243569643749998122 ) ) ;
#8048 = CARTESIAN_POINT ( 'NONE',  ( 27.30000000122903359, 5.773502691896255534, 3.535250795749688894E-16 ) ) ;
#8049 = CARTESIAN_POINT ( 'NONE',  ( 26.43750000000000000, -2.886751345948129988, 4.999999999999997335 ) ) ;
#8050 = CARTESIAN_POINT ( 'NONE',  ( 17.68125000122903501, 6.123233995736764310E-16, -4.999999999999998224 ) ) ;
#8051 = CARTESIAN_POINT ( 'NONE',  ( 29.96250000000000213, 2.886751345948126879, 4.999999999999999112 ) ) ;
#8052 = CARTESIAN_POINT ( 'NONE',  ( 28.32187500061451502, 3.027376345333613106, -5.243569643749998122 ) ) ;
#8053 = CARTESIAN_POINT ( 'NONE',  ( 2.000000000000001332, 14.30000000000000071, -26.53589838486224650 ) ) ;
#8054 = CARTESIAN_POINT ( 'NONE',  ( 2.121784821875001281, 16.85937500061451999, -26.32496088578401938 ) ) ;
#8055 = CARTESIAN_POINT ( 'NONE',  ( 2.662500001229036073, 0.000000000000000000, 4.999999999999998224 ) ) ;
#8056 = CARTESIAN_POINT ( 'NONE',  ( 5.887500000000000178, -2.886751345948125991, -5.000000000000000000 ) ) ;
#8057 = LINE ( 'NONE', #64567, #38452 ) ;
#8058 = CARTESIAN_POINT ( 'NONE',  ( 10.77187500061451786, 3.027376345333613106, -5.243569643749998122 ) ) ;
#8059 = CARTESIAN_POINT ( 'NONE',  ( 28.67812500061451431, 6.421520780324663323E-16, -5.243569643749999010 ) ) ;
#8060 = CARTESIAN_POINT ( 'NONE',  ( 15.50625000122903430, 4.330127018922192761, -2.499999999999997780 ) ) ;
#8061 = CARTESIAN_POINT ( 'NONE',  ( -0.8062380997993551235, 9.975217491784283297, -35.95894923966248058 ) ) ;
#8062 = DIRECTION ( 'NONE',  ( 0.000000000000000000, -1.000000000000000000, 8.673617379884035472E-17 ) ) ;
#8063 = CARTESIAN_POINT ( 'NONE',  ( 6.796875000614516438, 6.054752690667223547, 3.707466751127219781E-16 ) ) ;
#8064 = CARTESIAN_POINT ( 'NONE',  ( 11.29687500061451644, 6.054752690667223547, 3.707466751127219781E-16 ) ) ;
#8065 = CARTESIAN_POINT ( 'NONE',  ( 4.462500000000001243, -5.773502691896255534, -1.060575238724906372E-15 ) ) ;
#8066 =( BOUNDED_CURVE ( )  B_SPLINE_CURVE ( 2, ( #55159, #48519, #37428, #54064, #42969, #48885, #25613 ),
 .UNSPECIFIED., .F., .F. ) 
 B_SPLINE_CURVE_WITH_KNOTS ( ( 3, 2, 2, 3 ),
 ( 0.08333333333333328707, 0.08611111111111106886, 0.08888888888888883677, 0.09166666666666660468 ),
 .UNSPECIFIED. ) 
 CURVE ( )  GEOMETRIC_REPRESENTATION_ITEM ( )  RATIONAL_B_SPLINE_CURVE ( ( 1.000000000000001998, 0.8660254037844365982, 1.000000000000000000, 0.8660254037844387076, 1.000000000000000000, 0.8660254037844413721, 0.9999999999999973355 ) ) 
 REPRESENTATION_ITEM ( '' )  );
#8067 = EDGE_CURVE ( 'NONE', #48464, #34596, #6919, .T. ) ;
#8068 = CARTESIAN_POINT ( 'NONE',  ( 4.243569643749999898, 15.49062500061459779, 32.45002607614398471 ) ) ;
#8069 = CARTESIAN_POINT ( 'NONE',  ( 0.2617799820177835191, 25.54316770519903201, 34.00000000000000000 ) ) ;
#8070 = CARTESIAN_POINT ( 'NONE',  ( 5.362500000000003375, -5.773502691896255534, -1.060575238724906372E-15 ) ) ;
#8071 = CARTESIAN_POINT ( 'NONE',  ( 14.74687500061451573, 4.119189519843966529, -2.378215178124998275 ) ) ;
#8072 = CARTESIAN_POINT ( 'NONE',  ( 19.67812500061451786, 6.421520780324663323E-16, -5.243569643749999010 ) ) ;
#8073 = CARTESIAN_POINT ( 'NONE',  ( 13.82812500061451466, 6.421520780324663323E-16, -5.243569643749999010 ) ) ;
#8074 = CARTESIAN_POINT ( 'NONE',  ( 22.58437500061451786, -2.746126346562646425, 4.756430356249996549 ) ) ;
#8075 = CARTESIAN_POINT ( 'NONE',  ( 9.946875000614516793, 6.054752690667223547, 3.707466751127219781E-16 ) ) ;
#8076 = CARTESIAN_POINT ( 'NONE',  ( 25.61250000000000071, -5.773502691896255534, -1.060575238724906372E-15 ) ) ;
#8077 = CARTESIAN_POINT ( 'NONE',  ( 23.73750000122903359, 4.330127018922191873, 2.499999999999999556 ) ) ;
#8078 = CARTESIAN_POINT ( 'NONE',  ( 16.94999999999999929, 0.000000000000000000, 4.999999999999998224 ) ) ;
#8079 = CARTESIAN_POINT ( 'NONE',  ( 9.271875000614516082, -6.054752690667223547, -1.112240025338166033E-15 ) ) ;
#8080 = CARTESIAN_POINT ( 'NONE',  ( 25.43437500061451573, -4.541064518000419881, 2.621784821874995952 ) ) ;
#8081 = CARTESIAN_POINT ( 'NONE',  ( 23.68125000122903145, 4.330127018922191873, 2.499999999999999556 ) ) ;
#8082 = EDGE_CURVE ( 'NONE', #67338, #70443, #65705, .T. ) ;
#8083 = CARTESIAN_POINT ( 'NONE',  ( -3.999999999999999112, 12.91250000122903430, -30.00000000000000000 ) ) ;
#8084 = CARTESIAN_POINT ( 'NONE',  ( 20.44687500061451857, -3.027376345333614438, 5.243569643749998122 ) ) ;
#8085 = CARTESIAN_POINT ( 'NONE',  ( 10.95937500061451964, 0.000000000000000000, 5.243569643749999010 ) ) ;
#8086 = CARTESIAN_POINT ( 'NONE',  ( -3.756430356250001434, 13.35312499938548392, 32.16877607737301048 ) ) ;
#8087 = CARTESIAN_POINT ( 'NONE',  ( 22.64999999999999858, 4.330127018922192761, -2.499999999999997780 ) ) ;
#8088 = CARTESIAN_POINT ( 'NONE',  ( 4.000000000000000000, 12.98749999999999893, 27.69059892324149530 ) ) ;
#8089 = CARTESIAN_POINT ( 'NONE',  ( 9.001249775931846008E-16, 12.32187500061451857, -25.09994784771203058 ) ) ;
#8090 = CARTESIAN_POINT ( 'NONE',  ( 23.93437500061451573, 4.119189519843966529, 2.378215178124999607 ) ) ;
#8091 = CARTESIAN_POINT ( 'NONE',  ( 15.96562500061451573, -6.054752690667223547, -1.112240025338166033E-15 ) ) ;
#8092 = CARTESIAN_POINT ( 'NONE',  ( 5.137500000000000178, 5.773502691896255534, 3.535250795749688894E-16 ) ) ;
#8093 = CARTESIAN_POINT ( 'NONE',  ( -4.000000000000000000, 18.12500000000000355, 30.00000000000000000 ) ) ;
#8094 = DIRECTION ( 'NONE',  ( -0.000000000000000000, -1.000000000000000000, -0.000000000000000000 ) ) ;
#8095 = CARTESIAN_POINT ( 'NONE',  ( 13.68750000000000178, 5.773502691896255534, 3.535250795749688894E-16 ) ) ;
#8096 = CARTESIAN_POINT ( 'NONE',  ( 3.999999999999998668, 19.47500000122903430, 27.69059892324149175 ) ) ;
#8098 =( BOUNDED_CURVE ( )  B_SPLINE_CURVE ( 1, ( #50986, #45087 ),
 .UNSPECIFIED., .F., .F. ) 
 B_SPLINE_CURVE_WITH_KNOTS ( ( 2, 2 ),
 ( 0.000000000000000000, 1.000000000000000000 ),
 .UNSPECIFIED. ) 
 CURVE ( )  GEOMETRIC_REPRESENTATION_ITEM ( )  RATIONAL_B_SPLINE_CURVE ( ( 0.9401540804404022733, 0.9401540804404022733 ) ) 
 REPRESENTATION_ITEM ( '' )  );
#8097 = CARTESIAN_POINT ( 'NONE',  ( 13.57500000122903572, -5.773502691896255534, -1.060575238724906372E-15 ) ) ;
#8099 = CARTESIAN_POINT ( 'NONE',  ( 24.45937500061451786, 0.000000000000000000, 5.243569643749999010 ) ) ;
#8100 = CARTESIAN_POINT ( 'NONE',  ( 50.00000000000000000, 5.218601775200211179, 7.332543590861028804 ) ) ;
#8101 = ORIENTED_EDGE ( 'NONE', *, *, #39400, .T. ) ;
#8102 = CARTESIAN_POINT ( 'NONE',  ( 18.40312500061451573, 4.541064518000418104, -2.621784821874998173 ) ) ;
#8103 = CARTESIAN_POINT ( 'NONE',  ( 3.515625000614516882, 3.027376345333613106, -5.243569643749998122 ) ) ;
#8104 = CARTESIAN_POINT ( 'NONE',  ( 18.83437500061451431, 6.421520780324663323E-16, -5.243569643749999010 ) ) ;
#8105 = CARTESIAN_POINT ( 'NONE',  ( 29.67187500061451644, 3.027376345333613106, -5.243569643749998122 ) ) ;
#8106 = CARTESIAN_POINT ( 'NONE',  ( 4.453125000614517326, 4.541064518000418104, -2.621784821874998173 ) ) ;
#8107 = CARTESIAN_POINT ( 'NONE',  ( 22.00312500061451360, 4.541064518000418104, -2.621784821874998173 ) ) ;
#8108 = CARTESIAN_POINT ( 'NONE',  ( -2.121784821874999949, 15.67812500061451608, 26.32496088578401938 ) ) ;
#8109 = CARTESIAN_POINT ( 'NONE',  ( 19.91250000122903074, -4.330127018922190985, -2.500000000000001332 ) ) ;
#8110 = CARTESIAN_POINT ( 'NONE',  ( 12.45937500061451786, -4.119189519843965641, -2.378215178125001383 ) ) ;
#8111 = CARTESIAN_POINT ( 'NONE',  ( 5.953125000614519102, 0.000000000000000000, 5.243569643749999010 ) ) ;
#8112 = EDGE_CURVE ( 'NONE', #37474, #43716, #20388, .T. ) ;
#8113 = CARTESIAN_POINT ( 'NONE',  ( 13.72500000000000142, 4.330127018922191873, 2.499999999999999556 ) ) ;
#8114 = CARTESIAN_POINT ( 'NONE',  ( 2.934375000614518392, -4.541064518000419881, 2.621784821874995952 ) ) ;
#8115 = CARTESIAN_POINT ( 'NONE',  ( 21.79687500061451644, -3.027376345333614438, 5.243569643749998122 ) ) ;
#8116 = CARTESIAN_POINT ( 'NONE',  ( 15.14062500061451644, -3.027376345333610441, -5.243569643749999898 ) ) ;
#8117 = CARTESIAN_POINT ( 'NONE',  ( 25.83750000122903501, 6.123233995736764310E-16, -4.999999999999998224 ) ) ;
#8118 = CARTESIAN_POINT ( 'NONE',  ( 26.57812500061451644, 4.541064518000418104, 2.621784821874999949 ) ) ;
#8119 = CARTESIAN_POINT ( 'NONE',  ( 19.77187500061451786, 3.027376345333613106, -5.243569643749998122 ) ) ;
#8120 = CARTESIAN_POINT ( 'NONE',  ( 14.95312500061451644, 0.000000000000000000, 5.243569643749999010 ) ) ;
#8121 = CARTESIAN_POINT ( 'NONE',  ( 4.243569643749999898, 16.03437500061451715, 30.00000000000000000 ) ) ;
#8122 =( BOUNDED_CURVE ( )  B_SPLINE_CURVE ( 2, ( #40385, #40754, #24828, #30012, #1961, #7125, #1234, #19273, #47016 ),
 .UNSPECIFIED., .F., .F. ) 
 B_SPLINE_CURVE_WITH_KNOTS ( ( 3, 2, 2, 2, 3 ),
 ( 0.9239130434782608647, 0.9275362318840579823, 0.9347826086956522174, 0.9420289855072463414, 0.9456521739130434590 ),
 .UNSPECIFIED. ) 
 CURVE ( )  GEOMETRIC_REPRESENTATION_ITEM ( )  RATIONAL_B_SPLINE_CURVE ( ( 0.9330127018922194093, 0.9330127018922194093, 1.000000000000000000, 0.8660254037844387076, 1.000000000000000000, 0.8660254037844387076, 1.000000000000000000, 0.9330127018922194093, 0.9330127018922194093 ) ) 
 REPRESENTATION_ITEM ( '' )  );
#8123 = CARTESIAN_POINT ( 'NONE',  ( 19.86562500061451786, 3.027376345333611329, 5.243569643749999010 ) ) ;
#8124 = CARTESIAN_POINT ( 'NONE',  ( 28.60312500061451502, -4.541064518000417216, -2.621784821875001281 ) ) ;
#8125 = VERTEX_POINT ( 'NONE', #39092 ) ;
#8126 = CARTESIAN_POINT ( 'NONE',  ( 25.16249999999999432, -5.773502691896255534, -1.060575238724906372E-15 ) ) ;
#8127 = CARTESIAN_POINT ( 'NONE',  ( -2.000000000000000000, 10.47500000000000142, -33.46410161513775705 ) ) ;
#8128 = CARTESIAN_POINT ( 'NONE',  ( -1.878215178125001827, 19.35312499938548214, 33.25316411605952283 ) ) ;
#8129 = CARTESIAN_POINT ( 'NONE',  ( 26.39062500061451644, -3.027376345333610441, -5.243569643749999898 ) ) ;
#8130 = CARTESIAN_POINT ( 'NONE',  ( 7.078125000614516438, 6.421520780324663323E-16, -5.243569643749999010 ) ) ;
#8131 = CARTESIAN_POINT ( 'NONE',  ( 20.77500000122903145, -5.773502691896255534, -1.060575238724906372E-15 ) ) ;
#8132 = EDGE_CURVE ( 'NONE', #44451, #10990, #41847, .T. ) ;
#8133 = CARTESIAN_POINT ( 'NONE',  ( 25.30312500061451431, 0.000000000000000000, 5.243569643749999010 ) ) ;
#8134 = CARTESIAN_POINT ( 'NONE',  ( 24.60000000000000142, 0.000000000000000000, 4.999999999999998224 ) ) ;
#8135 = CARTESIAN_POINT ( 'NONE',  ( 1.999999999999998668, 16.81250000122903643, -33.46410161513775705 ) ) ;
#8136 = CARTESIAN_POINT ( 'NONE',  ( 28.90312500061451217, 0.000000000000000000, 5.243569643749999010 ) ) ;
#8137 = CARTESIAN_POINT ( 'NONE',  ( 10.90312500061451928, 0.000000000000000000, 5.243569643749999010 ) ) ;
#8138 = ORIENTED_EDGE ( 'NONE', *, *, #48242, .F. ) ;
#8139 = CARTESIAN_POINT ( 'NONE',  ( 24.59062500061451573, -3.027376345333610441, -5.243569643749999898 ) ) ;
#8140 = CARTESIAN_POINT ( 'NONE',  ( 4.903125000614516615, 4.541064518000418104, -2.621784821874998173 ) ) ;
#8141 = CARTESIAN_POINT ( 'NONE',  ( 13.92187500061451644, 2.746126346562645981, -4.756430356249997438 ) ) ;
#8142 = DIRECTION ( 'NONE',  ( 0.000000000000000000, 0.000000000000000000, -1.000000000000000000 ) ) ;
#8143 = CARTESIAN_POINT ( 'NONE',  ( 12.22499999999999964, 6.123233995736764310E-16, -4.999999999999998224 ) ) ;
#8144 = CARTESIAN_POINT ( 'NONE',  ( 13.43437500061451750, 6.421520780324663323E-16, -5.243569643749999010 ) ) ;
#8145 = CARTESIAN_POINT ( 'NONE',  ( 10.01250000122903394, -4.330127018922190985, -2.500000000000001332 ) ) ;
#8146 = CARTESIAN_POINT ( 'NONE',  ( 16.84687500061451715, -3.027376345333614438, 5.243569643749998122 ) ) ;
#8147 = CARTESIAN_POINT ( 'NONE',  ( 14.88750000000000107, -2.886751345948125991, -5.000000000000000000 ) ) ;
#8148 = CARTESIAN_POINT ( 'NONE',  ( 7.809375000614519280, 0.000000000000000000, 5.243569643749999010 ) ) ;
#8149 = CARTESIAN_POINT ( 'NONE',  ( 4.243569643749999898, 12.37812500061451715, -30.00000000000000000 ) ) ;
#8150 = CARTESIAN_POINT ( 'NONE',  ( 24.67500000000000071, -4.330127018922194537, 2.499999999999995559 ) ) ;
#8151 = CARTESIAN_POINT ( 'NONE',  ( 22.99687500061451573, 0.000000000000000000, 4.756430356249998326 ) ) ;
#8152 = ORIENTED_EDGE ( 'NONE', *, *, #60122, .T. ) ;
#8153 = CARTESIAN_POINT ( 'NONE',  ( 25.45312500061451644, -4.541064518000417216, -2.621784821875001281 ) ) ;
#8154 = FACE_OUTER_BOUND ( 'NONE', #69900, .T. ) ;
#8155 = CARTESIAN_POINT ( 'NONE',  ( 27.12187500061451573, 3.027376345333611329, 5.243569643749999010 ) ) ;
#8156 = CARTESIAN_POINT ( 'NONE',  ( 28.09687500061451360, -3.027376345333614438, 5.243569643749998122 ) ) ;
#8157 = CARTESIAN_POINT ( 'NONE',  ( 4.153125000614515727, 0.000000000000000000, 5.243569643749999010 ) ) ;
#8158 = CARTESIAN_POINT ( 'NONE',  ( 22.17187500061451644, -4.119189519843968306, 2.378215178124996054 ) ) ;
#8159 = CARTESIAN_POINT ( 'NONE',  ( 16.95937500061451786, -4.541064518000417216, -2.621784821875001281 ) ) ;
#8160 = CARTESIAN_POINT ( 'NONE',  ( 7.959375000614516971, 2.746126346562645981, -4.756430356249997438 ) ) ;
#8161 = CARTESIAN_POINT ( 'NONE',  ( 29.28750000122903074, -4.330127018922194537, 2.499999999999995559 ) ) ;
#8162 = CARTESIAN_POINT ( 'NONE',  ( 7.809375000614519280, 0.000000000000000000, 5.243569643749999010 ) ) ;
#8163 = CARTESIAN_POINT ( 'NONE',  ( 18.68437500061451928, -4.541064518000419881, 2.621784821874995952 ) ) ;
#8164 = CARTESIAN_POINT ( 'NONE',  ( -3.012979756977046897, 25.23363074891087265, 27.35627862958216738 ) ) ;
#8165 = CARTESIAN_POINT ( 'NONE',  ( 26.13749999999999929, -2.886751345948125991, -5.000000000000000000 ) ) ;
#8166 = CARTESIAN_POINT ( 'NONE',  ( 27.04687500061451644, 6.054752690667223547, 3.707466751127219781E-16 ) ) ;
#8167 = CARTESIAN_POINT ( 'NONE',  ( 4.000000000000000000, 10.28750000000000142, -27.69059892324149885 ) ) ;
#8168 = CARTESIAN_POINT ( 'NONE',  ( 29.92500000000000071, 4.330127018922191873, 2.499999999999999556 ) ) ;
#8169 = ORIENTED_EDGE ( 'NONE', *, *, #30275, .T. ) ;
#8170 = CARTESIAN_POINT ( 'NONE',  ( 7.425000000000000711, 4.330127018922191873, 2.499999999999999556 ) ) ;
#8171 = CARTESIAN_POINT ( 'NONE',  ( 8.484375000614518214, 5.492252693125287522, 3.363034840372157021E-16 ) ) ;
#8172 = CARTESIAN_POINT ( 'NONE',  ( 21.14062500061451289, 6.054752690667223547, 3.707466751127219781E-16 ) ) ;
#8173 = CARTESIAN_POINT ( 'NONE',  ( 12.33750000000000036, 5.773502691896255534, 3.535250795749688894E-16 ) ) ;
#8174 = CARTESIAN_POINT ( 'NONE',  ( 9.150000001229033231, -2.886751345948125991, -5.000000000000000000 ) ) ;
#8175 = CARTESIAN_POINT ( 'NONE',  ( 5.840625000614516615, 6.054752690667223547, 3.707466751127219781E-16 ) ) ;
#8176 = CARTESIAN_POINT ( 'NONE',  ( 21.33749999999999858, 5.773502691896255534, 3.535250795749688894E-16 ) ) ;
#8177 = CARTESIAN_POINT ( 'NONE',  ( 18.36562500061451431, 3.027376345333613106, -5.243569643749998122 ) ) ;
#8178 = CARTESIAN_POINT ( 'NONE',  ( 4.762500001229033941, 4.330127018922192761, -2.499999999999997780 ) ) ;
#8179 = CARTESIAN_POINT ( 'NONE',  ( 25.83750000122903501, 6.123233995736764310E-16, -4.999999999999998224 ) ) ;
#8180 = CARTESIAN_POINT ( 'NONE',  ( 1.878215178124997609, 18.41562499938548214, 33.25316411605952993 ) ) ;
#8181 = CARTESIAN_POINT ( 'NONE',  ( 3.900000000000000799, 0.000000000000000000, 4.999999999999998224 ) ) ;
#8182 = ORIENTED_EDGE ( 'NONE', *, *, #4284, .T. ) ;
#8183 = CARTESIAN_POINT ( 'NONE',  ( 19.71562500061451928, 3.027376345333613106, -5.243569643749998122 ) ) ;
#8184 = CARTESIAN_POINT ( 'NONE',  ( 26.72812500061451502, -4.541064518000419881, 2.621784821874995952 ) ) ;
#8185 = CARTESIAN_POINT ( 'NONE',  ( 27.30937500061451573, -4.541064518000417216, -2.621784821875001281 ) ) ;
#8186 = CARTESIAN_POINT ( 'NONE',  ( 9.862500000000000711, -5.773502691896255534, -1.060575238724906372E-15 ) ) ;
#8187 = CARTESIAN_POINT ( 'NONE',  ( 13.56562500061451892, 3.027376345333611329, 5.243569643749999010 ) ) ;
#8188 = CARTESIAN_POINT ( 'NONE',  ( 28.04062500061451502, -3.027376345333614438, 5.243569643749998122 ) ) ;
#8189 = EDGE_CURVE ( 'NONE', #41205, #2641, #69341, .T. ) ;
#8190 = CARTESIAN_POINT ( 'NONE',  ( 10.15312500061451750, -4.541064518000417216, -2.621784821875001281 ) ) ;
#8191 = CARTESIAN_POINT ( 'NONE',  ( 14.15625000122903288, 4.330127018922192761, -2.499999999999997780 ) ) ;
#8192 = CARTESIAN_POINT ( 'NONE',  ( 2.121784821874999061, 13.40937500061451892, 26.32496088578401583 ) ) ;
#8193 = CARTESIAN_POINT ( 'NONE',  ( 26.92500000122903359, 2.886751345948126879, 4.999999999999999112 ) ) ;
#8194 = CARTESIAN_POINT ( 'NONE',  ( 19.39687500061451786, 5.492252693125287522, 3.363034840372157021E-16 ) ) ;
#8195 = CARTESIAN_POINT ( 'NONE',  ( 16.67812500061451786, 4.541064518000418104, 2.621784821874999949 ) ) ;
#8196 = DIRECTION ( 'NONE',  ( -0.000000000000000000, -1.000000000000000000, -0.000000000000000000 ) ) ;
#8197 = CARTESIAN_POINT ( 'NONE',  ( 10.05937500061451750, 0.000000000000000000, 5.243569643749999010 ) ) ;
#8198 = CARTESIAN_POINT ( 'NONE',  ( 9.796875000614519990, -3.027376345333610441, -5.243569643749999898 ) ) ;
#8199 = CARTESIAN_POINT ( 'NONE',  ( 18.38437500061451857, 6.421520780324663323E-16, -5.243569643749999010 ) ) ;
#8200 = EDGE_LOOP ( 'NONE', ( #41656, #25321, #68798, #8038 ) ) ;
#8201 = CARTESIAN_POINT ( 'NONE',  ( -0.8069677186600735519, 9.969399234781874952, 35.94888112490725263 ) ) ;
#8202 = CARTESIAN_POINT ( 'NONE',  ( 21.06562500061451715, 3.027376345333613106, -5.243569643749998122 ) ) ;
#8203 = CARTESIAN_POINT ( 'NONE',  ( 16.28437500061452070, 4.541064518000418104, 2.621784821874999949 ) ) ;
#8204 = CARTESIAN_POINT ( 'NONE',  ( 22.56562500061451715, 3.027376345333611329, 5.243569643749999010 ) ) ;
#8205 = CARTESIAN_POINT ( 'NONE',  ( 3.999999999999998668, 15.31250000000000000, 27.69059892324149175 ) ) ;
#8206 = CARTESIAN_POINT ( 'NONE',  ( 27.85312500061451502, 4.541064518000418104, -2.621784821874998173 ) ) ;
#8207 = CARTESIAN_POINT ( 'NONE',  ( 8.325000001229033941, 2.886751345948129099, -4.999999999999998224 ) ) ;
#8208 = ORIENTED_EDGE ( 'NONE', *, *, #26740, .T. ) ;
#8209 = CARTESIAN_POINT ( 'NONE',  ( 4.050000001229035362, -2.886751345948129988, 4.999999999999997335 ) ) ;
#8210 = CARTESIAN_POINT ( 'NONE',  ( -2.828200636599751609E-16, 16.73750000000000071, -34.61880215351700230 ) ) ;
#8211 = CARTESIAN_POINT ( 'NONE',  ( 24.30000000122903359, -2.886751345948129988, 4.999999999999997335 ) ) ;
#8212 = CARTESIAN_POINT ( 'NONE',  ( 1.878215178125000495, 12.82812499938548356, 26.74683588394047007 ) ) ;
#8213 = CARTESIAN_POINT ( 'NONE',  ( 7.021875000614518747, -6.054752690667223547, -1.112240025338166033E-15 ) ) ;
#8214 = CARTESIAN_POINT ( 'NONE',  ( 2.000000000000001332, 15.20000000000000107, 33.46410161513774995 ) ) ;
#8215 = CARTESIAN_POINT ( 'NONE',  ( 15.89062500061451289, -3.027376345333614438, 5.243569643749998122 ) ) ;
#8216 = CARTESIAN_POINT ( 'NONE',  ( 8.259375000614518569, 0.000000000000000000, 5.243569643749999010 ) ) ;
#8217 = ADVANCED_FACE ( 'NONE', ( #40540 ), #33531, .T. ) ;
#8218 = CARTESIAN_POINT ( 'NONE',  ( 27.71250000122903145, 4.330127018922192761, -2.499999999999997780 ) ) ;
#8219 = CARTESIAN_POINT ( 'NONE',  ( 17.40937500061451715, -4.541064518000417216, -2.621784821875001281 ) ) ;
#8220 = CARTESIAN_POINT ( 'NONE',  ( 5.371875000614516615, 3.027376345333613106, -5.243569643749998122 ) ) ;
#8221 = FACE_OUTER_BOUND ( 'NONE', #62873, .T. ) ;
#8222 = CARTESIAN_POINT ( 'NONE',  ( 7.528125000614515727, 6.421520780324663323E-16, -5.243569643749999010 ) ) ;
#8223 = CARTESIAN_POINT ( 'NONE',  ( 16.71562500061451573, 3.027376345333611329, 5.243569643749999010 ) ) ;
#8224 = EDGE_CURVE ( 'NONE', #68516, #44765, #15645, .T. ) ;
#8225 = VERTEX_POINT ( 'NONE', #58230 ) ;
#8226 = CARTESIAN_POINT ( 'NONE',  ( 13.26562500061451644, -6.054752690667223547, -1.112240025338166033E-15 ) ) ;
#8227 = CARTESIAN_POINT ( 'NONE',  ( 6.450000001229034829, -2.886751345948125991, -5.000000000000000000 ) ) ;
#8228 = CARTESIAN_POINT ( 'NONE',  ( 10.82812500061451644, 4.541064518000418104, 2.621784821874999949 ) ) ;
#8229 = CARTESIAN_POINT ( 'NONE',  ( 20.78437500061451715, 4.119189519843966529, 2.378215178124999607 ) ) ;
#8230 = CARTESIAN_POINT ( 'NONE',  ( 10.27499999999999858, -4.330127018922194537, 2.499999999999995559 ) ) ;
#8231 = CARTESIAN_POINT ( 'NONE',  ( 6.150000001229033231, 5.773502691896255534, 3.535250795749688894E-16 ) ) ;
#8232 = CARTESIAN_POINT ( 'NONE',  ( 15.00937500061451679, 0.000000000000000000, 5.243569643749999010 ) ) ;
#8233 = CARTESIAN_POINT ( 'NONE',  ( 15.11250000122903359, 4.330127018922192761, -2.499999999999997780 ) ) ;
#8234 = CARTESIAN_POINT ( 'NONE',  ( 24.48749999999999716, 5.773502691896255534, 3.535250795749688894E-16 ) ) ;
#8235 = CARTESIAN_POINT ( 'NONE',  ( -4.243569643749999898, 18.41562500061451857, -32.45002607614398471 ) ) ;
#8236 = CARTESIAN_POINT ( 'NONE',  ( 30.00000000000000000, 0.000000000000000000, 4.999999999999998224 ) ) ;
#8237 = DIRECTION ( 'NONE',  ( -1.000000000000000000, -0.000000000000000000, -0.000000000000000000 ) ) ;
#8238 = PLANE ( 'NONE',  #60689 ) ;
#8239 = CARTESIAN_POINT ( 'NONE',  ( 4.000000000000000000, 10.85000000122903430, -27.69059892324149885 ) ) ;
#8240 = CARTESIAN_POINT ( 'NONE',  ( 18.80625000122903501, 0.000000000000000000, 4.999999999999998224 ) ) ;
#8241 = CARTESIAN_POINT ( 'NONE',  ( 16.73437500061451644, 4.541064518000418104, 2.621784821874999949 ) ) ;
#8242 =( BOUNDED_CURVE ( )  B_SPLINE_CURVE ( 2, ( #30310, #52480, #68754, #70192, #46944, #69481, #18838 ),
 .UNSPECIFIED., .F., .F. ) 
 B_SPLINE_CURVE_WITH_KNOTS ( ( 3, 2, 2, 3 ),
 ( 0.6250000000000000000, 0.6277777777777777679, 0.6305555555555555358, 0.6333333333333333037 ),
 .UNSPECIFIED. ) 
 CURVE ( )  GEOMETRIC_REPRESENTATION_ITEM ( )  RATIONAL_B_SPLINE_CURVE ( ( 1.000000000000000000, 0.8660254037844387076, 1.000000000000000000, 0.8660254037844387076, 1.000000000000000000, 0.8660254037844387076, 1.000000000000000000 ) ) 
 REPRESENTATION_ITEM ( '' )  );
#8243 = CARTESIAN_POINT ( 'NONE',  ( 29.84999999999999787, 4.330127018922192761, -2.499999999999997780 ) ) ;
#8244 = CARTESIAN_POINT ( 'NONE',  ( 11.91562500061451857, -6.054752690667223547, -1.112240025338166033E-15 ) ) ;
#8245 = CARTESIAN_POINT ( 'NONE',  ( 29.33437500061451431, -2.746126346562646425, 4.756430356249996549 ) ) ;
#8246 = CARTESIAN_POINT ( 'NONE',  ( 23.70937500061451786, -4.541064518000417216, -2.621784821875001281 ) ) ;
#8247 = CARTESIAN_POINT ( 'NONE',  ( 15.38437500061451679, -2.746126346562646425, 4.756430356249996549 ) ) ;
#8248 = CARTESIAN_POINT ( 'NONE',  ( 9.590625000614517504, -3.027376345333614438, 5.243569643749998122 ) ) ;
#8249 = CARTESIAN_POINT ( 'NONE',  ( 14.40937500061451715, 4.541064518000418104, -2.621784821874998173 ) ) ;
#8250 = ORIENTED_EDGE ( 'NONE', *, *, #7387, .T. ) ;
#8251 = CARTESIAN_POINT ( 'NONE',  ( 25.80937500061451928, 0.000000000000000000, 5.243569643749999010 ) ) ;
#8252 = CARTESIAN_POINT ( 'NONE',  ( 28.22812500061451502, 6.421520780324663323E-16, -5.243569643749999010 ) ) ;
#8253 = CARTESIAN_POINT ( 'NONE',  ( 17.87812500061451715, 6.421520780324663323E-16, -5.243569643749999010 ) ) ;
#8254 = CARTESIAN_POINT ( 'NONE',  ( 28.37812500061451715, 4.541064518000418104, 2.621784821874999949 ) ) ;
#8255 = CARTESIAN_POINT ( 'NONE',  ( 4.844509297411972781, 1.237226603047926421, -5.095516945469514170 ) ) ;
#8256 = CARTESIAN_POINT ( 'NONE',  ( 7.050000000000000711, 0.000000000000000000, 4.999999999999998224 ) ) ;
#8257 = CARTESIAN_POINT ( 'NONE',  ( 19.80000000122903359, -2.886751345948129988, 4.999999999999997335 ) ) ;
#8258 = DIRECTION ( 'NONE',  ( -0.000000000000000000, -1.000000000000000000, -0.000000000000000000 ) ) ;
#8259 = CARTESIAN_POINT ( 'NONE',  ( 8.446875000614515017, 4.119189519843966529, -2.378215178124998275 ) ) ;
#8260 = ORIENTED_EDGE ( 'NONE', *, *, #52094, .F. ) ;
#8261 = CARTESIAN_POINT ( 'NONE',  ( 14.02499999999999858, 6.123233995736764310E-16, -4.999999999999998224 ) ) ;
#8262 = CARTESIAN_POINT ( 'NONE',  ( 19.76250000000000639, -5.773502691896255534, -1.060575238724906372E-15 ) ) ;
#8263 = CARTESIAN_POINT ( 'NONE',  ( 16.35937500061451644, 0.000000000000000000, 5.243569643749999010 ) ) ;
#8264 = CARTESIAN_POINT ( 'NONE',  ( 12.81562500061451537, -6.054752690667223547, -1.112240025338166033E-15 ) ) ;
#8265 = ORIENTED_EDGE ( 'NONE', *, *, #163, .T. ) ;
#8266 = CARTESIAN_POINT ( 'NONE',  ( 10.27499999999999858, -4.330127018922194537, 2.499999999999995559 ) ) ;
#8267 = CARTESIAN_POINT ( 'NONE',  ( 5.803125000614517859, 4.541064518000418104, -2.621784821874998173 ) ) ;
#8268 = CARTESIAN_POINT ( 'NONE',  ( 10.23750000000000071, -2.886751345948130876, 4.999999999999996447 ) ) ;
#8269 = CARTESIAN_POINT ( 'NONE',  ( 11.77500000000000036, 6.123233995736764310E-16, -4.999999999999998224 ) ) ;
#8270 = CARTESIAN_POINT ( 'NONE',  ( 29.40937500061451360, -5.492252693125287522, -1.008910452111647106E-15 ) ) ;
#8271 = CARTESIAN_POINT ( 'NONE',  ( 4.243569643749999010, 14.66562500061451857, 27.54997392385601174 ) ) ;
#8272 = CARTESIAN_POINT ( 'NONE',  ( 26.99062500061451431, 6.054752690667223547, 3.707466751127219781E-16 ) ) ;
#8273 = CARTESIAN_POINT ( 'NONE',  ( 9.337500000000000355, -2.886751345948129988, 4.999999999999997335 ) ) ;
#8274 = CARTESIAN_POINT ( 'NONE',  ( -7.967954043666661671E-16, 17.47812499938548214, 34.33755215474603517 ) ) ;
#8275 = CARTESIAN_POINT ( 'NONE',  ( 23.82187500061451502, 3.027376345333613106, -5.243569643749998122 ) ) ;
#8276 = CARTESIAN_POINT ( 'NONE',  ( 21.59062500061451928, 6.054752690667223547, 3.707466751127219781E-16 ) ) ;
#8277 = CARTESIAN_POINT ( 'NONE',  ( -2.121784821874999949, 15.22812500061459318, -33.67503911421598417 ) ) ;
#8278 = CARTESIAN_POINT ( 'NONE',  ( 23.47500000122903430, -5.773502691896255534, -1.060575238724906372E-15 ) ) ;
#8279 = CARTESIAN_POINT ( 'NONE',  ( 6.853125000614516793, 0.000000000000000000, 5.243569643749999010 ) ) ;
#8280 = CARTESIAN_POINT ( 'NONE',  ( 26.48437500061451644, 5.824947211148865298E-16, -4.756430356249998326 ) ) ;
#8281 = CARTESIAN_POINT ( 'NONE',  ( 23.54062500061451502, -3.027376345333614438, 5.243569643749998122 ) ) ;
#8282 = CARTESIAN_POINT ( 'NONE',  ( 10.09687500061451715, -2.746126346562646425, 4.756430356249996549 ) ) ;
#8283 = CARTESIAN_POINT ( 'NONE',  ( -1.878215178125001827, 16.54062499938548569, 33.25316411605952283 ) ) ;
#8284 = CARTESIAN_POINT ( 'NONE',  ( 16.09687500061452070, -3.027376345333610441, -5.243569643749999898 ) ) ;
#8285 = CARTESIAN_POINT ( 'NONE',  ( 24.90937500061451715, 0.000000000000000000, 5.243569643749999010 ) ) ;
#8286 = CARTESIAN_POINT ( 'NONE',  ( -4.243569643749998122, 14.04687500061451999, 32.45002607614398471 ) ) ;
#8287 = CARTESIAN_POINT ( 'NONE',  ( 5.503125000614516260, 0.000000000000000000, 5.243569643749999010 ) ) ;
#8288 = CARTESIAN_POINT ( 'NONE',  ( 28.26562500061451289, 3.027376345333613106, -5.243569643749998122 ) ) ;
#8289 = CARTESIAN_POINT ( 'NONE',  ( 29.61562500061451431, 3.027376345333613106, -5.243569643749998122 ) ) ;
#8290 = DIRECTION ( 'NONE',  ( -1.000000000000000000, -0.000000000000000000, -0.000000000000000000 ) ) ;
#8291 = CARTESIAN_POINT ( 'NONE',  ( 1.009598436472904703, 9.950840295117078682, -35.91779160164027473 ) ) ;
#8292 = CARTESIAN_POINT ( 'NONE',  ( 3.403125000614518836, -4.541064518000417216, -2.621784821875001281 ) ) ;
#8293 = CARTESIAN_POINT ( 'NONE',  ( 6.984375000614516438, -4.541064518000419881, 2.621784821874995952 ) ) ;
#8294 = PRESENTATION_STYLE_ASSIGNMENT (( #58884 ) ) ;
#8295 = CARTESIAN_POINT ( 'NONE',  ( 16.35000000122903430, -2.886751345948125991, -5.000000000000000000 ) ) ;
#8296 = CARTESIAN_POINT ( 'NONE',  ( 4.096875000614518925, 6.054752690667223547, 3.707466751127219781E-16 ) ) ;
#8297 = CARTESIAN_POINT ( 'NONE',  ( 5.165625000614518569, -6.054752690667223547, -1.112240025338166033E-15 ) ) ;
#8298 = CARTESIAN_POINT ( 'NONE',  ( -4.000000000000000888, 13.15624999877096535, 32.30940107675850470 ) ) ;
#8299 = CARTESIAN_POINT ( 'NONE',  ( 21.91875000122902861, 2.886751345948126879, 4.999999999999999112 ) ) ;
#8300 = CARTESIAN_POINT ( 'NONE',  ( 13.99687500061451928, 6.054752690667223547, 3.707466751127219781E-16 ) ) ;
#8301 = CARTESIAN_POINT ( 'NONE',  ( -3.999999999999999112, 10.51250000000000107, 27.69059892324149885 ) ) ;
#8302 = VERTEX_POINT ( 'NONE', #18703 ) ;
#8303 = CARTESIAN_POINT ( 'NONE',  ( 23.20312500061451644, -4.541064518000417216, -2.621784821875001281 ) ) ;
#8304 = CARTESIAN_POINT ( 'NONE',  ( 7.753125000614518036, 0.000000000000000000, 5.243569643749999010 ) ) ;
#8305 = CARTESIAN_POINT ( 'NONE',  ( 23.48437500061451644, 4.541064518000418104, 2.621784821874999949 ) ) ;
#8306 = CARTESIAN_POINT ( 'NONE',  ( 8.615625000614517859, 3.027376345333611329, 5.243569643749999010 ) ) ;
#8307 = CARTESIAN_POINT ( 'NONE',  ( 10.27500000122903323, 2.886751345948126879, 4.999999999999999112 ) ) ;
#8308 =( BOUNDED_CURVE ( )  B_SPLINE_CURVE ( 2, ( #19130, #69411, #25420, #64207, #19497, #42055, #59024, #47963, #4370 ),
 .UNSPECIFIED., .F., .F. ) 
 B_SPLINE_CURVE_WITH_KNOTS ( ( 3, 2, 2, 2, 3 ),
 ( 0.09722222222222222376, 0.1018518518518518462, 0.1111111111111111049, 0.1203703703703703637, 0.1250000000000000000 ),
 .UNSPECIFIED. ) 
 CURVE ( )  GEOMETRIC_REPRESENTATION_ITEM ( )  RATIONAL_B_SPLINE_CURVE ( ( 0.9330127018922192983, 0.9330127018922194093, 1.000000000000000000, 0.8660254037844387076, 1.000000000000000000, 0.8660254037844387076, 1.000000000000000000, 0.9330127018922191873, 0.9330127018922192983 ) ) 
 REPRESENTATION_ITEM ( '' )  );
#8309 = CARTESIAN_POINT ( 'NONE',  ( 25.52812500061451573, 6.421520780324663323E-16, -5.243569643749999010 ) ) ;
#8310 = EDGE_CURVE ( 'NONE', #50518, #31702, #36444, .T. ) ;
#8311 = CARTESIAN_POINT ( 'NONE',  ( -4.243569643749999898, 10.80312500061451786, -30.00000000000000000 ) ) ;
#8312 = CARTESIAN_POINT ( 'NONE',  ( 10.57500000122903572, 2.886751345948129099, -4.999999999999998224 ) ) ;
#8313 = CARTESIAN_POINT ( 'NONE',  ( 22.67812500061451431, -4.541064518000419881, 2.621784821874995952 ) ) ;
#8314 = CARTESIAN_POINT ( 'NONE',  ( 17.87812500061451715, 6.421520780324663323E-16, -5.243569643749999010 ) ) ;
#8315 = CARTESIAN_POINT ( 'NONE',  ( 27.90937500061451715, 4.119189519843966529, -2.378215178124998275 ) ) ;
#8316 = CARTESIAN_POINT ( 'NONE',  ( 19.34999999999999787, -4.330127018922190985, -2.500000000000001332 ) ) ;
#8317 = CARTESIAN_POINT ( 'NONE',  ( 14.47500000122903430, -5.773502691896255534, -1.060575238724906372E-15 ) ) ;
#8318 = CARTESIAN_POINT ( 'NONE',  ( 10.41562500061451679, 3.027376345333611329, 5.243569643749999010 ) ) ;
#8319 = CARTESIAN_POINT ( 'NONE',  ( 12.89062500061451821, -3.027376345333610441, -5.243569643749999898 ) ) ;
#8320 = CARTESIAN_POINT ( 'NONE',  ( 22.57500000122903572, -5.773502691896255534, -1.060575238724906372E-15 ) ) ;
#8321 = CARTESIAN_POINT ( 'NONE',  ( 20.70937500061451786, 4.541064518000418104, -2.621784821874998173 ) ) ;
#8322 = CARTESIAN_POINT ( 'NONE',  ( 20.70937500061451786, 4.541064518000418104, -2.621784821874998173 ) ) ;
#8323 = CARTESIAN_POINT ( 'NONE',  ( 7.537500001229033408, 4.330127018922191873, 2.499999999999999556 ) ) ;
#8324 = CARTESIAN_POINT ( 'NONE',  ( 7.171875000614517326, 3.027376345333613106, -5.243569643749998122 ) ) ;
#8325 = CARTESIAN_POINT ( 'NONE',  ( 22.84687500061451715, -3.027376345333610441, -5.243569643749999898 ) ) ;
#8326 = CARTESIAN_POINT ( 'NONE',  ( 4.271383450090062261, -2.599258264455263312, -4.416836559537284046 ) ) ;
#8327 = CARTESIAN_POINT ( 'NONE',  ( 20.57812500061451644, 6.421520780324663323E-16, -5.243569643749999010 ) ) ;
#8328 = CARTESIAN_POINT ( 'NONE',  ( 25.39687500061451431, -3.027376345333614438, 5.243569643749998122 ) ) ;
#8329 = CARTESIAN_POINT ( 'NONE',  ( -3.756430356250000102, 18.37812499938548427, 30.00000000000000000 ) ) ;
#8330 = CARTESIAN_POINT ( 'NONE',  ( 3.421875000614516882, -6.054752690667223547, -1.112240025338166033E-15 ) ) ;
#8331 = CARTESIAN_POINT ( 'NONE',  ( 2.000000000000001332, 15.65000000000000036, 33.46410161513774995 ) ) ;
#8332 = CARTESIAN_POINT ( 'NONE',  ( 5.259375000614518569, -4.541064518000417216, -2.621784821875001281 ) ) ;
#8333 = CARTESIAN_POINT ( 'NONE',  ( 17.35312500061451502, -4.541064518000417216, -2.621784821875001281 ) ) ;
#8334 = ORIENTED_EDGE ( 'NONE', *, *, #63321, .T. ) ;
#8335 = DIRECTION ( 'NONE',  ( -0.000000000000000000, -1.000000000000000000, -0.000000000000000000 ) ) ;
#8336 = CARTESIAN_POINT ( 'NONE',  ( 25.97812500061451502, 6.421520780324663323E-16, -5.243569643749999010 ) ) ;
#8337 = CARTESIAN_POINT ( 'NONE',  ( 3.721875000614518036, 3.027376345333611329, 5.243569643749999010 ) ) ;
#8338 = CARTESIAN_POINT ( 'NONE',  ( 10.12500000122903288, 2.886751345948129099, -4.999999999999997335 ) ) ;
#8339 = CARTESIAN_POINT ( 'NONE',  ( 8.625000000000000000, 6.123233995736764310E-16, -4.999999999999998224 ) ) ;
#8340 = CARTESIAN_POINT ( 'NONE',  ( 15.59999999999999964, 0.000000000000000000, 4.999999999999998224 ) ) ;
#8341 = CARTESIAN_POINT ( 'NONE',  ( 19.79062500061451502, 6.054752690667223547, 3.707466751127219781E-16 ) ) ;
#8342 = VERTEX_POINT ( 'NONE', #58958 ) ;
#8343 = CARTESIAN_POINT ( 'NONE',  ( 23.66250000000000142, 2.886751345948126879, 4.999999999999999112 ) ) ;
#8344 = CARTESIAN_POINT ( 'NONE',  ( 26.89687500061451431, -3.027376345333610441, -5.243569643749999898 ) ) ;
#8345 = ORIENTED_EDGE ( 'NONE', *, *, #32039, .F. ) ;
#8346 = CARTESIAN_POINT ( 'NONE',  ( 9.525000000000002132, 6.123233995736764310E-16, -4.999999999999998224 ) ) ;
#8347 = CARTESIAN_POINT ( 'NONE',  ( 14.16562500061451679, -6.054752690667223547, -1.112240025338166033E-15 ) ) ;
#8348 = CARTESIAN_POINT ( 'NONE',  ( 3.328125000614516438, -4.541064518000419881, 2.621784821874995952 ) ) ;
#8349 = CARTESIAN_POINT ( 'NONE',  ( 17.25937500061451502, -5.492252693125287522, -1.008910452111647106E-15 ) ) ;
#8350 = CARTESIAN_POINT ( 'NONE',  ( 28.34062500061451928, 6.054752690667223547, 3.707466751127219781E-16 ) ) ;
#8351 = CARTESIAN_POINT ( 'NONE',  ( 12.60000000122903430, -2.886751345948129988, 4.999999999999997335 ) ) ;
#8352 = CARTESIAN_POINT ( 'NONE',  ( 18.67500000000000071, 4.330127018922191873, 2.499999999999999556 ) ) ;
#8353 = CARTESIAN_POINT ( 'NONE',  ( 27.48749999999999716, -2.886751345948125991, -5.000000000000000000 ) ) ;
#8354 = CARTESIAN_POINT ( 'NONE',  ( 45.00000000000000000, 9.000000000000000000, 0.000000000000000000 ) ) ;
#8355 = CARTESIAN_POINT ( 'NONE',  ( 8.109375000614518214, 4.541064518000418104, -2.621784821874998173 ) ) ;
#8356 = CARTESIAN_POINT ( 'NONE',  ( 18.42187500061451644, 3.027376345333613106, -5.243569643749998122 ) ) ;
#8357 = CARTESIAN_POINT ( 'NONE',  ( 26.09999999999999787, -4.330127018922190985, -2.500000000000001332 ) ) ;
#8358 = ORIENTED_EDGE ( 'NONE', *, *, #44624, .F. ) ;
#8359 = CARTESIAN_POINT ( 'NONE',  ( 28.41562500061451502, 3.027376345333611329, 5.243569643749999010 ) ) ;
#8360 = CARTESIAN_POINT ( 'NONE',  ( 4.275000000000001243, 4.330127018922191873, 2.499999999999999556 ) ) ;
#8361 = CARTESIAN_POINT ( 'NONE',  ( 4.434375000614519280, 6.421520780324663323E-16, -5.243569643749999010 ) ) ;
#8362 = CARTESIAN_POINT ( 'NONE',  ( 16.53750000000000142, -2.886751345948129988, 4.999999999999997335 ) ) ;
#8363 = CARTESIAN_POINT ( 'NONE',  ( 13.52812500061451750, 4.541064518000418104, 2.621784821874999949 ) ) ;
#8364 = CARTESIAN_POINT ( 'NONE',  ( 25.89375000122903003, 5.773502691896255534, 3.535250795749688401E-16 ) ) ;
#8365 = CARTESIAN_POINT ( 'NONE',  ( 9.581250001229033586, 6.123233995736764310E-16, -4.999999999999998224 ) ) ;
#8366 = CYLINDRICAL_SURFACE ( 'NONE', #15060, 4.000000000000000000 ) ;
#8367 = CARTESIAN_POINT ( 'NONE',  ( 17.70000000122903216, -2.886751345948125991, -5.000000000000000000 ) ) ;
#8368 = CARTESIAN_POINT ( 'NONE',  ( 0.000000000000000000, 20.00000000000000000, -30.00000000000000000 ) ) ;
#8369 = CARTESIAN_POINT ( 'NONE',  ( 16.54687500061451644, -2.746126346562642428, -4.756430356249999214 ) ) ;
#8370 = CARTESIAN_POINT ( 'NONE',  ( 7.040625000614517681, -3.027376345333610441, -5.243569643749999898 ) ) ;
#8371 = CARTESIAN_POINT ( 'NONE',  ( 24.87187500061451573, 3.027376345333611329, 5.243569643749999010 ) ) ;
#8372 = CARTESIAN_POINT ( 'NONE',  ( 19.65000000122902790, 5.773502691896255534, 3.535250795749688401E-16 ) ) ;
#8373 = CARTESIAN_POINT ( 'NONE',  ( 24.04687500061451644, -3.027376345333614438, 5.243569643749998122 ) ) ;
#8374 = CARTESIAN_POINT ( 'NONE',  ( 5.812500000000001776, -5.773502691896255534, -1.060575238724906372E-15 ) ) ;
#8375 = CARTESIAN_POINT ( 'NONE',  ( 4.000000000000000000, 10.85000000122903430, 32.30940107675849049 ) ) ;
#8376 = CARTESIAN_POINT ( 'NONE',  ( 15.66562500061451857, 3.027376345333613106, -5.243569643749998122 ) ) ;
#8377 = CARTESIAN_POINT ( 'NONE',  ( 3.787500001229033408, 6.123233995736764310E-16, -4.999999999999998224 ) ) ;
#8378 = CARTESIAN_POINT ( 'NONE',  ( 10.43437500061451750, 4.541064518000418104, 2.621784821874999949 ) ) ;
#8379 = CARTESIAN_POINT ( 'NONE',  ( 3.046343057529203424, 3.964819538874875704, 3.046343057529141696 ) ) ;
#8380 = VERTEX_POINT ( 'NONE', #63425 ) ;
#8381 = CARTESIAN_POINT ( 'NONE',  ( 12.14062500061451821, 6.054752690667223547, 3.707466751127219781E-16 ) ) ;
#8382 = CARTESIAN_POINT ( 'NONE',  ( 13.98750000000000071, -2.886751345948237457, -4.999999999999807265 ) ) ;
#8383 = CARTESIAN_POINT ( 'NONE',  ( 25.08750000122903145, 4.330127018922191873, 2.499999999999999556 ) ) ;
#8384 = CARTESIAN_POINT ( 'NONE',  ( 9.796875000614519990, -3.027376345333610441, -5.243569643749999898 ) ) ;
#8385 = CARTESIAN_POINT ( 'NONE',  ( 11.20312500061451644, 4.541064518000418104, -2.621784821874998173 ) ) ;
#8386 = ADVANCED_FACE ( 'NONE', ( #19066 ), #8366, .F. ) ;
#8387 = CARTESIAN_POINT ( 'NONE',  ( 27.73125000122902861, 4.330127018922191873, 2.499999999999999556 ) ) ;
#8388 = CARTESIAN_POINT ( 'NONE',  ( 24.98437500061451644, -4.541064518000419881, 2.621784821874995952 ) ) ;
#8389 = CARTESIAN_POINT ( 'NONE',  ( 4.312500001229034652, 4.330127018922192761, -2.499999999999997780 ) ) ;
#8390 = DIRECTION ( 'NONE',  ( -1.000000000000000000, -0.000000000000000000, -0.000000000000000000 ) ) ;
#8391 = CARTESIAN_POINT ( 'NONE',  ( -2.121784821874999949, 14.38437500061451679, -33.67503911421598417 ) ) ;
#8392 = AXIS2_PLACEMENT_3D ( 'NONE', #32888, #72781, #50257 ) ;
#8393 = CARTESIAN_POINT ( 'NONE',  ( 16.32187500061451502, 3.027376345333611329, 5.243569643749999010 ) ) ;
#8394 = CARTESIAN_POINT ( 'NONE',  ( 18.63750000122903216, 6.123233995736764310E-16, -4.999999999999998224 ) ) ;
#8395 = CARTESIAN_POINT ( 'NONE',  ( 11.63437500061451857, 6.421520780324663323E-16, -5.243569643749999010 ) ) ;
#8396 = CARTESIAN_POINT ( 'NONE',  ( -4.243569643749999898, 18.86562500061451431, -32.45002607614398471 ) ) ;
#8397 = CARTESIAN_POINT ( 'NONE',  ( 20.25000000122903288, -2.886751345948129988, 4.999999999999997335 ) ) ;
#8398 = CARTESIAN_POINT ( 'NONE',  ( 12.44062500061451537, -3.027376345333610441, -5.243569643749999898 ) ) ;
#8399 = VERTEX_POINT ( 'NONE', #40912 ) ;
#8400 = CARTESIAN_POINT ( 'NONE',  ( 16.12500000000000000, -4.330127018922194537, 2.499999999999995559 ) ) ;
#8401 = CARTESIAN_POINT ( 'NONE',  ( 29.09999999999999787, 0.000000000000000000, 4.999999999999998224 ) ) ;
#8402 = CARTESIAN_POINT ( 'NONE',  ( 11.37187500061451928, 3.027376345333611329, 5.243569643749999010 ) ) ;
#8403 = CARTESIAN_POINT ( 'NONE',  ( -3.305248395036964552E-15, 5.000000000000034639, 25.99999999999995737 ) ) ;
#8404 = CARTESIAN_POINT ( 'NONE',  ( 13.53750000122903430, -4.330127018922194537, 2.499999999999995559 ) ) ;
#8405 = CARTESIAN_POINT ( 'NONE',  ( 21.67500000122903359, -5.773502691896255534, -1.060575238724906372E-15 ) ) ;
#8406 = CARTESIAN_POINT ( 'NONE',  ( 18.81562500061452070, 3.027376345333613106, -5.243569643749998122 ) ) ;
#8407 = CARTESIAN_POINT ( 'NONE',  ( 21.44062500061452070, -3.027376345333610441, -5.243569643749999898 ) ) ;
#8408 = CARTESIAN_POINT ( 'NONE',  ( 28.16250000122903074, 4.330127018922192761, -2.499999999999997780 ) ) ;
#8409 = CARTESIAN_POINT ( 'NONE',  ( 25.83749999999999858, 5.773502691896255534, 3.535250795749688894E-16 ) ) ;
#8410 = CARTESIAN_POINT ( 'NONE',  ( 7.584375000614516082, 5.824947211148865298E-16, -4.756430356249998326 ) ) ;
#8411 = CARTESIAN_POINT ( 'NONE',  ( 28.39687500061452141, 6.054752690667223547, 3.707466751127219781E-16 ) ) ;
#8412 = CARTESIAN_POINT ( 'NONE',  ( -2.000000000000000000, 9.687500001229034652, -33.46410161513775705 ) ) ;
#8413 = CARTESIAN_POINT ( 'NONE',  ( 4.243569643749999010, 13.37187500061451750, -32.45002607614398471 ) ) ;
#8414 = CARTESIAN_POINT ( 'NONE',  ( 4.687500001229034652, 6.123233995736764310E-16, -4.999999999999998224 ) ) ;
#8415 = CARTESIAN_POINT ( 'NONE',  ( 5.325000000000000178, -4.330127018922194537, 2.499999999999995559 ) ) ;
#8416 = CARTESIAN_POINT ( 'NONE',  ( 11.88749999999999929, 5.773502691896255534, 3.535250795749688401E-16 ) ) ;
#8417 = CARTESIAN_POINT ( 'NONE',  ( 7.359375000614516438, 0.000000000000000000, 5.243569643749999010 ) ) ;
#8418 = CARTESIAN_POINT ( 'NONE',  ( 28.34062500061451928, 6.054752690667223547, 3.707466751127219781E-16 ) ) ;
#8419 = DIRECTION ( 'NONE',  ( -1.000000000000000000, -0.000000000000000000, -0.000000000000000000 ) ) ;
#8420 = CARTESIAN_POINT ( 'NONE',  ( 1.071796769724489895, 10.52990381179670010, 26.00000000000000355 ) ) ;
#8421 = CARTESIAN_POINT ( 'NONE',  ( 6.159375000614517148, -4.541064518000417216, -2.621784821875001281 ) ) ;
#8422 = CARTESIAN_POINT ( 'NONE',  ( 10.20937500061451786, -4.541064518000417216, -2.621784821875001281 ) ) ;
#8423 = CARTESIAN_POINT ( 'NONE',  ( 4.125000000000000000, 6.123233995736764310E-16, -4.999999999999998224 ) ) ;
#8424 = CARTESIAN_POINT ( 'NONE',  ( 4.243569643749999898, 13.72812500061459495, 30.00000000000000000 ) ) ;
#8425 = CARTESIAN_POINT ( 'NONE',  ( 3.012598849231780118, 25.23371056053735728, 27.35582546009486649 ) ) ;
#8426 = CARTESIAN_POINT ( 'NONE',  ( 7.500000000000000000, 0.000000000000000000, 4.999999999999998224 ) ) ;
#8427 = ADVANCED_FACE ( 'NONE', ( #64142 ), #41623, .T. ) ;
#8428 = CARTESIAN_POINT ( 'NONE',  ( 15.49687500061451573, -4.119189519843965641, -2.378215178125001383 ) ) ;
#8429 = CARTESIAN_POINT ( 'NONE',  ( 20.42812500061451431, -4.541064518000419881, 2.621784821874995952 ) ) ;
#8430 = CARTESIAN_POINT ( 'NONE',  ( 10.34062500061451750, 6.054752690667223547, 3.707466751127219781E-16 ) ) ;
#8431 = CARTESIAN_POINT ( 'NONE',  ( 22.65937500061451360, -5.492252693125287522, -1.008910452111647106E-15 ) ) ;
#8432 = CARTESIAN_POINT ( 'NONE',  ( 10.62187500061451928, -6.054752690667223547, -1.112240025338166033E-15 ) ) ;
#8433 = CARTESIAN_POINT ( 'NONE',  ( 25.98750000000000071, -2.886751345948129988, 4.999999999999997335 ) ) ;
#8434 = CARTESIAN_POINT ( 'NONE',  ( 19.50000000122903288, -2.886751345948125991, -5.000000000000000000 ) ) ;
#8435 = CARTESIAN_POINT ( 'NONE',  ( 27.70312500061451289, -4.541064518000417216, -2.621784821875001281 ) ) ;
#8436 = DIRECTION ( 'NONE',  ( -0.000000000000000000, -1.000000000000000000, -0.000000000000000000 ) ) ;
#8437 = CARTESIAN_POINT ( 'NONE',  ( 10.35937500061451644, 4.541064518000418104, -2.621784821874998173 ) ) ;
#8438 = CARTESIAN_POINT ( 'NONE',  ( 14.18437500061451750, -4.541064518000419881, 2.621784821874995952 ) ) ;
#8439 = CARTESIAN_POINT ( 'NONE',  ( 26.70937500061451431, 0.000000000000000000, 5.243569643749999010 ) ) ;
#8440 = EDGE_CURVE ( 'NONE', #24521, #8998, #53806, .T. ) ;
#8441 = CARTESIAN_POINT ( 'NONE',  ( 4.265625000614517326, -6.054752690667223547, -1.112240025338166033E-15 ) ) ;
#8442 = CYLINDRICAL_SURFACE ( 'NONE', #6568, 4.999999999999998224 ) ;
#8443 = CARTESIAN_POINT ( 'NONE',  ( 19.02187500061451786, 3.027376345333611329, 5.243569643749999010 ) ) ;
#8444 = CARTESIAN_POINT ( 'NONE',  ( 10.73437500061451644, 6.421520780324663323E-16, -5.243569643749999010 ) ) ;
#8445 = CARTESIAN_POINT ( 'NONE',  ( -3.756430356249999214, 13.27812499938548463, 27.83122392262697531 ) ) ;
#8446 = CARTESIAN_POINT ( 'NONE',  ( 22.34999999999999787, 0.000000000000000000, 4.999999999999998224 ) ) ;
#8447 = CARTESIAN_POINT ( 'NONE',  ( -4.000000000000000000, 14.97499999999999964, 30.00000000000000000 ) ) ;
#8448 = CARTESIAN_POINT ( 'NONE',  ( -4.243569643749999898, 12.62187500061451928, -32.45002607614398471 ) ) ;
#8449 = CARTESIAN_POINT ( 'NONE',  ( 23.89687500061451786, 5.492252693125287522, 3.363034840372157021E-16 ) ) ;
#8450 = CARTESIAN_POINT ( 'NONE',  ( 14.76562500061451821, 3.027376345333613106, -5.243569643749998122 ) ) ;
#8451 = CARTESIAN_POINT ( 'NONE',  ( 3.450000000000001510, 0.000000000000000000, 4.999999999999998224 ) ) ;
#8452 =( BOUNDED_CURVE ( )  B_SPLINE_CURVE ( 2, ( #20644, #30001, #60166, #9576, #32108, #52544, #54641, #41108, #4046 ),
 .UNSPECIFIED., .F., .F. ) 
 B_SPLINE_CURVE_WITH_KNOTS ( ( 3, 2, 2, 2, 3 ),
 ( 0.7083333333333333703, 0.7129629629629629095, 0.7222222222222222099, 0.7314814814814815103, 0.7361111111111111605 ),
 .UNSPECIFIED. ) 
 CURVE ( )  GEOMETRIC_REPRESENTATION_ITEM ( )  RATIONAL_B_SPLINE_CURVE ( ( 0.9330127018922192983, 0.9330127018922200755, 1.000000000000000000, 0.8660254037844387076, 1.000000000000000000, 0.8660254037844387076, 1.000000000000000000, 0.9330127018922185211, 0.9330127018922192983 ) ) 
 REPRESENTATION_ITEM ( '' )  );
#8453 = EDGE_CURVE ( 'NONE', #31017, #60322, #45423, .T. ) ;
#8454 = CARTESIAN_POINT ( 'NONE',  ( 25.57499999999999929, -4.330127018922194537, 2.499999999999995559 ) ) ;
#8455 = CARTESIAN_POINT ( 'NONE',  ( 13.12500000000000178, 6.123233995736764310E-16, -4.999999999999998224 ) ) ;
#8456 = CARTESIAN_POINT ( 'NONE',  ( -2.000000000000000000, 16.88750000122903572, 26.53589838486224650 ) ) ;
#8457 = CARTESIAN_POINT ( 'NONE',  ( 10.80000000122903536, -2.886751345948129988, 4.999999999999997335 ) ) ;
#8458 = CARTESIAN_POINT ( 'NONE',  ( 23.67187500061451999, -6.054752690667223547, -1.112240025338166033E-15 ) ) ;
#8459 = CARTESIAN_POINT ( 'NONE',  ( 16.99687500061451573, -3.027376345333610441, -5.243569643749999898 ) ) ;
#8460 = DIRECTION ( 'NONE',  ( -1.000000000000000000, -0.000000000000000000, -0.000000000000000000 ) ) ;
#8461 = VERTEX_POINT ( 'NONE', #42357 ) ;
#8462 = CARTESIAN_POINT ( 'NONE',  ( 20.76562500061451644, 3.027376345333611329, 5.243569643749999010 ) ) ;
#8463 = CARTESIAN_POINT ( 'NONE',  ( 4.678125000614516971, -4.541064518000419881, 2.621784821874995952 ) ) ;
#8464 = CARTESIAN_POINT ( 'NONE',  ( 17.25937500061451502, 0.000000000000000000, 5.243569643749999010 ) ) ;
#8465 = CARTESIAN_POINT ( 'NONE',  ( 29.29687500061451644, 6.054752690667223547, 3.707466751127219781E-16 ) ) ;
#8466 = CARTESIAN_POINT ( 'NONE',  ( 5.653125000614517504, -4.541064518000417216, -2.621784821875001281 ) ) ;
#8467 = CARTESIAN_POINT ( 'NONE',  ( 19.60312500061451502, -4.541064518000417216, -2.621784821875001281 ) ) ;
#8468 = CARTESIAN_POINT ( 'NONE',  ( 4.243569643749999898, 16.39062500061451999, 32.45002607614398471 ) ) ;
#8469 = CARTESIAN_POINT ( 'NONE',  ( 17.36250000122903359, 4.330127018922192761, -2.499999999999997780 ) ) ;
#8470 = CARTESIAN_POINT ( 'NONE',  ( 12.23437500061451821, 4.119189519843966529, 2.378215178124999607 ) ) ;
#8471 = CARTESIAN_POINT ( 'NONE',  ( 6.028125000614517504, -4.541064518000419881, 2.621784821874995952 ) ) ;
#8472 = CARTESIAN_POINT ( 'NONE',  ( 4.171875000614517326, 3.027376345333611329, 5.243569643749999010 ) ) ;
#8473 = CARTESIAN_POINT ( 'NONE',  ( 3.571875000614517237, 3.027376345333613106, -5.243569643749998122 ) ) ;
#8474 = CARTESIAN_POINT ( 'NONE',  ( 23.48437500061451644, 4.541064518000418104, 2.621784821874999949 ) ) ;
#8475 = CARTESIAN_POINT ( 'NONE',  ( 13.71562500061451750, -6.054752690667223547, -1.112240025338166033E-15 ) ) ;
#8476 = CARTESIAN_POINT ( 'NONE',  ( 25.53750000122903074, 4.330127018922191873, 2.499999999999999556 ) ) ;
#8477 = CARTESIAN_POINT ( 'NONE',  ( 23.84062500061451928, 6.054752690667223547, 3.707466751127219781E-16 ) ) ;
#8478 = CARTESIAN_POINT ( 'NONE',  ( 20.03437500061451715, -4.541064518000419881, 2.621784821874995952 ) ) ;
#8479 = CARTESIAN_POINT ( 'NONE',  ( 13.60312500061451679, 0.000000000000000000, 5.243569643749999010 ) ) ;
#8480 = CARTESIAN_POINT ( 'NONE',  ( 9.001249775931846008E-16, 14.57187500061451679, 34.90005215228797653 ) ) ;
#8481 = CARTESIAN_POINT ( 'NONE',  ( 20.39062500061451644, -3.027376345333614438, 5.243569643749998122 ) ) ;
#8482 = CYLINDRICAL_SURFACE ( 'NONE', #754, 9.000000000000000000 ) ;
#8483 = ORIENTED_EDGE ( 'NONE', *, *, #5952, .T. ) ;
#8484 = ORIENTED_EDGE ( 'NONE', *, *, #70743, .F. ) ;
#8485 = CARTESIAN_POINT ( 'NONE',  ( 23.77499999999999858, -4.330127018922194537, 2.499999999999995559 ) ) ;
#8486 = CARTESIAN_POINT ( 'NONE',  ( -3.999999999999999112, 11.45000000000000107, -30.00000000000000000 ) ) ;
#8487 = CARTESIAN_POINT ( 'NONE',  ( 14.83125000122903359, -4.330127018922194537, 2.499999999999995559 ) ) ;
#8488 = CARTESIAN_POINT ( 'NONE',  ( 26.12812500061451360, 4.541064518000418104, 2.621784821874999949 ) ) ;
#8489 = CARTESIAN_POINT ( 'NONE',  ( 7.715625000614515727, 3.027376345333611329, 5.243569643749999010 ) ) ;
#8490 = CARTESIAN_POINT ( 'NONE',  ( 19.65000000122902790, 5.773502691896255534, 3.535250795749688894E-16 ) ) ;
#8491 = EDGE_CURVE ( 'NONE', #27766, #65361, #23196, .T. ) ;
#8492 = CARTESIAN_POINT ( 'NONE',  ( 25.52812500061451573, 6.421520780324663323E-16, -5.243569643749999010 ) ) ;
#8493 = CARTESIAN_POINT ( 'NONE',  ( 25.12499999999999645, -4.330127018922194537, 2.499999999999995559 ) ) ;
#8494 = CARTESIAN_POINT ( 'NONE',  ( 28.11562500061451431, -6.054752690667223547, -1.112240025338166033E-15 ) ) ;
#8495 = CARTESIAN_POINT ( 'NONE',  ( 8.728125000614518569, -4.541064518000419881, 2.621784821874995952 ) ) ;
#8496 = EDGE_LOOP ( 'NONE', ( #61068, #1007, #39447, #48879 ) ) ;
#8497 = AXIS2_PLACEMENT_3D ( 'NONE', #42292, #41925, #14572 ) ;
#8498 = CARTESIAN_POINT ( 'NONE',  ( 23.61562500061451431, -6.054752690667223547, -1.112240025338166033E-15 ) ) ;
#8499 = CARTESIAN_POINT ( 'NONE',  ( 4.378125000614518925, 6.421520780324663323E-16, -5.243569643749999010 ) ) ;
#8500 = PRODUCT_DEFINITION_CONTEXT ( 'detailed design', #62028, 'design' ) ;
#8501 = CARTESIAN_POINT ( 'NONE',  ( 13.43437500061451750, 5.824947211148865298E-16, -4.756430356249998326 ) ) ;
#8502 = CARTESIAN_POINT ( 'NONE',  ( 3.665625000614517681, 3.027376345333611329, 5.243569643749999010 ) ) ;
#8503 = CARTESIAN_POINT ( 'NONE',  ( 4.243569643749999898, 19.59687500061452070, -27.54997392385601529 ) ) ;
#8504 =( BOUNDED_CURVE ( )  B_SPLINE_CURVE ( 2, ( #12020, #62980, #58512, #62625, #57792, #34543, #12376, #23817, #41193 ),
 .UNSPECIFIED., .F., .F. ) 
 B_SPLINE_CURVE_WITH_KNOTS ( ( 3, 2, 2, 2, 3 ),
 ( 0.1630434782608695676, 0.1666666666666666574, 0.1739130434782608647, 0.1811594202898550721, 0.1847826086956521896 ),
 .UNSPECIFIED. ) 
 CURVE ( )  GEOMETRIC_REPRESENTATION_ITEM ( )  RATIONAL_B_SPLINE_CURVE ( ( 0.9330127018922194093, 0.9330127018922196314, 1.000000000000000000, 0.8660254037844387076, 1.000000000000000000, 0.8660254037844387076, 1.000000000000000000, 0.9330127018922190762, 0.9330127018922194093 ) ) 
 REPRESENTATION_ITEM ( '' )  );
#8505 = CARTESIAN_POINT ( 'NONE',  ( 11.96250000000000213, 2.886751345948126879, 4.999999999999999112 ) ) ;
#8506 = CARTESIAN_POINT ( 'NONE',  ( 13.84687500061451537, -3.027376345333610441, -5.243569643749999898 ) ) ;
#8507 = CARTESIAN_POINT ( 'NONE',  ( 8.550000001229031810, -2.886751345948129988, 4.999999999999997335 ) ) ;
#8508 = CARTESIAN_POINT ( 'NONE',  ( 15.19687500061451857, -3.027376345333610441, -5.243569643749999898 ) ) ;
#8509 = CARTESIAN_POINT ( 'NONE',  ( 15.86250000000000249, 2.886751345948129099, -4.999999999999998224 ) ) ;
#8510 = CARTESIAN_POINT ( 'NONE',  ( 9.459375000614517859, 4.541064518000418104, -2.621784821874998173 ) ) ;
#8511 = CARTESIAN_POINT ( 'NONE',  ( 4.243569643749999898, 11.92812500061451608, -30.00000000000000000 ) ) ;
#8512 = CYLINDRICAL_SURFACE ( 'NONE', #25320, 4.999999999999998224 ) ;
#8513 = CARTESIAN_POINT ( 'NONE',  ( 13.62187500061451750, 3.027376345333611329, 5.243569643749999010 ) ) ;
#8514 = CARTESIAN_POINT ( 'NONE',  ( 15.71250000000000036, -5.773502691896255534, -1.060575238724906372E-15 ) ) ;
#8515 = CARTESIAN_POINT ( 'NONE',  ( 22.56562500061451715, 3.027376345333611329, 5.243569643749999010 ) ) ;
#8516 = CARTESIAN_POINT ( 'NONE',  ( -0.7368805616696195715, 9.859898480082234684, 25.82089837893477480 ) ) ;
#8517 = CARTESIAN_POINT ( 'NONE',  ( 11.32500000000000107, 6.123233995736764310E-16, -4.999999999999998224 ) ) ;
#8518 = CARTESIAN_POINT ( 'NONE',  ( 25.92187500061451999, -6.054752690667223547, -1.112240025338166033E-15 ) ) ;
#8519 = CARTESIAN_POINT ( 'NONE',  ( 28.28437500061451715, 6.421520780324663323E-16, -5.243569643749999010 ) ) ;
#8520 =( BOUNDED_CURVE ( )  B_SPLINE_CURVE ( 2, ( #58576, #59301, #25708, #2807, #70769, #20145, #71136 ),
 .UNSPECIFIED., .F., .F. ) 
 B_SPLINE_CURVE_WITH_KNOTS ( ( 3, 2, 2, 3 ),
 ( 0.5999999999999999778, 0.6027777777777777457, 0.6055555555555555136, 0.6083333333333332815 ),
 .UNSPECIFIED. ) 
 CURVE ( )  GEOMETRIC_REPRESENTATION_ITEM ( )  RATIONAL_B_SPLINE_CURVE ( ( 1.000000000000000000, 0.8660254037844387076, 1.000000000000000000, 0.8660254037844387076, 1.000000000000000000, 0.8660254037844387076, 1.000000000000000000 ) ) 
 REPRESENTATION_ITEM ( '' )  );
#8521 = CARTESIAN_POINT ( 'NONE',  ( 4.303125000614516971, -4.541064518000417216, -2.621784821875001281 ) ) ;
#8522 = CARTESIAN_POINT ( 'NONE',  ( 23.18437500061451217, -2.746126346562642428, -4.756430356249999214 ) ) ;
#8523 = CARTESIAN_POINT ( 'NONE',  ( 17.48437500061451999, 6.421520780324663323E-16, -5.243569643749999010 ) ) ;
#8524 = CARTESIAN_POINT ( 'NONE',  ( 8.634375000614515017, -2.746126346562646425, 4.756430356249996549 ) ) ;
#8525 = CARTESIAN_POINT ( 'NONE',  ( 2.953125000614516438, -4.541064518000417216, -2.621784821875001281 ) ) ;
#8526 = CARTESIAN_POINT ( 'NONE',  ( 5.484375000614518214, 4.541064518000418104, 2.621784821874999949 ) ) ;
#8527 = CARTESIAN_POINT ( 'NONE',  ( 16.24687500061451573, 6.054752690667223547, 3.707466751127219781E-16 ) ) ;
#8528 = CARTESIAN_POINT ( 'NONE',  ( 9.881250001229032520, -4.330127018922194537, 2.499999999999995559 ) ) ;
#8529 = CARTESIAN_POINT ( 'NONE',  ( 27.56250000000000000, 2.886751345948129099, -4.999999999999998224 ) ) ;
#8530 = CARTESIAN_POINT ( 'NONE',  ( 26.52187500061451431, 3.027376345333613106, -5.243569643749998122 ) ) ;
#8531 = CARTESIAN_POINT ( 'NONE',  ( 3.756430356250000546, 13.69062499938548250, 27.83122392262697886 ) ) ;
#8532 = CARTESIAN_POINT ( 'NONE',  ( 21.82499999999999574, 4.330127018922191873, 2.499999999999999556 ) ) ;
#8533 = VERTEX_POINT ( 'NONE', #58597 ) ;
#8534 = CARTESIAN_POINT ( 'NONE',  ( 7.050000000000000711, 0.000000000000000000, 4.999999999999998224 ) ) ;
#8535 = CARTESIAN_POINT ( 'NONE',  ( 8.184375000614515727, -2.746126346562646425, 4.756430356249996549 ) ) ;
#8536 = CARTESIAN_POINT ( 'NONE',  ( 22.60312500061451857, 0.000000000000000000, 5.243569643749999010 ) ) ;
#8537 = CARTESIAN_POINT ( 'NONE',  ( 12.90000000000000213, 0.000000000000000000, 4.999999999999998224 ) ) ;
#8538 = EDGE_CURVE ( 'NONE', #40887, #30395, #30752, .T. ) ;
#8539 = CARTESIAN_POINT ( 'NONE',  ( 9.075000001229033941, -5.773502691896255534, -1.060575238724906372E-15 ) ) ;
#8540 = CARTESIAN_POINT ( 'NONE',  ( 6.140625000614516438, -3.027376345333610441, -5.243569643749999898 ) ) ;
#8541 = CARTESIAN_POINT ( 'NONE',  ( 21.71249999999999858, 2.886751345948129099, -4.999999999999998224 ) ) ;
#8542 = CARTESIAN_POINT ( 'NONE',  ( 19.49062500061451431, -3.027376345333614438, 5.243569643749998122 ) ) ;
#8543 = CARTESIAN_POINT ( 'NONE',  ( 23.47499999999999787, 6.123233995736764310E-16, -4.999999999999998224 ) ) ;
#8544 = CARTESIAN_POINT ( 'NONE',  ( 25.98750000122903003, 4.330127018922191873, 2.499999999999999556 ) ) ;
#8545 = CARTESIAN_POINT ( 'NONE',  ( -7.967954043666661671E-16, 18.37812499938548427, 34.33755215474603517 ) ) ;
#8546 =( BOUNDED_CURVE ( )  B_SPLINE_CURVE ( 2, ( #14109, #37747, #48478, #65453, #71746, #65825, #36648 ),
 .UNSPECIFIED., .F., .F. ) 
 B_SPLINE_CURVE_WITH_KNOTS ( ( 3, 2, 2, 3 ),
 ( 0.4000000000000000777, 0.4033333333333333215, 0.4066666666666666763, 0.4099999999999999201 ),
 .UNSPECIFIED. ) 
 CURVE ( )  GEOMETRIC_REPRESENTATION_ITEM ( )  RATIONAL_B_SPLINE_CURVE ( ( 0.9999999999999977796, 0.8660254037844409281, 1.000000000000000000, 0.8660254037844387076, 1.000000000000000000, 0.8660254037844409281, 0.9999999999999977796 ) ) 
 REPRESENTATION_ITEM ( '' )  );
#8547 = CARTESIAN_POINT ( 'NONE',  ( 4.724999999999999645, 4.330127018922191873, 2.499999999999999556 ) ) ;
#8548 = ORIENTED_EDGE ( 'NONE', *, *, #17032, .T. ) ;
#8549 = CARTESIAN_POINT ( 'NONE',  ( 20.54062500061451502, -3.027376345333610441, -5.243569643749999898 ) ) ;
#8550 = CARTESIAN_POINT ( 'NONE',  ( 26.54062500061451146, 6.054752690667223547, 3.707466751127219781E-16 ) ) ;
#8551 = CARTESIAN_POINT ( 'NONE',  ( 25.05937500061451573, -4.541064518000417216, -2.621784821875001281 ) ) ;
#8552 = CARTESIAN_POINT ( 'NONE',  ( 9.750000000000001776, 0.000000000000000000, 4.999999999999998224 ) ) ;
#8553 = CARTESIAN_POINT ( 'NONE',  ( 12.55312500061451786, 4.541064518000418104, -2.621784821874998173 ) ) ;
#8554 = CARTESIAN_POINT ( 'NONE',  ( 27.96562500061451928, 3.027376345333611329, 5.243569643749999010 ) ) ;
#8555 = CARTESIAN_POINT ( 'NONE',  ( 9.553125000614517859, 0.000000000000000000, 5.243569643749999010 ) ) ;
#8556 = FACE_OUTER_BOUND ( 'NONE', #20970, .T. ) ;
#8557 = CARTESIAN_POINT ( 'NONE',  ( -3.000416591977282496E-16, 11.64687500061451786, 25.09994784771203058 ) ) ;
#8558 = CARTESIAN_POINT ( 'NONE',  ( 24.71250000122903145, 0.000000000000000000, 4.999999999999998224 ) ) ;
#8559 = CARTESIAN_POINT ( 'NONE',  ( 18.68437500061451928, -4.119189519843968306, 2.378215178124996054 ) ) ;
#8560 = CARTESIAN_POINT ( 'NONE',  ( 13.37812500061451715, 6.421520780324663323E-16, -5.243569643749999010 ) ) ;
#8561 = CARTESIAN_POINT ( 'NONE',  ( 10.80937500061451928, 4.541064518000418104, -2.621784821874998173 ) ) ;
#8562 = CARTESIAN_POINT ( 'NONE',  ( 8.671875000614518214, 3.027376345333611329, 5.243569643749999010 ) ) ;
#8563 = CARTESIAN_POINT ( 'NONE',  ( 16.84687500061451715, -3.027376345333614438, 5.243569643749998122 ) ) ;
#8564 = EDGE_LOOP ( 'NONE', ( #5921, #66714, #29257, #61200 ) ) ;
#8565 = CARTESIAN_POINT ( 'NONE',  ( -1.585543809737898213, 9.875380255848558164, 35.79011327352668559 ) ) ;
#8566 = CARTESIAN_POINT ( 'NONE',  ( 22.07812500061451644, 4.541064518000418104, 2.621784821874999949 ) ) ;
#8567 = CARTESIAN_POINT ( 'NONE',  ( 16.47187500061452070, -6.054752690667223547, -1.112240025338166033E-15 ) ) ;
#8568 = CARTESIAN_POINT ( 'NONE',  ( 23.09062500061451573, -3.027376345333614438, 5.243569643749998122 ) ) ;
#8569 = CARTESIAN_POINT ( 'NONE',  ( -1.999999999999997113, 12.87500000000000178, 33.46410161513775705 ) ) ;
#8570 = CARTESIAN_POINT ( 'NONE',  ( 27.70312500061451289, -4.541064518000417216, -2.621784821875001281 ) ) ;
#8571 = CARTESIAN_POINT ( 'NONE',  ( 6.825000001229034829, -5.773502691896255534, -1.060575238724906372E-15 ) ) ;
#8572 = ORIENTED_EDGE ( 'NONE', *, *, #34302, .F. ) ;
#8573 = CARTESIAN_POINT ( 'NONE',  ( 4.612500001229032698, -4.330127018922190985, -2.500000000000001332 ) ) ;
#8574 = CARTESIAN_POINT ( 'NONE',  ( 3.999999999999998668, 16.66249999999999787, -32.30940107675850470 ) ) ;
#8575 = CARTESIAN_POINT ( 'NONE',  ( 25.87500000122903288, 2.886751345948129099, -4.999999999999998224 ) ) ;
#8576 = CARTESIAN_POINT ( 'NONE',  ( -1.878215178124999163, 14.70312499938548356, 26.74683588394047007 ) ) ;
#8577 = CARTESIAN_POINT ( 'NONE',  ( 7.996875000614519280, -3.027376345333610441, -5.243569643749999898 ) ) ;
#8578 = CARTESIAN_POINT ( 'NONE',  ( 4.322286709174337105, 2.513530903668243610, -4.417718143658825980 ) ) ;
#8579 = CARTESIAN_POINT ( 'NONE',  ( 15.85312500061451857, 0.000000000000000000, 5.243569643749999010 ) ) ;
#8580 = CARTESIAN_POINT ( 'NONE',  ( 9.459375000614517859, 4.541064518000418104, -2.621784821874998173 ) ) ;
#8581 = CARTESIAN_POINT ( 'NONE',  ( 27.90000000122903145, -2.886751345948129988, 4.999999999999997335 ) ) ;
#8582 = CARTESIAN_POINT ( 'NONE',  ( 17.10937500061451999, 4.541064518000418104, -2.621784821874998173 ) ) ;
#8583 = CARTESIAN_POINT ( 'NONE',  ( 5.334375000614517859, 6.421520780324663323E-16, -5.243569643749999010 ) ) ;
#8584 = CARTESIAN_POINT ( 'NONE',  ( 2.393811435568372112E-14, 18.68750000000000355, 34.00000000000000000 ) ) ;
#8585 = CARTESIAN_POINT ( 'NONE',  ( 5.765625000614519102, 3.027376345333613106, -5.243569643749998122 ) ) ;
#8586 = CARTESIAN_POINT ( 'NONE',  ( 15.96562500061451573, -6.054752690667223547, -1.112240025338166033E-15 ) ) ;
#8587 = ORIENTED_EDGE ( 'NONE', *, *, #54635, .F. ) ;
#8588 = CARTESIAN_POINT ( 'NONE',  ( 13.19062500061451537, -3.027376345333614438, 5.243569643749998122 ) ) ;
#8589 = CARTESIAN_POINT ( 'NONE',  ( 5.100000001229034297, -2.886751345948125991, -5.000000000000000000 ) ) ;
#8590 = CARTESIAN_POINT ( 'NONE',  ( 9.778125000614517504, 6.421520780324663323E-16, -5.243569643749999010 ) ) ;
#8591 = CARTESIAN_POINT ( 'NONE',  ( 22.02187500061452141, 2.746126346562645981, -4.756430356249997438 ) ) ;
#8592 = CARTESIAN_POINT ( 'NONE',  ( 11.58750000000000036, -2.886751345948129988, 4.999999999999997335 ) ) ;
#8593 = ADVANCED_FACE ( 'NONE', ( #1747 ), #36076, .F. ) ;
#8594 = CARTESIAN_POINT ( 'NONE',  ( 6.675000001229034474, 2.886751345948126879, 4.999999999999999112 ) ) ;
#8595 = CARTESIAN_POINT ( 'NONE',  ( 19.87500000000000000, 6.123233995736764310E-16, -4.999999999999998224 ) ) ;
#8596 = CARTESIAN_POINT ( 'NONE',  ( 14.25937500061451679, -4.541064518000417216, -2.621784821875001281 ) ) ;
#8597 = CARTESIAN_POINT ( 'NONE',  ( 15.37500000122903465, -5.773502691896255534, -1.060575238724906372E-15 ) ) ;
#8598 = CARTESIAN_POINT ( 'NONE',  ( 23.36250000000000071, -5.773502691896255534, -1.060575238724906372E-15 ) ) ;
#8599 = CARTESIAN_POINT ( 'NONE',  ( 4.243569643749999898, 18.67812500061451431, -30.00000000000000000 ) ) ;
#8600 = CARTESIAN_POINT ( 'NONE',  ( 3.236215399915419511, 3.811430163627435252, 3.601125184156294345 ) ) ;
#8601 = CARTESIAN_POINT ( 'NONE',  ( 45.00000000000000000, 0.000000000000000000, 4.999999999999998224 ) ) ;
#8602 = CARTESIAN_POINT ( 'NONE',  ( 34.99999999999999289, -2.499999999999999556, -3.499999999999999556 ) ) ;
#8603 = CARTESIAN_POINT ( 'NONE',  ( 3.481582908954544919, -3.588718827790031263, 3.545339672739869830 ) ) ;
#8604 = CARTESIAN_POINT ( 'NONE',  ( 3.921087004242067131, -3.102464839086551240, -4.227284519891857606 ) ) ;
#8605 = CARTESIAN_POINT ( 'NONE',  ( 15.57187500061451679, -6.054752690667223547, -1.112240025338166033E-15 ) ) ;
#8606 = CARTESIAN_POINT ( 'NONE',  ( 29.66249999999999432, -5.773502691896255534, -1.060575238724906372E-15 ) ) ;
#8607 = CARTESIAN_POINT ( 'NONE',  ( 12.70312500061451821, 0.000000000000000000, 5.243569643749999010 ) ) ;
#8608 = CARTESIAN_POINT ( 'NONE',  ( 7.518750001229031810, 2.886751345948126879, 4.999999999999999112 ) ) ;
#8609 = CARTESIAN_POINT ( 'NONE',  ( 23.97187500061451360, 3.027376345333611329, 5.243569643749999010 ) ) ;
#8610 = CARTESIAN_POINT ( 'NONE',  ( 14.82187500061451502, 4.119189519843966529, 2.378215178124999607 ) ) ;
#8611 = CARTESIAN_POINT ( 'NONE',  ( 9.703125000614514661, -4.541064518000417216, -2.621784821875001281 ) ) ;
#8612 = CARTESIAN_POINT ( 'NONE',  ( 12.12187500061451573, 3.027376345333613106, -5.243569643749998122 ) ) ;
#8613 = ORIENTED_EDGE ( 'NONE', *, *, #11628, .T. ) ;
#8614 = CARTESIAN_POINT ( 'NONE',  ( 23.97187500061451360, 3.027376345333611329, 5.243569643749999010 ) ) ;
#8615 = CARTESIAN_POINT ( 'NONE',  ( 24.81562500061451715, 3.027376345333611329, 5.243569643749999010 ) ) ;
#8616 = CARTESIAN_POINT ( 'NONE',  ( 28.26562500061451289, 3.027376345333613106, -5.243569643749998122 ) ) ;
#8617 = CARTESIAN_POINT ( 'NONE',  ( 4.882324679417408220, 1.079004970772768246, -5.131482293177458409 ) ) ;
#8618 = CARTESIAN_POINT ( 'NONE',  ( 8.287499999999999645, 5.773502691896255534, 3.535250795749688894E-16 ) ) ;
#8619 = CARTESIAN_POINT ( 'NONE',  ( 16.61250000122903359, 0.000000000000000000, 4.999999999999998224 ) ) ;
#8620 = CARTESIAN_POINT ( 'NONE',  ( 18.75000000000000000, 0.000000000000000000, 4.999999999999998224 ) ) ;
#8621 = CARTESIAN_POINT ( 'NONE',  ( 8.521875000614517859, 4.119189519843966529, 2.378215178124999607 ) ) ;
#8622 = VERTEX_POINT ( 'NONE', #47529 ) ;
#8623 = CARTESIAN_POINT ( 'NONE',  ( 16.08749999999999503, -2.886751345948129988, 4.999999999999997335 ) ) ;
#8624 = CARTESIAN_POINT ( 'NONE',  ( 18.86249999999999716, -5.773502691896255534, -1.060575238724906372E-15 ) ) ;
#8625 = CARTESIAN_POINT ( 'NONE',  ( 13.07812500061451821, 4.541064518000418104, 2.621784821874999949 ) ) ;
#8626 = VERTEX_POINT ( 'NONE', #31264 ) ;
#8627 = CARTESIAN_POINT ( 'NONE',  ( 1.626862140677534273E-15, 16.17500000122903359, -26.00000000000000355 ) ) ;
#8628 = CARTESIAN_POINT ( 'NONE',  ( 4.243569643749999898, 16.48437500061451644, -30.00000000000000000 ) ) ;
#8629 = CARTESIAN_POINT ( 'NONE',  ( 5.203125000614518214, -4.541064518000417216, -2.621784821875001281 ) ) ;
#8630 = CARTESIAN_POINT ( 'NONE',  ( 19.81875000122903430, -5.773502691896255534, -1.060575238724906372E-15 ) ) ;
#8631 = CARTESIAN_POINT ( 'NONE',  ( 13.46249999999999858, -5.773502691896255534, -1.060575238724906372E-15 ) ) ;
#8632 = CARTESIAN_POINT ( 'NONE',  ( 28.39687500061451431, 0.000000000000000000, 4.756430356249998326 ) ) ;
#8633 = VERTEX_POINT ( 'NONE', #68982 ) ;
#8634 = CARTESIAN_POINT ( 'NONE',  ( 9.001249775931846008E-16, 14.96562500061451750, 34.90005215228797653 ) ) ;
#8635 = CARTESIAN_POINT ( 'NONE',  ( 26.46562500061451573, 3.027376345333613106, -5.243569643749998122 ) ) ;
#8636 = CARTESIAN_POINT ( 'NONE',  ( 9.375000000000001776, -4.330127018922194537, 2.499999999999995559 ) ) ;
#8637 = CARTESIAN_POINT ( 'NONE',  ( -1.878215178125001827, 16.54062499938548569, 33.25316411605952283 ) ) ;
#8638 = CARTESIAN_POINT ( 'NONE',  ( 23.37187500061451573, 3.027376345333613106, -5.243569643749998122 ) ) ;
#8639 = CARTESIAN_POINT ( 'NONE',  ( 18.17812500061451786, -4.541064518000419881, 2.621784821874995952 ) ) ;
#8640 = CARTESIAN_POINT ( 'NONE',  ( -4.243569643749998122, 13.99062500061459602, -27.54997392385601174 ) ) ;
#8641 = CARTESIAN_POINT ( 'NONE',  ( 23.58750000122903145, 6.123233995736764310E-16, -4.999999999999998224 ) ) ;
#8642 = CARTESIAN_POINT ( 'NONE',  ( 6.253125000614517148, 4.541064518000418104, -2.621784821874998173 ) ) ;
#8643 = CARTESIAN_POINT ( 'NONE',  ( 26.97187500061451004, 2.746126346562645981, -4.756430356249997438 ) ) ;
#8644 = CARTESIAN_POINT ( 'NONE',  ( 22.04062500061451502, 6.054752690667223547, 3.707466751127219781E-16 ) ) ;
#8645 = CARTESIAN_POINT ( 'NONE',  ( 10.24687500061451750, -2.746126346562642428, -4.756430356249999214 ) ) ;
#8646 = CARTESIAN_POINT ( 'NONE',  ( -1.878215178125001827, 16.09062499938548285, 33.25316411605952283 ) ) ;
#8647 = CARTESIAN_POINT ( 'NONE',  ( 16.65937500061452070, 4.541064518000418104, -2.621784821874998173 ) ) ;
#8648 = CARTESIAN_POINT ( 'NONE',  ( 16.24687500061451573, 6.054752690667223547, 3.707466751127219781E-16 ) ) ;
#8649 = CARTESIAN_POINT ( 'NONE',  ( 24.57187500061451502, -6.054752690667223547, -1.112240025338166033E-15 ) ) ;
#8650 = CARTESIAN_POINT ( 'NONE',  ( -4.243569643749999898, 14.42187500061451999, 27.54997392385601529 ) ) ;
#8651 = CARTESIAN_POINT ( 'NONE',  ( 5.578125000614518214, -4.541064518000419881, 2.621784821874995952 ) ) ;
#8652 = CARTESIAN_POINT ( 'NONE',  ( 28.71562500061451573, 3.027376345333613106, -5.243569643749998122 ) ) ;
#8653 = CARTESIAN_POINT ( 'NONE',  ( 29.69062500061451715, 6.054752690667223547, 3.707466751127219781E-16 ) ) ;
#8654 = CARTESIAN_POINT ( 'NONE',  ( 4.648177544792955741E-15, 13.73749999999999716, 33.99999999999999289 ) ) ;
#8655 = CARTESIAN_POINT ( 'NONE',  ( 1.970565482296603443, 9.811066920826823079, -35.68093638750369223 ) ) ;
#8656 = CARTESIAN_POINT ( 'NONE',  ( 3.703125000614516882, 0.000000000000000000, 5.243569643749999010 ) ) ;
#8657 = CARTESIAN_POINT ( 'NONE',  ( 6.721875000614518925, 3.027376345333613106, -5.243569643749998122 ) ) ;
#8658 = CARTESIAN_POINT ( 'NONE',  ( 13.95000000122903572, -2.886751345948129988, 4.999999999999997335 ) ) ;
#8659 = CARTESIAN_POINT ( 'NONE',  ( 4.359375000614517326, -4.541064518000417216, -2.621784821875001281 ) ) ;
#8660 = CARTESIAN_POINT ( 'NONE',  ( 10.65000000122903323, 5.773502691896255534, 3.535250795749688894E-16 ) ) ;
#8661 = CARTESIAN_POINT ( 'NONE',  ( 3.965625000614515727, 3.027376345333613106, -5.243569643749998122 ) ) ;
#8662 = CARTESIAN_POINT ( 'NONE',  ( 3.999999999999998668, 13.75624999877096677, 32.30940107675850470 ) ) ;
#8663 = CARTESIAN_POINT ( 'NONE',  ( 20.19375000122903430, -2.886751345948129988, 4.999999999999997335 ) ) ;
#8664 = CARTESIAN_POINT ( 'NONE',  ( 13.69687500061451679, -3.027376345333614438, 5.243569643749998122 ) ) ;
#8665 = CARTESIAN_POINT ( 'NONE',  ( 7.650000000000000355, -4.330127018922190985, -2.500000000000001332 ) ) ;
#8666 = ORIENTED_EDGE ( 'NONE', *, *, #61233, .F. ) ;
#8667 = CARTESIAN_POINT ( 'NONE',  ( 23.24062500061451786, -3.027376345333610441, -5.243569643749999898 ) ) ;
#8668 = CARTESIAN_POINT ( 'NONE',  ( 7.565625000614518036, 3.027376345333613106, -5.243569643749998122 ) ) ;
#8669 = CARTESIAN_POINT ( 'NONE',  ( 25.43437500061451573, -4.541064518000419881, 2.621784821874995952 ) ) ;
#8670 = CARTESIAN_POINT ( 'NONE',  ( 7.378125000614518036, -4.541064518000419881, 2.621784821874995952 ) ) ;
#8671 = DIRECTION ( 'NONE',  ( -1.000000000000000000, -0.000000000000000000, -0.000000000000000000 ) ) ;
#8672 = CARTESIAN_POINT ( 'NONE',  ( 9.187500001229034652, 6.123233995736764310E-16, -4.999999999999998224 ) ) ;
#8673 = CARTESIAN_POINT ( 'NONE',  ( 23.95312500061451289, 0.000000000000000000, 5.243569643749999010 ) ) ;
#8674 = CARTESIAN_POINT ( 'NONE',  ( -2.121784821874996840, 11.32812500061451644, -26.32496088578401583 ) ) ;
#8675 = CARTESIAN_POINT ( 'NONE',  ( 9.937500001229032875, -4.330127018922194537, 2.499999999999995559 ) ) ;
#8676 = CARTESIAN_POINT ( 'NONE',  ( 20.35312500061451502, 0.000000000000000000, 5.243569643749999010 ) ) ;
#8677 = CARTESIAN_POINT ( 'NONE',  ( 18.02812500061451573, 4.541064518000418104, 2.621784821874999949 ) ) ;
#8678 = CARTESIAN_POINT ( 'NONE',  ( 27.57187500061451857, 2.746126346562643317, 4.756430356249998326 ) ) ;
#8679 = CARTESIAN_POINT ( 'NONE',  ( 19.27500000000000213, -4.330127018922194537, 2.499999999999995559 ) ) ;
#8680 = CARTESIAN_POINT ( 'NONE',  ( 13.12500000122903288, -5.773502691896255534, -1.060575238724906372E-15 ) ) ;
#8681 = CARTESIAN_POINT ( 'NONE',  ( 9.515625000614518214, 3.027376345333611329, 5.243569643749999010 ) ) ;
#8682 = CARTESIAN_POINT ( 'NONE',  ( 13.41562500061451502, 3.027376345333613106, -5.243569643749998122 ) ) ;
#8683 = CARTESIAN_POINT ( 'NONE',  ( 22.53750000122903430, -4.330127018922194537, 2.499999999999995559 ) ) ;
#8684 = CARTESIAN_POINT ( 'NONE',  ( 21.23437500061451644, 4.541064518000418104, 2.621784821874999949 ) ) ;
#8685 = CARTESIAN_POINT ( 'NONE',  ( 21.27187500061451786, 3.027376345333611329, 5.243569643749999010 ) ) ;
#8686 = CARTESIAN_POINT ( 'NONE',  ( 2.393811435568372112E-14, 18.68750000000000355, 34.00000000000000000 ) ) ;
#8687 = CARTESIAN_POINT ( 'NONE',  ( 8.662500001229034297, -4.330127018922190985, -2.500000000000001332 ) ) ;
#8688 = CARTESIAN_POINT ( 'NONE',  ( 6.684375000614518392, 6.421520780324663323E-16, -5.243569643749999010 ) ) ;
#8689 = CARTESIAN_POINT ( 'NONE',  ( 23.10937500061451644, 0.000000000000000000, 5.243569643749999010 ) ) ;
#8690 = CARTESIAN_POINT ( 'NONE',  ( 4.715814460642238970, -1.662339852463772916, 4.911777014959029408 ) ) ;
#8691 = EDGE_CURVE ( 'NONE', #55926, #41736, #19804, .T. ) ;
#8692 = CARTESIAN_POINT ( 'NONE',  ( 19.22812500061451502, 6.421520780324663323E-16, -5.243569643749999010 ) ) ;
#8693 = CARTESIAN_POINT ( 'NONE',  ( 24.00937500061451502, 0.000000000000000000, 5.243569643749999010 ) ) ;
#8694 = CARTESIAN_POINT ( 'NONE',  ( 3.756430356249998770, 20.36562499938548143, 32.16877607737301759 ) ) ;
#8695 = CARTESIAN_POINT ( 'NONE',  ( 4.898587196589407898E-16, 12.50000000000000000, 34.00000000000000000 ) ) ;
#8696 = CARTESIAN_POINT ( 'NONE',  ( 16.36875000122903145, 2.886751345948129099, -4.999999999999997335 ) ) ;
#8697 = CARTESIAN_POINT ( 'NONE',  ( 6.384375000614516793, 4.541064518000418104, 2.621784821874999949 ) ) ;
#8698 = CARTESIAN_POINT ( 'NONE',  ( 17.20312500061451644, 0.000000000000000000, 5.243569643749999010 ) ) ;
#8699 = ORIENTED_EDGE ( 'NONE', *, *, #16481, .T. ) ;
#8700 = CARTESIAN_POINT ( 'NONE',  ( 22.80000000000000071, 0.000000000000000000, 4.999999999999998224 ) ) ;
#8701 = CARTESIAN_POINT ( 'NONE',  ( 24.44062500061451715, -3.027376345333614438, 5.243569643749998122 ) ) ;
#8702 = CARTESIAN_POINT ( 'NONE',  ( 2.000000000000001332, 17.00000000000000000, 33.46410161513774995 ) ) ;
#8703 = CARTESIAN_POINT ( 'NONE',  ( 30.00000000000000000, 1.224646799147353059E-15, -9.999999999999998224 ) ) ;
#8704 = CARTESIAN_POINT ( 'NONE',  ( 15.37500000000000000, 6.123233995736764310E-16, -4.999999999999998224 ) ) ;
#8705 = CARTESIAN_POINT ( 'NONE',  ( 27.33750000122903145, 4.330127018922191873, 2.499999999999999556 ) ) ;
#8706 = CARTESIAN_POINT ( 'NONE',  ( 21.44062500061452070, -3.027376345333610441, -5.243569643749999898 ) ) ;
#8707 = ORIENTED_EDGE ( 'NONE', *, *, #13371, .T. ) ;
#8708 = CARTESIAN_POINT ( 'NONE',  ( 22.23750000000000071, 5.773502691896255534, 3.535250795749688894E-16 ) ) ;
#8709 = CARTESIAN_POINT ( 'NONE',  ( 23.63437500061451502, -4.541064518000419881, 2.621784821874995952 ) ) ;
#8710 = ADVANCED_FACE ( 'NONE', ( #19431 ), #8004, .T. ) ;
#8711 = ORIENTED_EDGE ( 'NONE', *, *, #64551, .T. ) ;
#8712 = DIRECTION ( 'NONE',  ( -1.000000000000000000, 0.000000000000000000, 0.000000000000000000 ) ) ;
#8713 = CARTESIAN_POINT ( 'NONE',  ( 13.90312500061451750, 4.541064518000418104, -2.621784821874998173 ) ) ;
#8714 = CARTESIAN_POINT ( 'NONE',  ( 3.440625000614518036, -3.027376345333610441, -5.243569643749999898 ) ) ;
#8715 = CARTESIAN_POINT ( 'NONE',  ( 16.43437500061451573, -2.746126346562642428, -4.756430356249999214 ) ) ;
#8716 = CARTESIAN_POINT ( 'NONE',  ( 26.27812500061451573, -4.541064518000419881, 2.621784821874995952 ) ) ;
#8717 = CARTESIAN_POINT ( 'NONE',  ( 13.01250000122903394, 0.000000000000000000, 4.999999999999998224 ) ) ;
#8718 = CARTESIAN_POINT ( 'NONE',  ( 20.58750000000000213, -2.886751345948129988, 4.999999999999997335 ) ) ;
#8719 = CARTESIAN_POINT ( 'NONE',  ( 25.91250000000000142, 2.886751345948126879, 4.999999999999999112 ) ) ;
#8720 = CARTESIAN_POINT ( 'NONE',  ( 6.121875000614517504, -6.054752690667223547, -1.112240025338166033E-15 ) ) ;
#8721 = CARTESIAN_POINT ( 'NONE',  ( 16.24687500061451573, 6.054752690667223547, 3.707466751127219781E-16 ) ) ;
#8722 = VERTEX_POINT ( 'NONE', #26460 ) ;
#8723 = CARTESIAN_POINT ( 'NONE',  ( 29.20312500061451644, 4.541064518000418104, -2.621784821874998173 ) ) ;
#8724 = CARTESIAN_POINT ( 'NONE',  ( 26.74687500061451573, -3.027376345333614438, 5.243569643749998122 ) ) ;
#8725 = CARTESIAN_POINT ( 'NONE',  ( -2.498395430326213790E-14, 18.91249999999999787, 26.00000000000000000 ) ) ;
#8726 = CARTESIAN_POINT ( 'NONE',  ( 15.11249999999999893, 2.886751345948126879, 4.999999999999999112 ) ) ;
#8727 = CARTESIAN_POINT ( 'NONE',  ( 12.51562500061451821, 3.027376345333613106, -5.243569643749998122 ) ) ;
#8728 = CARTESIAN_POINT ( 'NONE',  ( 16.35000000000000142, 4.330127018922192761, -2.499999999999997780 ) ) ;
#8729 = LINE ( 'NONE', #47528, #64291 ) ;
#8730 = CARTESIAN_POINT ( 'NONE',  ( 26.92499999999999716, -4.330127018922194537, 2.499999999999995559 ) ) ;
#8731 = CARTESIAN_POINT ( 'NONE',  ( 19.16250000122903430, 4.330127018922192761, -2.499999999999997780 ) ) ;
#8732 = CARTESIAN_POINT ( 'NONE',  ( 15.18750000122903465, 4.330127018922191873, 2.499999999999999556 ) ) ;
#8733 = CARTESIAN_POINT ( 'NONE',  ( 17.74687500061451928, -2.746126346562646425, 4.756430356249996549 ) ) ;
#8734 = CARTESIAN_POINT ( 'NONE',  ( 8.765625000614518214, -6.054752690667223547, -1.112240025338166033E-15 ) ) ;
#8735 = CARTESIAN_POINT ( 'NONE',  ( 25.39687500061451431, -3.027376345333614438, 5.243569643749998122 ) ) ;
#8736 = EDGE_CURVE ( 'NONE', #44903, #53469, #38308, .T. ) ;
#8737 = CARTESIAN_POINT ( 'NONE',  ( -2.121784821874996840, 17.23437500061451999, 33.67503911421598417 ) ) ;
#8738 = CARTESIAN_POINT ( 'NONE',  ( 24.87187500061451573, 3.027376345333611329, 5.243569643749999010 ) ) ;
#8739 = CARTESIAN_POINT ( 'NONE',  ( 5.362500000000003375, -5.773502691896255534, -1.060575238724906372E-15 ) ) ;
#8740 = CARTESIAN_POINT ( 'NONE',  ( -2.828200636599751609E-16, 11.90000000122903501, 25.38119784648299770 ) ) ;
#8741 = CARTESIAN_POINT ( 'NONE',  ( 12.89062500061451821, -3.027376345333610441, -5.243569643749999898 ) ) ;
#8743 =( BOUNDED_CURVE ( )  B_SPLINE_CURVE ( 2, ( #53138, #37974, #36878, #9175, #30972, #43164, #47600 ),
 .UNSPECIFIED., .F., .F. ) 
 B_SPLINE_CURVE_WITH_KNOTS ( ( 3, 2, 2, 3 ),
 ( 0.2600000000000000644, 0.2633333333333333637, 0.2666666666666667185, 0.2700000000000000733 ),
 .UNSPECIFIED. ) 
 CURVE ( )  GEOMETRIC_REPRESENTATION_ITEM ( )  RATIONAL_B_SPLINE_CURVE ( ( 0.9999999999999977796, 0.8660254037844409281, 1.000000000000000000, 0.8660254037844387076, 1.000000000000000000, 0.8660254037844364872, 1.000000000000002220 ) ) 
 REPRESENTATION_ITEM ( '' )  );
#8742 = CARTESIAN_POINT ( 'NONE',  ( 3.412500001229032964, 4.330127018922192761, -2.499999999999997780 ) ) ;
#8744 = CARTESIAN_POINT ( 'NONE',  ( 9.121875000614517504, 3.027376345333611329, 5.243569643749999010 ) ) ;
#8745 = CARTESIAN_POINT ( 'NONE',  ( -3.182292052831503071, 3.860956188314065507, -27.56400650891052351 ) ) ;
#8746 = ORIENTED_EDGE ( 'NONE', *, *, #30487, .F. ) ;
#8747 = CARTESIAN_POINT ( 'NONE',  ( 10.71562500061451928, 3.027376345333613106, -5.243569643749998122 ) ) ;
#8748 = CARTESIAN_POINT ( 'NONE',  ( 13.62187500061451750, 3.027376345333611329, 5.243569643749999010 ) ) ;
#8749 = CARTESIAN_POINT ( 'NONE',  ( 4.000000000000000000, 19.68124999877096570, 27.69059892324149885 ) ) ;
#8750 = CARTESIAN_POINT ( 'NONE',  ( 20.92500000122903714, 2.886751345948129099, -4.999999999999998224 ) ) ;
#8751 = CARTESIAN_POINT ( 'NONE',  ( 11.18437500061451928, 6.421520780324663323E-16, -5.243569643749999010 ) ) ;
#8752 = CARTESIAN_POINT ( 'NONE',  ( 13.22812500061451502, -4.541064518000419881, 2.621784821874995952 ) ) ;
#8753 = CARTESIAN_POINT ( 'NONE',  ( 28.55625000122903145, 4.330127018922192761, -2.499999999999997780 ) ) ;
#8754 = CARTESIAN_POINT ( 'NONE',  ( 20.78437500061451715, 4.541064518000418104, 2.621784821874999949 ) ) ;
#8755 = CARTESIAN_POINT ( 'NONE',  ( 0.000000000000000000, 0.000000000000000000, 50.00000000000000000 ) ) ;
#8756 = CYLINDRICAL_SURFACE ( 'NONE', #72873, 4.999999999999998224 ) ;
#8757 = CARTESIAN_POINT ( 'NONE',  ( 8.362500000000002487, 2.886751345948126879, 4.999999999999998224 ) ) ;
#8758 = CARTESIAN_POINT ( 'NONE',  ( 2.121784821874999061, 15.20937500061451786, -33.67503911421598417 ) ) ;
#8759 = CARTESIAN_POINT ( 'NONE',  ( 16.73437500061451644, 4.541064518000418104, 2.621784821874999949 ) ) ;
#8760 = CARTESIAN_POINT ( 'NONE',  ( 15.30000000122903359, -2.886751345948129988, 4.999999999999997335 ) ) ;
#8761 = CARTESIAN_POINT ( 'NONE',  ( 11.07187500061451679, -6.054752690667223547, -1.112240025338166033E-15 ) ) ;
#8762 = CARTESIAN_POINT ( 'NONE',  ( 4.243569643749999898, 17.32812500061451644, -30.00000000000000000 ) ) ;
#8763 = CARTESIAN_POINT ( 'NONE',  ( 17.58750000122903145, -4.330127018922194537, 2.499999999999995559 ) ) ;
#8764 = CARTESIAN_POINT ( 'NONE',  ( 11.57812500061451644, 6.421520780324663323E-16, -5.243569643749999010 ) ) ;
#8765 = VECTOR ( 'NONE', #61298, 1000.000000000000000 ) ;
#8766 = ORIENTED_EDGE ( 'NONE', *, *, #19281, .T. ) ;
#8767 = CARTESIAN_POINT ( 'NONE',  ( 16.83749999999999858, 5.773502691896255534, 3.535250795749688894E-16 ) ) ;
#8768 = CARTESIAN_POINT ( 'NONE',  ( 29.25000000000000000, -4.330127018922190985, -2.500000000000001332 ) ) ;
#8769 = CARTESIAN_POINT ( 'NONE',  ( 9.346875000614517148, -3.027376345333610441, -5.243569643749999898 ) ) ;
#8770 = CARTESIAN_POINT ( 'NONE',  ( 4.043974773626141328, 2.940596785297640459, 4.204683744944501811 ) ) ;
#8771 = CARTESIAN_POINT ( 'NONE',  ( 12.11250000122903181, 0.000000000000000000, 4.999999999999998224 ) ) ;
#8772 = CARTESIAN_POINT ( 'NONE',  ( 21.33750000122903145, 6.123233995736764310E-16, -4.999999999999998224 ) ) ;
#8773 = CARTESIAN_POINT ( 'NONE',  ( 17.20312500061451644, 0.000000000000000000, 5.243569643749999010 ) ) ;
#8774 = CARTESIAN_POINT ( 'NONE',  ( 19.71562500061451928, 3.027376345333613106, -5.243569643749998122 ) ) ;
#8775 = CARTESIAN_POINT ( 'NONE',  ( 26.85000000122903430, 5.773502691896255534, 3.535250795749688894E-16 ) ) ;
#8776 = CARTESIAN_POINT ( 'NONE',  ( 24.82499999999999929, 6.123233995736764310E-16, -4.999999999999998224 ) ) ;
#8777 = CARTESIAN_POINT ( 'NONE',  ( 9.999999999999992895, -5.857864376269048101, 9.999999999999992895 ) ) ;
#8778 = CARTESIAN_POINT ( 'NONE',  ( 28.38749999999999929, -2.886751345948125991, -5.000000000000000000 ) ) ;
#8779 = CARTESIAN_POINT ( 'NONE',  ( 28.88437500061451502, 4.541064518000418104, 2.621784821874999949 ) ) ;
#8780 = CARTESIAN_POINT ( 'NONE',  ( -2.000000000000000000, 15.87500000000000000, 26.53589838486224650 ) ) ;
#8781 = CARTESIAN_POINT ( 'NONE',  ( 4.243569643749999898, 14.19687500061451857, -27.54997392385601529 ) ) ;
#8782 = CARTESIAN_POINT ( 'NONE',  ( 3.337500001229034563, 6.123233995736764310E-16, -4.999999999999998224 ) ) ;
#8783 = CARTESIAN_POINT ( 'NONE',  ( 3.937500000000000444, -2.886751345948129988, 4.999999999999997335 ) ) ;
#8784 = CARTESIAN_POINT ( 'NONE',  ( 11.84999999999999964, 4.330127018922192761, -2.499999999999997780 ) ) ;
#8785 = CARTESIAN_POINT ( 'NONE',  ( 7.434375000614519280, -4.541064518000419881, 2.621784821874995952 ) ) ;
#8786 = CARTESIAN_POINT ( 'NONE',  ( 25.19062500061451715, 6.054752690667223547, 3.707466751127219781E-16 ) ) ;
#8787 = CARTESIAN_POINT ( 'NONE',  ( 1.999999999999997335, 16.92500000000000071, 33.46410161513775705 ) ) ;
#8788 = CARTESIAN_POINT ( 'NONE',  ( 14.47499999999999964, 6.123233995736764310E-16, -4.999999999999998224 ) ) ;
#8789 = ADVANCED_FACE ( 'NONE', ( #6126 ), #29385, .T. ) ;
#8790 = DIRECTION ( 'NONE',  ( 0.000000000000000000, 0.000000000000000000, -1.000000000000000000 ) ) ;
#8791 = EDGE_CURVE ( 'NONE', #28731, #66075, #26013, .T. ) ;
#8792 = CARTESIAN_POINT ( 'NONE',  ( 5.559375000614517504, 0.000000000000000000, 5.243569643749999010 ) ) ;
#8793 = CARTESIAN_POINT ( 'NONE',  ( 8.746875000614515727, -3.027376345333614438, 5.243569643749998122 ) ) ;
#8794 = CARTESIAN_POINT ( 'NONE',  ( 3.225000000000002309, 6.123233995736764310E-16, -4.999999999999998224 ) ) ;
#8795 = CARTESIAN_POINT ( 'NONE',  ( -4.243569643749998122, 12.19062500061459531, 32.45002607614398471 ) ) ;
#8796 = CARTESIAN_POINT ( 'NONE',  ( 7.320879633048903241E-15, 17.63749999999999218, -34.00000000000000000 ) ) ;
#8797 = CARTESIAN_POINT ( 'NONE',  ( 3.149999999999999911, -4.330127018922190985, -2.500000000000001332 ) ) ;
#8798 = CARTESIAN_POINT ( 'NONE',  ( 14.52187500061451608, -4.119189519843968306, 2.378215178124996054 ) ) ;
#8799 = CARTESIAN_POINT ( 'NONE',  ( 19.90312500061451573, 0.000000000000000000, 5.243569643749999010 ) ) ;
#8800 = CARTESIAN_POINT ( 'NONE',  ( 10.52812500061451750, -4.541064518000419881, 2.621784821874995952 ) ) ;
#8801 = CARTESIAN_POINT ( 'NONE',  ( 23.18437500061451217, -2.746126346562642428, -4.756430356249999214 ) ) ;
#8802 = CARTESIAN_POINT ( 'NONE',  ( 9.196875000614518569, -3.027376345333614438, 5.243569643749998122 ) ) ;
#8803 = CARTESIAN_POINT ( 'NONE',  ( 25.01249999999999929, 2.886751345948126879, 4.999999999999999112 ) ) ;
#8804 = CARTESIAN_POINT ( 'NONE',  ( 19.38750000122903216, -4.330127018922194537, 2.499999999999995559 ) ) ;
#8805 = CARTESIAN_POINT ( 'NONE',  ( 27.21562500061451928, -6.054752690667223547, -1.112240025338166033E-15 ) ) ;
#8806 = CARTESIAN_POINT ( 'NONE',  ( 15.52500000000000036, 4.330127018922191873, 2.499999999999999556 ) ) ;
#8807 = CARTESIAN_POINT ( 'NONE',  ( 9.909375000614517148, 4.541064518000418104, -2.621784821874998173 ) ) ;
#8808 = CARTESIAN_POINT ( 'NONE',  ( 14.48437500061451821, 4.541064518000418104, 2.621784821874999949 ) ) ;
#8809 = CARTESIAN_POINT ( 'NONE',  ( 26.14687500061451431, 6.054752690667223547, 3.707466751127219781E-16 ) ) ;
#8810 = CARTESIAN_POINT ( 'NONE',  ( 23.53125000122902932, 6.123233995736764310E-16, -4.999999999999998224 ) ) ;
#8811 = CARTESIAN_POINT ( 'NONE',  ( 13.68750000000000178, 5.773502691896255534, 3.535250795749688894E-16 ) ) ;
#8812 = CARTESIAN_POINT ( 'NONE',  ( 20.67187500061451289, 3.027376345333613106, -5.243569643749998122 ) ) ;
#8813 = CARTESIAN_POINT ( 'NONE',  ( 11.67187500061451821, 3.027376345333613106, -5.243569643749998122 ) ) ;
#8814 = CARTESIAN_POINT ( 'NONE',  ( 2.655984681222220721E-16, 19.61562499938548143, 25.66244784525396483 ) ) ;
#8815 = CARTESIAN_POINT ( 'NONE',  ( 23.32499999999999929, -4.330127018922194537, 2.499999999999995559 ) ) ;
#8816 = CARTESIAN_POINT ( 'NONE',  ( 1.999999999999997335, 15.57500000000000107, 33.46410161513775705 ) ) ;
#8817 = CARTESIAN_POINT ( 'NONE',  ( 4.243569643749999898, 11.53437500061451892, -30.00000000000000000 ) ) ;
#8818 = CARTESIAN_POINT ( 'NONE',  ( 25.20937500061451431, 4.119189519843966529, -2.378215178124998275 ) ) ;
#8819 = CARTESIAN_POINT ( 'NONE',  ( 15.47812500061451679, -4.541064518000419881, 2.621784821874995952 ) ) ;
#8820 = CARTESIAN_POINT ( 'NONE',  ( 3.937500000000000444, -2.886751345948129988, 4.999999999999997335 ) ) ;
#8821 = CARTESIAN_POINT ( 'NONE',  ( -1.394453263437886604E-15, 19.32500000122903216, -26.00000000000000000 ) ) ;
#8822 = CARTESIAN_POINT ( 'NONE',  ( 30.00000000000000000, 0.000000000000000000, 0.000000000000000000 ) ) ;
#8823 = CARTESIAN_POINT ( 'NONE',  ( 11.92500000000000071, 4.330127018922191873, 2.499999999999999556 ) ) ;
#8824 = CARTESIAN_POINT ( 'NONE',  ( 2.000000000000001332, 18.91250000122903430, 33.46410161513774995 ) ) ;
#8825 = CARTESIAN_POINT ( 'NONE',  ( 10.65000000122903323, 5.773502691896255534, 3.535250795749688894E-16 ) ) ;
#8826 = VECTOR ( 'NONE', #45717, 1000.000000000000000 ) ;
#8827 = CARTESIAN_POINT ( 'NONE',  ( 23.40937500061451715, 4.541064518000418104, -2.621784821874998173 ) ) ;
#8828 = CARTESIAN_POINT ( 'NONE',  ( 15.68437500061451573, 6.421520780324663323E-16, -5.243569643749999010 ) ) ;
#8829 = CARTESIAN_POINT ( 'NONE',  ( 4.898587196589412829E-16, 27.50000000000000000, 34.00000000000000000 ) ) ;
#8830 = ORIENTED_EDGE ( 'NONE', *, *, #53492, .T. ) ;
#8831 = CARTESIAN_POINT ( 'NONE',  ( 17.84062500061451573, -3.027376345333610441, -5.243569643749999898 ) ) ;
#8832 = CARTESIAN_POINT ( 'NONE',  ( 3.853125000614517681, -4.541064518000417216, -2.621784821875001281 ) ) ;
#8833 = CARTESIAN_POINT ( 'NONE',  ( 17.40937500061451715, -4.541064518000417216, -2.621784821875001281 ) ) ;
#8834 = CARTESIAN_POINT ( 'NONE',  ( 28.95937500061451431, 0.000000000000000000, 5.243569643749999010 ) ) ;
#8835 = CARTESIAN_POINT ( 'NONE',  ( 4.003125000614518925, 4.541064518000418104, -2.621784821874998173 ) ) ;
#8836 = CARTESIAN_POINT ( 'NONE',  ( 19.30312500061451786, 4.541064518000418104, -2.621784821874998173 ) ) ;
#8837 = CARTESIAN_POINT ( 'NONE',  ( -4.243569643749999898, 14.40312500061451750, 30.00000000000000000 ) ) ;
#8838 = CARTESIAN_POINT ( 'NONE',  ( 17.43750000122903288, 4.330127018922191873, 2.499999999999999556 ) ) ;
#8839 = CARTESIAN_POINT ( 'NONE',  ( 13.50937500061451679, 4.119189519843966529, -2.378215178124998275 ) ) ;
#8840 = CARTESIAN_POINT ( 'NONE',  ( 7.078125000614516438, 6.421520780324663323E-16, -5.243569643749999010 ) ) ;
#8841 = CARTESIAN_POINT ( 'NONE',  ( 28.82812500061451644, 4.541064518000418104, 2.621784821874999949 ) ) ;
#8842 = CARTESIAN_POINT ( 'NONE',  ( 9.825000001229032165, 2.886751345948126879, 4.999999999999998224 ) ) ;
#8843 = CARTESIAN_POINT ( 'NONE',  ( 22.32187500061451502, -6.054752690667223547, -1.112240025338166033E-15 ) ) ;
#8844 = CARTESIAN_POINT ( 'NONE',  ( 14.39062500061451821, 6.054752690667223547, 3.707466751127219781E-16 ) ) ;
#8845 = CARTESIAN_POINT ( 'NONE',  ( 24.86250000122903359, -4.330127018922190985, -2.500000000000001332 ) ) ;
#8846 = CARTESIAN_POINT ( 'NONE',  ( 23.69062500061451004, -3.027376345333610441, -5.243569643749999898 ) ) ;
#8847 = CARTESIAN_POINT ( 'NONE',  ( 19.54687500061451644, -3.027376345333614438, 5.243569643749998122 ) ) ;
#8848 = CARTESIAN_POINT ( 'NONE',  ( 14.05312500061451431, 0.000000000000000000, 5.243569643749999010 ) ) ;
#8849 = CARTESIAN_POINT ( 'NONE',  ( 4.243569643749999010, 14.27187500061451964, 27.54997392385601174 ) ) ;
#8850 = CARTESIAN_POINT ( 'NONE',  ( 19.30312500061451786, 4.541064518000418104, -2.621784821874998173 ) ) ;
#8851 = CARTESIAN_POINT ( 'NONE',  ( 29.35312500061451502, 0.000000000000000000, 5.243569643749999010 ) ) ;
#8852 = EDGE_LOOP ( 'NONE', ( #41260, #26213, #43941, #556 ) ) ;
#8853 = EDGE_LOOP ( 'NONE', ( #41532, #34454, #58473, #17243 ) ) ;
#8854 = CARTESIAN_POINT ( 'NONE',  ( 24.11249999999999716, 2.886751345948126879, 4.999999999999999112 ) ) ;
#8855 = CARTESIAN_POINT ( 'NONE',  ( 3.999999999999999112, 10.32500000000000107, -30.00000000000000000 ) ) ;
#8856 = CARTESIAN_POINT ( 'NONE',  ( 13.08750000122903323, -4.330127018922194537, 2.499999999999995559 ) ) ;
#8857 = CARTESIAN_POINT ( 'NONE',  ( 27.14062500061451644, -3.027376345333614438, 5.243569643749998122 ) ) ;
#8858 = CARTESIAN_POINT ( 'NONE',  ( 7.528125000614515727, 6.421520780324663323E-16, -5.243569643749999010 ) ) ;
#8859 = CARTESIAN_POINT ( 'NONE',  ( 19.16250000122903430, 4.330127018922192761, -2.499999999999997780 ) ) ;
#8860 = CARTESIAN_POINT ( 'NONE',  ( 24.32812500061451289, 4.541064518000418104, 2.621784821874999949 ) ) ;
#8861 = CARTESIAN_POINT ( 'NONE',  ( 23.85000000000000142, -4.330127018922190985, -2.500000000000001332 ) ) ;
#8862 = CARTESIAN_POINT ( 'NONE',  ( 28.26562500061451289, 3.027376345333613106, -5.243569643749998122 ) ) ;
#8863 = CARTESIAN_POINT ( 'NONE',  ( 8.765625000614518214, -6.054752690667223547, -1.112240025338166033E-15 ) ) ;
#8864 = VERTEX_POINT ( 'NONE', #40474 ) ;
#8865 = EDGE_CURVE ( 'NONE', #24022, #6086, #22744, .T. ) ;
#8866 = CARTESIAN_POINT ( 'NONE',  ( 24.36562500061451786, 3.027376345333611329, 5.243569643749999010 ) ) ;
#8867 = CARTESIAN_POINT ( 'NONE',  ( 5.465625000614517504, 3.027376345333611329, 5.243569643749999010 ) ) ;
#8868 = CARTESIAN_POINT ( 'NONE',  ( 14.10937500061451644, 0.000000000000000000, 4.756430356249998326 ) ) ;
#8869 = CARTESIAN_POINT ( 'NONE',  ( 3.253125000614518036, 0.000000000000000000, 5.243569643749999010 ) ) ;
#8870 = CARTESIAN_POINT ( 'NONE',  ( 8.484601909799253346E-16, 12.57500000122903216, -25.38119784648299770 ) ) ;
#8871 = CARTESIAN_POINT ( 'NONE',  ( -1.071796769724491005, 13.60759618943233384, -34.00000000000000000 ) ) ;
#8872 = VECTOR ( 'NONE', #17167, 1000.000000000000000 ) ;
#8873 = CARTESIAN_POINT ( 'NONE',  ( 10.83750000000000036, -2.886751345948125991, -5.000000000000000000 ) ) ;
#8875 = CARTESIAN_POINT ( 'NONE',  ( 11.07187500061451679, -6.054752690667223547, -1.112240025338166033E-15 ) ) ;
#8874 = VECTOR ( 'NONE', #3541, 1000.000000000000000 ) ;
#8876 = CARTESIAN_POINT ( 'NONE',  ( 9.975000001229034297, -5.773502691896255534, -1.060575238724906372E-15 ) ) ;
#8877 = CARTESIAN_POINT ( 'NONE',  ( 14.82187500061451679, 3.027376345333613106, -5.243569643749998122 ) ) ;
#8878 = CARTESIAN_POINT ( 'NONE',  ( 14.47499999999999964, 6.123233995736764310E-16, -4.999999999999998224 ) ) ;
#8879 = CARTESIAN_POINT ( 'NONE',  ( 6.871875000614517504, 3.027376345333611329, 5.243569643749999010 ) ) ;
#8880 = CARTESIAN_POINT ( 'NONE',  ( 2.121784821875001281, 10.05312500061451608, -26.32496088578401938 ) ) ;
#8881 = CIRCLE ( 'NONE', #60761, 5.999999999999998224 ) ;
#8882 = DIRECTION ( 'NONE',  ( 0.000000000000000000, 0.000000000000000000, 1.000000000000000000 ) ) ;
#8883 = EDGE_CURVE ( 'NONE', #1580, #40669, #39029, .T. ) ;
#8884 = CARTESIAN_POINT ( 'NONE',  ( 13.05937500061451750, 4.541064518000418104, -2.621784821874998173 ) ) ;
#8885 = CARTESIAN_POINT ( 'NONE',  ( 13.23750000000000071, 5.773502691896255534, 3.535250795749688401E-16 ) ) ;
#8886 = CARTESIAN_POINT ( 'NONE',  ( 23.09062500061451573, -3.027376345333614438, 5.243569643749998122 ) ) ;
#8887 = CARTESIAN_POINT ( 'NONE',  ( 2.121784821875001281, 11.00937500061451857, 33.67503911421598417 ) ) ;
#8888 = CARTESIAN_POINT ( 'NONE',  ( 11.28749999999999964, -2.886751345948126435, -5.000000000000000000 ) ) ;
#8889 = CARTESIAN_POINT ( 'NONE',  ( 27.04687500061451644, 6.054752690667223547, 3.707466751127219781E-16 ) ) ;
#8890 =( BOUNDED_CURVE ( )  B_SPLINE_CURVE ( 2, ( #71518, #39363, #44908, #54888, #27914, #15349, #10187 ),
 .UNSPECIFIED., .F., .F. ) 
 B_SPLINE_CURVE_WITH_KNOTS ( ( 3, 2, 2, 3 ),
 ( 0.8083333333333333481, 0.8111111111111111160, 0.8138888888888888840, 0.8166666666666666519 ),
 .UNSPECIFIED. ) 
 CURVE ( )  GEOMETRIC_REPRESENTATION_ITEM ( )  RATIONAL_B_SPLINE_CURVE ( ( 1.000000000000000000, 0.8660254037844387076, 1.000000000000000000, 0.8660254037844387076, 1.000000000000000000, 0.8660254037844387076, 1.000000000000000000 ) ) 
 REPRESENTATION_ITEM ( '' )  );
#8891 = CARTESIAN_POINT ( 'NONE',  ( 15.78750000122903430, -4.330127018922194537, 2.499999999999995559 ) ) ;
#8892 = CARTESIAN_POINT ( 'NONE',  ( 5.353125000614515905, 4.541064518000418104, -2.621784821874998173 ) ) ;
#8893 = CARTESIAN_POINT ( 'NONE',  ( 22.65937500061451360, -5.492252693125287522, -1.008910452111647106E-15 ) ) ;
#8894 = CARTESIAN_POINT ( 'NONE',  ( 17.37187500061451573, -6.054752690667223547, -1.112240025338166033E-15 ) ) ;
#8895 = CARTESIAN_POINT ( 'NONE',  ( 8.146875000614516082, 0.000000000000000000, 4.756430356249998326 ) ) ;
#8896 = CARTESIAN_POINT ( 'NONE',  ( 27.52500000122903145, -5.773502691896255534, -1.060575238724906372E-15 ) ) ;
#8897 = CARTESIAN_POINT ( 'NONE',  ( 5.559375000614517504, 0.000000000000000000, 5.243569643749999010 ) ) ;
#8898 = CARTESIAN_POINT ( 'NONE',  ( 17.29687500061451999, -3.027376345333614438, 5.243569643749998122 ) ) ;
#8899 = CARTESIAN_POINT ( 'NONE',  ( -3.179521419646683889, 25.19832693812782054, 32.44092611819090166 ) ) ;
#8900 = CARTESIAN_POINT ( 'NONE',  ( 23.47499999999999787, 6.123233995736764310E-16, -4.999999999999998224 ) ) ;
#8901 = CARTESIAN_POINT ( 'NONE',  ( 3.375000001229033320, 2.886751345948129099, -4.999999999999998224 ) ) ;
#8903 = EDGE_CURVE ( 'NONE', #16877, #35360, #45857, .T. ) ;
#8902 = CARTESIAN_POINT ( 'NONE',  ( 27.38437500061451857, 6.421520780324663323E-16, -5.243569643749999010 ) ) ;
#8904 = CARTESIAN_POINT ( 'NONE',  ( -1.878215178125001827, 13.95312499938548356, 33.25316411605952283 ) ) ;
#8905 = CARTESIAN_POINT ( 'NONE',  ( 5.775000001229033231, 2.886751345948126879, 4.999999999999998224 ) ) ;
#8906 = CARTESIAN_POINT ( 'NONE',  ( 8.662499999999999645, 2.886751345948129099, -4.999999999999998224 ) ) ;
#8907 = CARTESIAN_POINT ( 'NONE',  ( 8.971875000614515372, 4.119189519843966529, 2.378215178124999607 ) ) ;
#8908 = CARTESIAN_POINT ( 'NONE',  ( 22.34062500061451573, -3.027376345333610441, -5.243569643749999898 ) ) ;
#8909 = CARTESIAN_POINT ( 'NONE',  ( 11.43750000000000000, 5.773502691896255534, 3.535250795749688894E-16 ) ) ;
#8910 = CARTESIAN_POINT ( 'NONE',  ( 3.065625000614517592, 3.027376345333613106, -5.243569643749998122 ) ) ;
#8911 = CARTESIAN_POINT ( 'NONE',  ( 18.78749999999999432, -2.886751345948129988, 4.999999999999997335 ) ) ;
#8912 = CARTESIAN_POINT ( 'NONE',  ( 19.22812500061451502, 6.421520780324663323E-16, -5.243569643749999010 ) ) ;
#8913 = CARTESIAN_POINT ( 'NONE',  ( 4.102673862605173305, -2.857983061023190441, 4.201819747086521062 ) ) ;
#8914 = CARTESIAN_POINT ( 'NONE',  ( 23.81250000122903288, 0.000000000000000000, 4.999999999999998224 ) ) ;
#8915 = CARTESIAN_POINT ( 'NONE',  ( -3.756430356250000990, 19.20312499938548356, 32.16877607737301048 ) ) ;
#8916 = CARTESIAN_POINT ( 'NONE',  ( 29.78437500061451715, 4.541064518000418104, 2.621784821874999949 ) ) ;
#8917 = AXIS2_PLACEMENT_3D ( 'NONE', #46832, #57892, #63802 ) ;
#8918 = ORIENTED_EDGE ( 'NONE', *, *, #25401, .T. ) ;
#8919 = CARTESIAN_POINT ( 'NONE',  ( 19.97812500061451502, -4.541064518000419881, 2.621784821874995952 ) ) ;
#8920 = CARTESIAN_POINT ( 'NONE',  ( 27.96562500061451928, 3.027376345333611329, 5.243569643749999010 ) ) ;
#8921 = CARTESIAN_POINT ( 'NONE',  ( 25.39687500061451431, -3.027376345333614438, 5.243569643749998122 ) ) ;
#8922 = CARTESIAN_POINT ( 'NONE',  ( 7.800000000000001599, 4.330127018922192761, -2.499999999999997780 ) ) ;
#8923 = CARTESIAN_POINT ( 'NONE',  ( 11.42812500061451608, -4.541064518000419881, 2.621784821874995952 ) ) ;
#8924 = CARTESIAN_POINT ( 'NONE',  ( 27.10312500061451502, 0.000000000000000000, 5.243569643749999010 ) ) ;
#8925 = CARTESIAN_POINT ( 'NONE',  ( 17.22187500061451715, 3.027376345333611329, 5.243569643749999010 ) ) ;
#8926 = CARTESIAN_POINT ( 'NONE',  ( 8.653125000614515727, 0.000000000000000000, 5.243569643749999010 ) ) ;
#8927 = CARTESIAN_POINT ( 'NONE',  ( 3.017996468573438396, -3.986467487895139605, 3.151570663109291459 ) ) ;
#8928 = CARTESIAN_POINT ( 'NONE',  ( -4.243569643749999898, 11.27187500061451608, 27.54997392385601529 ) ) ;
#8929 = CARTESIAN_POINT ( 'NONE',  ( 24.26250000122903216, 0.000000000000000000, 4.999999999999998224 ) ) ;
#8930 = CARTESIAN_POINT ( 'NONE',  ( 19.80937500061451573, 4.119189519843966529, -2.378215178124998275 ) ) ;
#8931 = CARTESIAN_POINT ( 'NONE',  ( 14.16562500061451679, -6.054752690667223547, -1.112240025338166033E-15 ) ) ;
#8932 = CARTESIAN_POINT ( 'NONE',  ( 9.871875000614517504, 3.027376345333613106, -5.243569643749998122 ) ) ;
#8933 = CARTESIAN_POINT ( 'NONE',  ( 10.28437500061451715, 6.421520780324663323E-16, -5.243569643749999010 ) ) ;
#8934 = ORIENTED_EDGE ( 'NONE', *, *, #26985, .T. ) ;
#8935 = CARTESIAN_POINT ( 'NONE',  ( 15.15000000000000036, 0.000000000000000000, 4.999999999999998224 ) ) ;
#8936 = CARTESIAN_POINT ( 'NONE',  ( 21.66562500061451502, 3.027376345333611329, 5.243569643749999010 ) ) ;
#8937 = CARTESIAN_POINT ( 'NONE',  ( 17.14687500061451786, 6.054752690667223547, 3.707466751127219781E-16 ) ) ;
#8938 = CARTESIAN_POINT ( 'NONE',  ( 20.95312500061451999, -4.541064518000417216, -2.621784821875001281 ) ) ;
#8939 = CARTESIAN_POINT ( 'NONE',  ( 4.000000000000000000, 11.63750000000000284, 32.30940107675849049 ) ) ;
#8940 = CARTESIAN_POINT ( 'NONE',  ( 27.21562500061451928, -6.054752690667223547, -1.112240025338166033E-15 ) ) ;
#8941 = CARTESIAN_POINT ( 'NONE',  ( 6.112500001229034474, 4.330127018922192761, -2.499999999999997780 ) ) ;
#8942 = VERTEX_POINT ( 'NONE', #1316 ) ;
#8943 = CARTESIAN_POINT ( 'NONE',  ( 3.112500001229034918, 0.000000000000000000, 4.999999999999998224 ) ) ;
#8944 = CARTESIAN_POINT ( 'NONE',  ( 2.000000000000001332, 17.44999999999999929, -26.53589838486224650 ) ) ;
#8945 = CARTESIAN_POINT ( 'NONE',  ( 25.80000000122903714, -2.886751345948125991, -5.000000000000000000 ) ) ;
#8946 = CARTESIAN_POINT ( 'NONE',  ( -7.967954043666661671E-16, 15.34062499938548463, 34.33755215474603517 ) ) ;
#8947 = CARTESIAN_POINT ( 'NONE',  ( 6.309375000614517504, 4.541064518000418104, -2.621784821874998173 ) ) ;
#8948 = CARTESIAN_POINT ( 'NONE',  ( 15.62812500061451537, 6.421520780324663323E-16, -5.243569643749999010 ) ) ;
#8949 = CARTESIAN_POINT ( 'NONE',  ( 8.409375000614518925, -4.541064518000417216, -2.621784821875001281 ) ) ;
#8950 = CARTESIAN_POINT ( 'NONE',  ( 26.25000000122903288, -2.886751345948125991, -5.000000000000000000 ) ) ;
#8951 =( BOUNDED_CURVE ( )  B_SPLINE_CURVE ( 2, ( #38234, #71867, #60764, #65210, #27167, #44162, #59664 ),
 .UNSPECIFIED., .F., .F. ) 
 B_SPLINE_CURVE_WITH_KNOTS ( ( 3, 2, 2, 3 ),
 ( 0.8399999999999999689, 0.8433333333333334902, 0.8466666666666667895, 0.8500000000000001998 ),
 .UNSPECIFIED. ) 
 CURVE ( )  GEOMETRIC_REPRESENTATION_ITEM ( )  RATIONAL_B_SPLINE_CURVE ( ( 1.000000000000000000, 0.8660254037844387076, 1.000000000000000000, 0.8660254037844387076, 1.000000000000000000, 0.8660254037844298258, 1.000000000000008882 ) ) 
 REPRESENTATION_ITEM ( '' )  );
#8952 = CARTESIAN_POINT ( 'NONE',  ( 17.52187500061451431, 3.027376345333612662, -5.243569643749998122 ) ) ;
#8953 = CARTESIAN_POINT ( 'NONE',  ( 6.159375000614517148, -4.541064518000417216, -2.621784821875001281 ) ) ;
#8954 = DIRECTION ( 'NONE',  ( 0.000000000000000000, 0.000000000000000000, 1.000000000000000000 ) ) ;
#8955 = CARTESIAN_POINT ( 'NONE',  ( 5.728125000614515905, 6.421520780324663323E-16, -5.243569643749999010 ) ) ;
#8956 =( BOUNDED_CURVE ( )  B_SPLINE_CURVE ( 2, ( #270, #637, #67867, #57490, #46417, #39799, #23144 ),
 .UNSPECIFIED., .F., .F. ) 
 B_SPLINE_CURVE_WITH_KNOTS ( ( 3, 2, 2, 3 ),
 ( 0.8583333333333332815, 0.8611111111111111605, 0.8638888888888889284, 0.8666666666666666963 ),
 .UNSPECIFIED. ) 
 CURVE ( )  GEOMETRIC_REPRESENTATION_ITEM ( )  RATIONAL_B_SPLINE_CURVE ( ( 1.000000000000000000, 0.8660254037844387076, 1.000000000000000000, 0.8660254037844387076, 1.000000000000000000, 0.8660254037844387076, 1.000000000000000000 ) ) 
 REPRESENTATION_ITEM ( '' )  );
#8957 = CARTESIAN_POINT ( 'NONE',  ( 15.02812500061451750, -4.541064518000419881, 2.621784821874995952 ) ) ;
#8958 = VERTEX_POINT ( 'NONE', #46376 ) ;
#8959 = CARTESIAN_POINT ( 'NONE',  ( 12.51562500061451821, 3.027376345333613106, -5.243569643749998122 ) ) ;
#8960 = CARTESIAN_POINT ( 'NONE',  ( 6.262500001229034829, 0.000000000000000000, 4.999999999999998224 ) ) ;
#8961 = CARTESIAN_POINT ( 'NONE',  ( 10.60312500061451679, -4.541064518000417216, -2.621784821875001281 ) ) ;
#8962 = CARTESIAN_POINT ( 'NONE',  ( 20.18437500061451573, 5.824947211148865298E-16, -4.756430356249998326 ) ) ;
#8963 = CARTESIAN_POINT ( 'NONE',  ( 11.28749999999999787, -2.886751345948125991, -5.000000000000000000 ) ) ;
#8964 = CARTESIAN_POINT ( 'NONE',  ( 4.012500001229033053, 0.000000000000000000, 4.999999999999998224 ) ) ;
#8965 = CARTESIAN_POINT ( 'NONE',  ( 20.36249999999999716, 2.886751345948129099, -4.999999999999998224 ) ) ;
#8966 = EDGE_CURVE ( 'NONE', #68862, #2641, #49314, .T. ) ;
#8967 =( BOUNDED_CURVE ( )  B_SPLINE_CURVE ( 2, ( #23792, #41170, #7178, #45981, #51527, #58127, #34519 ),
 .UNSPECIFIED., .F., .F. ) 
 B_SPLINE_CURVE_WITH_KNOTS ( ( 3, 2, 2, 3 ),
 ( 0.4500000000000000111, 0.4533333333333333104, 0.4566666666666666652, 0.4600000000000000200 ),
 .UNSPECIFIED. ) 
 CURVE ( )  GEOMETRIC_REPRESENTATION_ITEM ( )  RATIONAL_B_SPLINE_CURVE ( ( 1.000000000000000000, 0.8660254037844387076, 1.000000000000000000, 0.8660254037844387076, 1.000000000000000000, 0.8660254037844387076, 1.000000000000000000 ) ) 
 REPRESENTATION_ITEM ( '' )  );
#8968 = CARTESIAN_POINT ( 'NONE',  ( 17.97187500061451715, 3.027376345333613106, -5.243569643749998122 ) ) ;
#8969 = CARTESIAN_POINT ( 'NONE',  ( 16.12500000122903288, 2.886751345948126879, 4.999999999999999112 ) ) ;
#8970 = CARTESIAN_POINT ( 'NONE',  ( 21.44999999999999929, 0.000000000000000000, 4.999999999999998224 ) ) ;
#8971 = AXIS2_PLACEMENT_3D ( 'NONE', #62194, #68108, #45209 ) ;
#8972 = CARTESIAN_POINT ( 'NONE',  ( 4.243569643749999898, 16.87812500061451715, -30.00000000000000000 ) ) ;
#8973 = DIRECTION ( 'NONE',  ( 0.000000000000000000, 0.000000000000000000, -1.000000000000000000 ) ) ;
#8974 = CARTESIAN_POINT ( 'NONE',  ( 29.05312500061451431, -4.541064518000417216, -2.621784821875001281 ) ) ;
#8975 = FACE_OUTER_BOUND ( 'NONE', #45703, .T. ) ;
#8976 = CARTESIAN_POINT ( 'NONE',  ( -1.243387493232115393E-14, 15.76249999999999929, 26.00000000000000000 ) ) ;
#8977 = CARTESIAN_POINT ( 'NONE',  ( 16.43437500061451573, -4.541064518000419881, 2.621784821874995952 ) ) ;
#8978 = CARTESIAN_POINT ( 'NONE',  ( 18.28125000122903288, 4.330127018922191873, 2.499999999999999556 ) ) ;
#8979 = CARTESIAN_POINT ( 'NONE',  ( 11.05312500061451608, -4.541064518000417216, -2.621784821875001281 ) ) ;
#8980 = CARTESIAN_POINT ( 'NONE',  ( 7.106250001229032165, 0.000000000000000000, 4.999999999999998224 ) ) ;
#8981 = PRODUCT_DEFINITION_SHAPE ( 'NONE', 'NONE',  #45867 ) ;
#8982 = CARTESIAN_POINT ( 'NONE',  ( 23.18437500061451573, -4.541064518000419881, 2.621784821874995952 ) ) ;
#8983 = CARTESIAN_POINT ( 'NONE',  ( 15.49687500061451573, -4.119189519843965641, -2.378215178125001383 ) ) ;
#8984 = CARTESIAN_POINT ( 'NONE',  ( 6.815625000614517148, 3.027376345333611329, 5.243569643749999010 ) ) ;
#8985 = CARTESIAN_POINT ( 'NONE',  ( 14.25937500061451679, -4.541064518000417216, -2.621784821875001281 ) ) ;
#8986 = ORIENTED_EDGE ( 'NONE', *, *, #32530, .T. ) ;
#8987 = CARTESIAN_POINT ( 'NONE',  ( 24.42187500061451999, 3.027376345333611329, 5.243569643749999010 ) ) ;
#8988 = CARTESIAN_POINT ( 'NONE',  ( 28.11562500061451431, -6.054752690667223547, -1.112240025338166033E-15 ) ) ;
#8989 = CARTESIAN_POINT ( 'NONE',  ( 17.08125000122903003, -4.330127018922194537, 2.499999999999995559 ) ) ;
#8990 = CARTESIAN_POINT ( 'NONE',  ( 6.450000000000001066, 4.330127018922192761, -2.499999999999997780 ) ) ;
#8991 = CARTESIAN_POINT ( 'NONE',  ( 15.97500000122903430, 2.886751345948129099, -4.999999999999998224 ) ) ;
#8992 = CARTESIAN_POINT ( 'NONE',  ( -3.999999999999999112, 17.82500000122903572, -32.30940107675850470 ) ) ;
#8993 = CARTESIAN_POINT ( 'NONE',  ( 8.071875000614515017, 4.119189519843966529, 2.378215178124999607 ) ) ;
#8994 = VERTEX_POINT ( 'NONE', #22387 ) ;
#8995 = CARTESIAN_POINT ( 'NONE',  ( 15.15000000000000036, 0.000000000000000000, 4.999999999999998224 ) ) ;
#8996 = CARTESIAN_POINT ( 'NONE',  ( 19.72499999999999787, -4.330127018922194537, 2.499999999999995559 ) ) ;
#8997 = CARTESIAN_POINT ( 'NONE',  ( 12.59062500061451573, 6.054752690667223547, 3.707466751127219781E-16 ) ) ;
#8998 = VERTEX_POINT ( 'NONE', #39762 ) ;
#8999 = CARTESIAN_POINT ( 'NONE',  ( -4.000000000000000000, 16.71874999877096712, 30.00000000000000000 ) ) ;
#9000 = CARTESIAN_POINT ( 'NONE',  ( -3.000416591977282496E-16, 16.59687500061452070, -34.90005215228797653 ) ) ;
#9001 = CARTESIAN_POINT ( 'NONE',  ( 3.928125000614516527, 6.421520780324663323E-16, -5.243569643749999010 ) ) ;
#9002 = CARTESIAN_POINT ( 'NONE',  ( -7.967954043666661671E-16, 13.42812499938548321, 34.33755215474603517 ) ) ;
#9003 = CARTESIAN_POINT ( 'NONE',  ( 13.12500000000000178, 6.123233995736764310E-16, -4.999999999999998224 ) ) ;
#9004 = CARTESIAN_POINT ( 'NONE',  ( 27.64687500061451431, -4.119189519843965641, -2.378215178125001383 ) ) ;
#9005 = VERTEX_POINT ( 'NONE', #62279 ) ;
#9006 = CARTESIAN_POINT ( 'NONE',  ( 2.121784821875001281, 16.35312500061451857, 33.67503911421598417 ) ) ;
#9007 = CARTESIAN_POINT ( 'NONE',  ( 26.31562500061451715, -6.054752690667223547, -1.112240025338166033E-15 ) ) ;
#9008 = DIRECTION ( 'NONE',  ( 0.000000000000000000, 0.000000000000000000, -1.000000000000000000 ) ) ;
#9009 = CARTESIAN_POINT ( 'NONE',  ( 3.756430356249998770, 19.35312499938548214, 32.16877607737302469 ) ) ;
#9010 = CARTESIAN_POINT ( 'NONE',  ( 24.57187500061451502, -6.054752690667223547, -1.112240025338166033E-15 ) ) ;
#9011 = CARTESIAN_POINT ( 'NONE',  ( 18.32812500061451644, 6.421520780324663323E-16, -5.243569643749999010 ) ) ;
#9012 = ADVANCED_FACE ( 'NONE', ( #36372 ), #30469, .T. ) ;
#9013 = CARTESIAN_POINT ( 'NONE',  ( -2.121784821874996840, 13.12812500061459176, -26.32496088578401583 ) ) ;
#9014 = CARTESIAN_POINT ( 'NONE',  ( 24.56250000122903288, 4.330127018922192761, -2.499999999999997780 ) ) ;
#9015 = EDGE_CURVE ( 'NONE', #24863, #60259, #64072, .T. ) ;
#9016 = CARTESIAN_POINT ( 'NONE',  ( 5.090625000614516615, -3.027376345333614438, 5.243569643749998122 ) ) ;
#9017 = CARTESIAN_POINT ( 'NONE',  ( 26.07187500061451502, 2.746126346562645981, -4.756430356249997438 ) ) ;
#9018 = CARTESIAN_POINT ( 'NONE',  ( 20.35312500061451502, 0.000000000000000000, 5.243569643749999010 ) ) ;
#9019 = CARTESIAN_POINT ( 'NONE',  ( 9.384375000614518569, 5.824947211148865298E-16, -4.756430356249998326 ) ) ;
#9020 = CARTESIAN_POINT ( 'NONE',  ( -1.878215178124999163, 16.84062499938548285, 26.74683588394047007 ) ) ;
#9021 = CARTESIAN_POINT ( 'NONE',  ( 17.89687500061451431, -3.027376345333610441, -5.243569643749999898 ) ) ;
#9022 = CARTESIAN_POINT ( 'NONE',  ( 16.32187500061451502, 3.027376345333611329, 5.243569643749999010 ) ) ;
#9023 = CARTESIAN_POINT ( 'NONE',  ( 25.35937500061451644, 0.000000000000000000, 5.243569643749999010 ) ) ;
#9024 = CARTESIAN_POINT ( 'NONE',  ( -2.121784821874999949, 13.93437500061451750, 26.32496088578401938 ) ) ;
#9025 = CARTESIAN_POINT ( 'NONE',  ( 5.428125000614517859, 4.541064518000418104, 2.621784821874999949 ) ) ;
#9026 = CARTESIAN_POINT ( 'NONE',  ( 28.15312500061451573, -4.541064518000417216, -2.621784821875001281 ) ) ;
#9027 = CARTESIAN_POINT ( 'NONE',  ( 2.896875000614518747, -3.027376345333614438, 5.243569643749998122 ) ) ;
#9028 = CARTESIAN_POINT ( 'NONE',  ( -1.626862140677534273E-15, 16.43750000000000000, 34.00000000000000000 ) ) ;
#9029 = CARTESIAN_POINT ( 'NONE',  ( -3.999999999999999112, 18.64999999999999858, 30.00000000000000000 ) ) ;
#9030 = AXIS2_PLACEMENT_3D ( 'NONE', #62036, #12148, #49869 ) ;
#9031 = CARTESIAN_POINT ( 'NONE',  ( 7.246875000614518392, 6.054752690667223547, 3.707466751127219781E-16 ) ) ;
#9032 = CARTESIAN_POINT ( 'NONE',  ( 13.76250000122903394, 4.330127018922192761, -2.499999999999997780 ) ) ;
#9033 = CARTESIAN_POINT ( 'NONE',  ( 10.05000000122903181, -2.886751345948125991, -5.000000000000000000 ) ) ;
#9034 = CARTESIAN_POINT ( 'NONE',  ( 5.015625000614518214, 3.027376345333611329, 5.243569643749999010 ) ) ;
#9035 = CARTESIAN_POINT ( 'NONE',  ( -1.999999999999999112, 17.09374999877096712, 26.53589838486224650 ) ) ;
#9036 = CARTESIAN_POINT ( 'NONE',  ( 20.11875000122903145, 2.886751345948126879, 4.999999999999999112 ) ) ;
#9037 = CARTESIAN_POINT ( 'NONE',  ( 14.63437500061451679, -4.541064518000419881, 2.621784821874995952 ) ) ;
#9038 = CARTESIAN_POINT ( 'NONE',  ( 10.00000000000000000, 1.224646799147353256E-15, 50.00000000000000000 ) ) ;
#9039 = EDGE_LOOP ( 'NONE', ( #49478, #2361, #5672, #54652 ) ) ;
#9040 = CARTESIAN_POINT ( 'NONE',  ( 22.37812500061451360, 6.421520780324663323E-16, -5.243569643749999010 ) ) ;
#9041 = CARTESIAN_POINT ( 'NONE',  ( 6.553125000614518747, -4.541064518000417216, -2.621784821875001281 ) ) ;
#9042 = CARTESIAN_POINT ( 'NONE',  ( 24.75937500061451502, 4.541064518000418104, -2.621784821874998173 ) ) ;
#9043 = CARTESIAN_POINT ( 'NONE',  ( 7.303125000614516082, 0.000000000000000000, 5.243569643749999010 ) ) ;
#9044 = CARTESIAN_POINT ( 'NONE',  ( 3.756430356250000102, 12.75312499938548427, 30.00000000000000000 ) ) ;
#9045 = CARTESIAN_POINT ( 'NONE',  ( 9.037500001229034297, -4.330127018922194537, 2.499999999999995559 ) ) ;
#9046 = CARTESIAN_POINT ( 'NONE',  ( 21.74062500061451431, -3.027376345333614438, 5.243569643749998122 ) ) ;
#9047 = CARTESIAN_POINT ( 'NONE',  ( -4.243569643749999898, 10.31562500061451715, -32.45002607614398471 ) ) ;
#9048 = CARTESIAN_POINT ( 'NONE',  ( 11.32500000122903394, -5.773502691896255534, -1.060575238724906372E-15 ) ) ;
#9049 = CARTESIAN_POINT ( 'NONE',  ( 20.24062500061451431, 6.054752690667223547, 3.707466751127219781E-16 ) ) ;
#9050 = CARTESIAN_POINT ( 'NONE',  ( 19.00312500061451715, 0.000000000000000000, 5.243569643749999010 ) ) ;
#9051 = CARTESIAN_POINT ( 'NONE',  ( 27.42187500061451644, 2.746126346562645981, -4.756430356249997438 ) ) ;
#9052 = CARTESIAN_POINT ( 'NONE',  ( 18.93750000000000000, -2.886751345948125991, -5.000000000000000000 ) ) ;
#9053 = CARTESIAN_POINT ( 'NONE',  ( 11.36250000122903536, -4.330127018922190985, -2.500000000000001332 ) ) ;
#9054 = ADVANCED_FACE ( 'NONE', ( #25280 ), #55781, .T. ) ;
#9055 = CARTESIAN_POINT ( 'NONE',  ( 7.715625000614515727, 3.027376345333611329, 5.243569643749999010 ) ) ;
#9056 = CARTESIAN_POINT ( 'NONE',  ( 13.94062500061451892, 6.054752690667223547, 3.707466751127219781E-16 ) ) ;
#9057 = CARTESIAN_POINT ( 'NONE',  ( 22.61250000122903003, -4.330127018922190985, -2.500000000000001332 ) ) ;
#9058 = CARTESIAN_POINT ( 'NONE',  ( 20.78437500061451715, 4.541064518000418104, 2.621784821874999949 ) ) ;
#9059 = VECTOR ( 'NONE', #16356, 1000.000000000000000 ) ;
#9060 = CARTESIAN_POINT ( 'NONE',  ( 4.350000001229033408, 5.773502691896255534, 3.535250795749688894E-16 ) ) ;
#9061 = CARTESIAN_POINT ( 'NONE',  ( 7.396875000614519635, -3.027376345333614438, 5.243569643749998122 ) ) ;
#9062 = CARTESIAN_POINT ( 'NONE',  ( 22.20937500061451431, 0.000000000000000000, 5.243569643749999010 ) ) ;
#9063 = CARTESIAN_POINT ( 'NONE',  ( -2.000000000000001776, 12.80000000000000071, 33.46410161513775705 ) ) ;
#9064 = CARTESIAN_POINT ( 'NONE',  ( 19.64062500061451644, -3.027376345333610441, -5.243569643749999898 ) ) ;
#9065 = CARTESIAN_POINT ( 'NONE',  ( 23.48437500061451644, 4.541064518000418104, 2.621784821874999949 ) ) ;
#9066 = CARTESIAN_POINT ( 'NONE',  ( 3.756430356250000546, 20.44062499938548427, 27.83122392262697886 ) ) ;
#9067 = CARTESIAN_POINT ( 'NONE',  ( 27.67500000122903359, 2.886751345948146419, -4.999999999999968914 ) ) ;
#9068 = CARTESIAN_POINT ( 'NONE',  ( 5.296875000614518214, -3.027376345333610441, -5.243569643749999898 ) ) ;
#9069 = CARTESIAN_POINT ( 'NONE',  ( 16.07812500061451289, 6.421520780324663323E-16, -5.243569643749999010 ) ) ;
#9070 = CARTESIAN_POINT ( 'NONE',  ( 13.35937500061451821, -4.541064518000417216, -2.621784821875001281 ) ) ;
#9071 = VERTEX_POINT ( 'NONE', #13655 ) ;
#9072 = CARTESIAN_POINT ( 'NONE',  ( 22.19999999999999574, 4.330127018922192761, -2.499999999999997780 ) ) ;
#9073 = CARTESIAN_POINT ( 'NONE',  ( 24.36562500061451786, 3.027376345333611329, 5.243569643749999010 ) ) ;
#9074 = CARTESIAN_POINT ( 'NONE',  ( 1.071796769724484344, 16.98259618943233562, 34.00000000000000000 ) ) ;
#9075 = CARTESIAN_POINT ( 'NONE',  ( -3.999999999999999112, 18.27500000122903501, 27.69059892324149885 ) ) ;
#9076 = CARTESIAN_POINT ( 'NONE',  ( 15.33750000000000036, -2.886751345948125991, -5.000000000000000000 ) ) ;
#9077 = CARTESIAN_POINT ( 'NONE',  ( 23.85000000122903430, -2.886751345948129988, 4.999999999999997335 ) ) ;
#9078 = CARTESIAN_POINT ( 'NONE',  ( 17.50312500061451715, 4.541064518000418104, -2.621784821874998173 ) ) ;
#9079 = ORIENTED_EDGE ( 'NONE', *, *, #15629, .T. ) ;
#9080 = CARTESIAN_POINT ( 'NONE',  ( 23.36250000000000071, -5.773502691896255534, -1.060575238724906372E-15 ) ) ;
#9081 = CARTESIAN_POINT ( 'NONE',  ( 24.34687500061451715, 6.054752690667223547, 3.707466751127219781E-16 ) ) ;
#9082 = ORIENTED_EDGE ( 'NONE', *, *, #50559, .T. ) ;
#9083 = CARTESIAN_POINT ( 'NONE',  ( 11.73750000000000071, -2.886751345948126435, -5.000000000000000000 ) ) ;
#9084 = CARTESIAN_POINT ( 'NONE',  ( 9.553125000614517859, 0.000000000000000000, 5.243569643749999010 ) ) ;
#9085 = CARTESIAN_POINT ( 'NONE',  ( 4.340625000614515727, -3.027376345333610441, -5.243569643749999898 ) ) ;
#9086 = CARTESIAN_POINT ( 'NONE',  ( 17.67187500061451644, -4.119189519843968306, 2.378215178124996054 ) ) ;
#9087 = CARTESIAN_POINT ( 'NONE',  ( 26.57812500061451644, 4.541064518000418104, 2.621784821874999949 ) ) ;
#9088 = CARTESIAN_POINT ( 'NONE',  ( 20.43749999999999645, 5.773502691896255534, 3.535250795749688894E-16 ) ) ;
#9089 = CARTESIAN_POINT ( 'NONE',  ( 27.11249999999999716, 2.886751345948129099, -4.999999999999998224 ) ) ;
#9090 = CARTESIAN_POINT ( 'NONE',  ( 4.000000000000000000, 14.24374999877096748, 30.00000000000000000 ) ) ;
#9091 = CARTESIAN_POINT ( 'NONE',  ( 7.921875000614517326, -6.054752690667223547, -1.112240025338166033E-15 ) ) ;
#9092 = CARTESIAN_POINT ( 'NONE',  ( 17.74687500061451928, -3.027376345333614438, 5.243569643749998122 ) ) ;
#9093 = CARTESIAN_POINT ( 'NONE',  ( -3.137519842735245283E-14, 11.22500000122903430, 34.00000000000000000 ) ) ;
#9094 = VERTEX_POINT ( 'NONE', #12574 ) ;
#9095 = CARTESIAN_POINT ( 'NONE',  ( 25.90312500061451573, -4.541064518000417216, -2.621784821875001281 ) ) ;
#9096 = CARTESIAN_POINT ( 'NONE',  ( 28.28437500061451715, 6.421520780324663323E-16, -5.243569643749999010 ) ) ;
#9097 = CARTESIAN_POINT ( 'NONE',  ( 45.00000000000000000, 6.123233995736764310E-16, -4.999999999999998224 ) ) ;
#9098 = CARTESIAN_POINT ( 'NONE',  ( 15.78749999999999964, -2.886751345948125991, -5.000000000000000000 ) ) ;
#9099 = CARTESIAN_POINT ( 'NONE',  ( 12.10312500061451857, 4.541064518000418104, -2.621784821874998173 ) ) ;
#9100 = DIRECTION ( 'NONE',  ( -1.000000000000000000, -0.000000000000000000, -0.000000000000000000 ) ) ;
#9101 = DIRECTION ( 'NONE',  ( -1.000000000000000000, -0.000000000000000000, -0.000000000000000000 ) ) ;
#9102 = CARTESIAN_POINT ( 'NONE',  ( 28.30312500061451431, 4.541064518000418104, -2.621784821874998173 ) ) ;
#9103 = CARTESIAN_POINT ( 'NONE',  ( 18.82500000122903216, 2.886751345948126879, 4.999999999999999112 ) ) ;
#9104 = LINE ( 'NONE', #32002, #27709 ) ;
#9105 = CARTESIAN_POINT ( 'NONE',  ( 18.72187500061451360, -5.492252693125287522, -1.008910452111647106E-15 ) ) ;
#9106 = CARTESIAN_POINT ( 'NONE',  ( 6.140625000614516438, -3.027376345333610441, -5.243569643749999898 ) ) ;
#9107 = CARTESIAN_POINT ( 'NONE',  ( 23.07187500061451857, 3.027376345333611329, 5.243569643749999010 ) ) ;
#9108 = CARTESIAN_POINT ( 'NONE',  ( 4.243569643749999898, 17.83437500061451786, 30.00000000000000000 ) ) ;
#9109 = CARTESIAN_POINT ( 'NONE',  ( 24.68437500061451573, 6.421520780324663323E-16, -5.243569643749999010 ) ) ;
#9110 = CARTESIAN_POINT ( 'NONE',  ( 5.325000000000000178, -4.330127018922194537, 2.499999999999995559 ) ) ;
#9111 = CARTESIAN_POINT ( 'NONE',  ( -3.999999999999999556, 10.17500000122903359, 27.69059892324149530 ) ) ;
#9112 = CARTESIAN_POINT ( 'NONE',  ( 13.15312500061451750, 0.000000000000000000, 5.243569643749999010 ) ) ;
#9113 = CARTESIAN_POINT ( 'NONE',  ( 5.437500001229035540, -4.330127018922194537, 2.499999999999995559 ) ) ;
#9114 = CARTESIAN_POINT ( 'NONE',  ( 9.684375000614517504, -4.541064518000419881, 2.621784821874995952 ) ) ;
#9115 = CARTESIAN_POINT ( 'NONE',  ( 7.050000000000000711, 0.000000000000000000, 4.999999999999998224 ) ) ;
#9116 = CARTESIAN_POINT ( 'NONE',  ( 10.60312500061451679, -4.541064518000417216, -2.621784821875001281 ) ) ;
#9117 = CARTESIAN_POINT ( 'NONE',  ( 14.44687500061451679, 6.054752690667223547, 3.707466751127219781E-16 ) ) ;
#9118 = CARTESIAN_POINT ( 'NONE',  ( 21.65625000122903288, -4.330127018922190985, -2.500000000000001332 ) ) ;
#9119 = CARTESIAN_POINT ( 'NONE',  ( 21.67500000122903359, -5.773502691896255534, -1.060575238724906372E-15 ) ) ;
#9120 = CARTESIAN_POINT ( 'NONE',  ( 11.33437500061451608, 4.541064518000418104, 2.621784821874999949 ) ) ;
#9121 = CARTESIAN_POINT ( 'NONE',  ( 11.80312500061451608, 0.000000000000000000, 5.243569643749999010 ) ) ;
#9122 = CARTESIAN_POINT ( 'NONE',  ( 29.26875000122903003, -5.773502691896255534, -1.060575238724906372E-15 ) ) ;
#9123 = CARTESIAN_POINT ( 'NONE',  ( 20.89687500061452141, -3.027376345333614438, 5.243569643749998122 ) ) ;
#9124 = CYLINDRICAL_SURFACE ( 'NONE', #21880, 4.999999999999998224 ) ;
#9125 = CARTESIAN_POINT ( 'NONE',  ( -2.000000000000000000, 11.93750000122903465, -33.46410161513775705 ) ) ;
#9126 = VECTOR ( 'NONE', #50705, 1000.000000000000000 ) ;
#9127 = CARTESIAN_POINT ( 'NONE',  ( -2.556497649636125342E-15, 18.87500000122903288, -26.00000000000000355 ) ) ;
#9128 = CARTESIAN_POINT ( 'NONE',  ( -2.121784821874999949, 14.83437500061451786, -33.67503911421598417 ) ) ;
#9129 = CARTESIAN_POINT ( 'NONE',  ( 14.10000000122903252, -2.886751345948125991, -5.000000000000000000 ) ) ;
#9130 = CARTESIAN_POINT ( 'NONE',  ( 10.80937500061451928, 4.541064518000418104, -2.621784821874998173 ) ) ;
#9131 = CARTESIAN_POINT ( 'NONE',  ( -2.121784821874996840, 18.97812500061451857, -26.32496088578401583 ) ) ;
#9132 = CARTESIAN_POINT ( 'NONE',  ( 17.36250000122903359, 4.330127018922192761, -2.499999999999997780 ) ) ;
#9133 = CARTESIAN_POINT ( 'NONE',  ( 12.70312500061451821, 0.000000000000000000, 5.243569643749999010 ) ) ;
#9134 = VERTEX_POINT ( 'NONE', #36198 ) ;
#9135 = CARTESIAN_POINT ( 'NONE',  ( 15.86250000000000249, 2.886751345948129099, -4.999999999999998224 ) ) ;
#9136 = CARTESIAN_POINT ( 'NONE',  ( 4.603329117574985752, 1.951758446961684434, -4.603329117574985752 ) ) ;
#9137 = CARTESIAN_POINT ( 'NONE',  ( 9.159375000614515372, 0.000000000000000000, 5.243569643749999010 ) ) ;
#9138 = CARTESIAN_POINT ( 'NONE',  ( 30.00000000000000000, 6.123233995736764310E-16, -4.999999999999998224 ) ) ;
#9139 = CARTESIAN_POINT ( 'NONE',  ( 13.80000000122903181, 5.773502691896255534, 3.535250795749688894E-16 ) ) ;
#9140 = CARTESIAN_POINT ( 'NONE',  ( 19.83750000122903145, -4.330127018922194537, 2.499999999999995559 ) ) ;
#9141 = CARTESIAN_POINT ( 'NONE',  ( 16.75312500061451715, 0.000000000000000000, 5.243569643749999010 ) ) ;
#9142 = CARTESIAN_POINT ( 'NONE',  ( 21.17812500061451431, 4.541064518000418104, 2.621784821874999949 ) ) ;
#9143 = CARTESIAN_POINT ( 'NONE',  ( 28.87500000122902932, -5.773502691896255534, -1.060575238724906372E-15 ) ) ;
#9144 = EDGE_CURVE ( 'NONE', #59952, #57422, #60946, .T. ) ;
#9145 = CARTESIAN_POINT ( 'NONE',  ( 4.753125000614515372, -4.541064518000417216, -2.621784821875001281 ) ) ;
#9146 = CARTESIAN_POINT ( 'NONE',  ( 25.08749999999999858, -2.886751345948129988, 4.999999999999997335 ) ) ;
#9147 = DIRECTION ( 'NONE',  ( -1.000000000000000000, -0.000000000000000000, -0.000000000000000000 ) ) ;
#9148 = CARTESIAN_POINT ( 'NONE',  ( 7.696875000614516793, 5.492252693125287522, 3.363034840372157021E-16 ) ) ;
#9149 = CARTESIAN_POINT ( 'NONE',  ( 29.14687500061451075, -3.027376345333610441, -5.243569643749999898 ) ) ;
#9150 = CARTESIAN_POINT ( 'NONE',  ( -5.810221930991193690E-16, 15.83749999999999680, 26.00000000000000355 ) ) ;
#9151 = CARTESIAN_POINT ( 'NONE',  ( 2.812500001229033320, -4.330127018922190985, -2.500000000000001332 ) ) ;
#9152 = CARTESIAN_POINT ( 'NONE',  ( 29.70937500061451431, 4.541064518000418104, -2.621784821874998173 ) ) ;
#9153 = LINE ( 'NONE', #21686, #65597 ) ;
#9154 = CARTESIAN_POINT ( 'NONE',  ( 7.471875000614519813, -6.054752690667223547, -1.112240025338166033E-15 ) ) ;
#9155 = CARTESIAN_POINT ( 'NONE',  ( 25.26562500061451289, 3.027376345333611329, 5.243569643749999010 ) ) ;
#9156 = CARTESIAN_POINT ( 'NONE',  ( 9.281250001229032875, 4.330127018922191873, 2.499999999999999556 ) ) ;
#9157 = CARTESIAN_POINT ( 'NONE',  ( 22.34999999999999787, 0.000000000000000000, 4.999999999999998224 ) ) ;
#9158 = CARTESIAN_POINT ( 'NONE',  ( 3.708868255654138135, -3.353251595422250375, 3.928382055777434267 ) ) ;
#9159 = CARTESIAN_POINT ( 'NONE',  ( 4.471875000614518925, 3.027376345333613106, -5.243569643749998122 ) ) ;
#9160 = CARTESIAN_POINT ( 'NONE',  ( 8.596875000614518925, 6.054752690667223547, 3.707466751127219781E-16 ) ) ;
#9161 = CARTESIAN_POINT ( 'NONE',  ( 3.112500000000000711, -5.773502691896255534, -1.060575238724906372E-15 ) ) ;
#9162 = CARTESIAN_POINT ( 'NONE',  ( -4.243569643749998122, 11.29062500061459495, 32.45002607614398471 ) ) ;
#9163 = CARTESIAN_POINT ( 'NONE',  ( 21.30000000000000071, 4.330127018922192761, -2.499999999999997780 ) ) ;
#9164 =( BOUNDED_CURVE ( )  B_SPLINE_CURVE ( 2, ( #68854, #6068, #1624, #29683, #18581, #13045, #35584 ),
 .UNSPECIFIED., .F., .F. ) 
 B_SPLINE_CURVE_WITH_KNOTS ( ( 3, 2, 2, 3 ),
 ( 0.6500000000000000222, 0.6533333333333333215, 0.6566666666666666208, 0.6600000000000000311 ),
 .UNSPECIFIED. ) 
 CURVE ( )  GEOMETRIC_REPRESENTATION_ITEM ( )  RATIONAL_B_SPLINE_CURVE ( ( 1.000000000000000000, 0.8660254037844387076, 1.000000000000000000, 0.8660254037844387076, 1.000000000000000000, 0.8660254037844387076, 1.000000000000000000 ) ) 
 REPRESENTATION_ITEM ( '' )  );
#9165 = CARTESIAN_POINT ( 'NONE',  ( 3.900000000000000799, 0.000000000000000000, 4.999999999999998224 ) ) ;
#9166 = CARTESIAN_POINT ( 'NONE',  ( 16.35937500061451644, -5.492252693125287522, -1.008910452111647106E-15 ) ) ;
#9167 = ORIENTED_EDGE ( 'NONE', *, *, #68280, .T. ) ;
#9168 = CARTESIAN_POINT ( 'NONE',  ( 21.44062500061452070, -3.027376345333610441, -5.243569643749999898 ) ) ;
#9169 = CARTESIAN_POINT ( 'NONE',  ( 10.26562500061451644, 3.027376345333613106, -5.243569643749998122 ) ) ;
#9170 = CARTESIAN_POINT ( 'NONE',  ( 23.10937500061451644, -5.492252693125287522, -1.008910452111647106E-15 ) ) ;
#9171 = CARTESIAN_POINT ( 'NONE',  ( 6.646875000614518747, -3.027376345333610441, -5.243569643749999898 ) ) ;
#9172 = CARTESIAN_POINT ( 'NONE',  ( 24.11249999999999716, 2.886751345948126879, 4.999999999999999112 ) ) ;
#9173 = CARTESIAN_POINT ( 'NONE',  ( 19.05000000122903359, -2.886751345948125991, -5.000000000000000000 ) ) ;
#9174 = CARTESIAN_POINT ( 'NONE',  ( 27.40312500061451573, 4.541064518000418104, -2.621784821874998173 ) ) ;
#9175 = CARTESIAN_POINT ( 'NONE',  ( 24.03750000000000142, 5.773502691896255534, 3.535250795749688401E-16 ) ) ;
#9176 = CARTESIAN_POINT ( 'NONE',  ( 9.046875000614518214, 6.054752690667223547, 3.707466751127219781E-16 ) ) ;
#9177 = CARTESIAN_POINT ( 'NONE',  ( 13.35937500061451821, -4.541064518000417216, -2.621784821875001281 ) ) ;
#9178 = CARTESIAN_POINT ( 'NONE',  ( 24.27187500061452141, 3.027376345333613106, -5.243569643749998122 ) ) ;
#9179 = CARTESIAN_POINT ( 'NONE',  ( -1.487416814333745711E-14, 16.06250000000000000, 34.00000000000000000 ) ) ;
#9180 = CARTESIAN_POINT ( 'NONE',  ( 13.87500000000000178, -4.330127018922194537, 2.499999999999995559 ) ) ;
#9181 = CARTESIAN_POINT ( 'NONE',  ( 19.17187500061451999, -6.054752690667223547, -1.112240025338166033E-15 ) ) ;
#9182 = CARTESIAN_POINT ( 'NONE',  ( 8.409375000614518925, -4.541064518000417216, -2.621784821875001281 ) ) ;
#9183 = CARTESIAN_POINT ( 'NONE',  ( 1.878215178125000495, 20.47812499938548569, 26.74683588394047007 ) ) ;
#9184 = CARTESIAN_POINT ( 'NONE',  ( 23.88749999999999929, -2.886751345948125991, -5.000000000000000000 ) ) ;
#9185 = CARTESIAN_POINT ( 'NONE',  ( -4.000000000000000888, 14.56250000000000000, 32.30940107675850470 ) ) ;
#9186 = CARTESIAN_POINT ( 'NONE',  ( -2.000000000000001776, 17.30000000000000071, 33.46410161513775705 ) ) ;
#9187 = CARTESIAN_POINT ( 'NONE',  ( 25.92187500061451999, -5.492252693125287522, -1.008910452111647106E-15 ) ) ;
#9188 = CARTESIAN_POINT ( 'NONE',  ( 12.66562500061451502, 3.027376345333611329, 5.243569643749999010 ) ) ;
#9189 = CARTESIAN_POINT ( 'NONE',  ( 4.500000000000000888, -4.330127018922190985, -2.500000000000001332 ) ) ;
#9190 = CARTESIAN_POINT ( 'NONE',  ( 15.82499999999999929, 6.123233995736764310E-16, -4.999999999999998224 ) ) ;
#9191 = DIRECTION ( 'NONE',  ( 0.000000000000000000, 1.000000000000000000, -0.000000000000000000 ) ) ;
#9192 = CARTESIAN_POINT ( 'NONE',  ( 11.70000000000000284, -4.330127018922190985, -2.500000000000001332 ) ) ;
#9193 = CARTESIAN_POINT ( 'NONE',  ( 1.999999999999998668, 18.16250000122903074, 26.53589838486224650 ) ) ;
#9194 = CARTESIAN_POINT ( 'NONE',  ( 10.50000000122903465, -2.886751345948125991, -5.000000000000000000 ) ) ;
#9195 = CARTESIAN_POINT ( 'NONE',  ( 21.98437500061451644, 6.421520780324663323E-16, -5.243569643749999010 ) ) ;
#9196 = CARTESIAN_POINT ( 'NONE',  ( 16.50937500061451502, -4.541064518000417216, -2.621784821875001281 ) ) ;
#9197 = CARTESIAN_POINT ( 'NONE',  ( 20.21250000122903145, 0.000000000000000000, 4.999999999999998224 ) ) ;
#9198 = ORIENTED_EDGE ( 'NONE', *, *, #37402, .F. ) ;
#9199 = CARTESIAN_POINT ( 'NONE',  ( 17.27812500061451217, -4.541064518000419881, 2.621784821874995952 ) ) ;
#9200 = CARTESIAN_POINT ( 'NONE',  ( 2.915625000614516793, -6.054752690667223547, -1.112240025338166033E-15 ) ) ;
#9201 = CARTESIAN_POINT ( 'NONE',  ( 17.85937500061451999, -4.541064518000417216, -2.621784821875001281 ) ) ;
#9202 = CARTESIAN_POINT ( 'NONE',  ( 29.78437500061451715, 4.541064518000418104, 2.621784821874999949 ) ) ;
#9203 = CARTESIAN_POINT ( 'NONE',  ( 3.703125000614516882, 0.000000000000000000, 5.243569643749999010 ) ) ;
#9204 = CARTESIAN_POINT ( 'NONE',  ( 18.55312500061451431, 0.000000000000000000, 5.243569643749999010 ) ) ;
#9205 = CARTESIAN_POINT ( 'NONE',  ( 28.17187500061451644, -6.054752690667223547, -1.112240025338166033E-15 ) ) ;
#9206 = CARTESIAN_POINT ( 'NONE',  ( 4.243569643749999898, 13.72812500061451679, 30.00000000000000000 ) ) ;
#9207 = CARTESIAN_POINT ( 'NONE',  ( 17.62500000122903288, -5.773502691896255534, -1.060575238724906372E-15 ) ) ;
#9208 = CARTESIAN_POINT ( 'NONE',  ( 8.859375000614518214, -4.119189519843965641, -2.378215178125001383 ) ) ;
#9209 = CARTESIAN_POINT ( 'NONE',  ( 8.240625000614516082, -3.027376345333614438, 5.243569643749998122 ) ) ;
#9210 = CARTESIAN_POINT ( 'NONE',  ( 26.01562500061451289, 3.027376345333613106, -5.243569643749998122 ) ) ;
#9211 = CARTESIAN_POINT ( 'NONE',  ( 1.510657702057710734E-15, 19.10000000122903430, -33.99999999999999289 ) ) ;
#9212 = CARTESIAN_POINT ( 'NONE',  ( 22.39687500061451075, -3.027376345333610441, -5.243569643749999898 ) ) ;
#9213 = CARTESIAN_POINT ( 'NONE',  ( 13.34062500061451750, -3.027376345333610441, -5.243569643749999898 ) ) ;
#9214 = CARTESIAN_POINT ( 'NONE',  ( 22.76250000122903216, 4.330127018922192761, -2.499999999999997780 ) ) ;
#9215 = CARTESIAN_POINT ( 'NONE',  ( 23.91562500061451502, 3.027376345333611329, 5.243569643749999010 ) ) ;
#9216 = CARTESIAN_POINT ( 'NONE',  ( 18.49687500061452283, 6.054752690667223547, 3.707466751127219781E-16 ) ) ;
#9217 = CARTESIAN_POINT ( 'NONE',  ( 12.62812500061451537, 4.541064518000418104, 2.621784821874999949 ) ) ;
#9218 = CARTESIAN_POINT ( 'NONE',  ( 2.121784821874999061, 15.65937500061451892, 26.32496088578401583 ) ) ;
#9219 = CARTESIAN_POINT ( 'NONE',  ( 20.35312500061451502, 0.000000000000000000, 5.243569643749999010 ) ) ;
#9220 = FACE_OUTER_BOUND ( 'NONE', #11981, .T. ) ;
#9221 = ORIENTED_EDGE ( 'NONE', *, *, #49500, .T. ) ;
#9222 = EDGE_LOOP ( 'NONE', ( #42752, #16126, #24636, #20805 ) ) ;
#9223 = CARTESIAN_POINT ( 'NONE',  ( 21.89999999999999858, 0.000000000000000000, 4.999999999999998224 ) ) ;
#9224 = CARTESIAN_POINT ( 'NONE',  ( 3.999999999999998668, 10.36250000000000071, -32.30940107675850470 ) ) ;
#9225 = CARTESIAN_POINT ( 'NONE',  ( 14.79375000122903039, -2.886751345948130876, 4.999999999999996447 ) ) ;
#9226 = CARTESIAN_POINT ( 'NONE',  ( 26.46562500061451573, 3.027376345333613106, -5.243569643749998122 ) ) ;
#9227 = CARTESIAN_POINT ( 'NONE',  ( 6.215625000614517504, 3.027376345333613106, -5.243569643749998122 ) ) ;
#9228 = CARTESIAN_POINT ( 'NONE',  ( 19.91250000122903074, -4.330127018922190985, -2.500000000000001332 ) ) ;
#9229 = VECTOR ( 'NONE', #24853, 1000.000000000000000 ) ;
#9230 = CARTESIAN_POINT ( 'NONE',  ( 23.99062500061451786, -3.027376345333614438, 5.243569643749998122 ) ) ;
#9231 = CARTESIAN_POINT ( 'NONE',  ( 23.21250000000000213, 2.886751345948126879, 4.999999999999999112 ) ) ;
#9232 = CARTESIAN_POINT ( 'NONE',  ( 27.89062500061451289, 6.054752690667223547, 3.707466751127219781E-16 ) ) ;
#9233 = CARTESIAN_POINT ( 'NONE',  ( 9.065625000614517148, 3.027376345333611329, 5.243569643749999010 ) ) ;
#9234 = EDGE_LOOP ( 'NONE', ( #62532, #61431, #41521, #35208 ) ) ;
#9235 = EDGE_CURVE ( 'NONE', #23877, #58137, #68515, .T. ) ;
#9236 = CARTESIAN_POINT ( 'NONE',  ( 23.84062500061451928, 6.054752690667223547, 3.707466751127219781E-16 ) ) ;
#9237 = CARTESIAN_POINT ( 'NONE',  ( 6.178125000614518747, 6.421520780324663323E-16, -5.243569643749999010 ) ) ;
#9238 = CARTESIAN_POINT ( 'NONE',  ( 13.05937500061451750, 4.119189519843966529, -2.378215178124998275 ) ) ;
#9239 = CARTESIAN_POINT ( 'NONE',  ( 3.928125000614516527, 6.421520780324663323E-16, -5.243569643749999010 ) ) ;
#9240 = CARTESIAN_POINT ( 'NONE',  ( -2.828200636599751609E-16, 14.60000000122903430, -34.61880215351700230 ) ) ;
#9241 = CARTESIAN_POINT ( 'NONE',  ( -2.000000000000000000, 13.62500000000000178, -33.46410161513775705 ) ) ;
#9242 = CARTESIAN_POINT ( 'NONE',  ( 10.12500000000000178, 4.330127018922191873, 2.499999999999999556 ) ) ;
#9243 = CARTESIAN_POINT ( 'NONE',  ( 11.10937500061451644, -4.541064518000417216, -2.621784821875001281 ) ) ;
#9244 = CARTESIAN_POINT ( 'NONE',  ( 6.825000001229034829, -5.773502691896255534, -1.060575238724906372E-15 ) ) ;
#9245 = CARTESIAN_POINT ( 'NONE',  ( 15.30937500061451750, 4.541064518000418104, -2.621784821874998173 ) ) ;
#9246 = CARTESIAN_POINT ( 'NONE',  ( 16.12500000000000000, -4.330127018922194537, 2.499999999999995559 ) ) ;
#9247 = CARTESIAN_POINT ( 'NONE',  ( 7.021875000614518747, -6.054752690667223547, -1.112240025338166033E-15 ) ) ;
#9248 = CARTESIAN_POINT ( 'NONE',  ( -3.000416591977282496E-16, 10.24062500061451608, -34.90005215228797653 ) ) ;
#9249 = DIRECTION ( 'NONE',  ( -1.000000000000000000, -0.000000000000000000, -0.000000000000000000 ) ) ;
#9250 = CARTESIAN_POINT ( 'NONE',  ( 13.32187500061451502, -6.054752690667223547, -1.112240025338166033E-15 ) ) ;
#9251 = CARTESIAN_POINT ( 'NONE',  ( 3.668019400630285531, 3.397886648580393132, 3.993668605712777264 ) ) ;
#9252 = CARTESIAN_POINT ( 'NONE',  ( 22.60312500061451857, 0.000000000000000000, 5.243569643749999010 ) ) ;
#9253 = CARTESIAN_POINT ( 'NONE',  ( -2.498395430326213790E-14, 18.85624999877096641, 26.00000000000000000 ) ) ;
#9254 = DIRECTION ( 'NONE',  ( -0.000000000000000000, -1.000000000000000000, -0.000000000000000000 ) ) ;
#9255 = CARTESIAN_POINT ( 'NONE',  ( 25.88437500061451502, -4.541064518000419881, 2.621784821874995952 ) ) ;
#9256 = LINE ( 'NONE', #37685, #36734 ) ;
#9257 = CARTESIAN_POINT ( 'NONE',  ( 4.378125000614518925, 6.421520780324663323E-16, -5.243569643749999010 ) ) ;
#9258 = CARTESIAN_POINT ( 'NONE',  ( 21.68437500061451573, -2.746126346562646425, 4.756430356249996549 ) ) ;
#9259 = CARTESIAN_POINT ( 'NONE',  ( 13.35937500061451821, -4.541064518000417216, -2.621784821875001281 ) ) ;
#9260 = CARTESIAN_POINT ( 'NONE',  ( 26.13750000122903216, -4.330127018922194537, 2.499999999999995559 ) ) ;
#9261 = CARTESIAN_POINT ( 'NONE',  ( 26.36250000122903003, 4.330127018922192761, -2.499999999999997780 ) ) ;
#9262 = CARTESIAN_POINT ( 'NONE',  ( 6.234375000614519102, 6.421520780324663323E-16, -5.243569643749999010 ) ) ;
#9263 = CARTESIAN_POINT ( 'NONE',  ( 15.45937500061451608, 0.000000000000000000, 5.243569643749999010 ) ) ;
#9264 = CARTESIAN_POINT ( 'NONE',  ( 1.071796769724488785, 17.75134618820329635, 34.00000000000000000 ) ) ;
#9265 = CARTESIAN_POINT ( 'NONE',  ( 24.41250000000000142, 2.886751345948129099, -4.999999999999998224 ) ) ;
#9266 = CARTESIAN_POINT ( 'NONE',  ( 3.712500001229034563, -4.330127018922190985, -2.500000000000001332 ) ) ;
#9267 = CARTESIAN_POINT ( 'NONE',  ( 26.29687500061451644, -3.027376345333614438, 5.243569643749998122 ) ) ;
#9268 = CARTESIAN_POINT ( 'NONE',  ( -1.878215178125001827, 14.40312499938548463, 33.25316411605952283 ) ) ;
#9269 = CARTESIAN_POINT ( 'NONE',  ( 10.01250000000000107, 2.886751345948129099, -4.999999999999997335 ) ) ;
#9270 = CARTESIAN_POINT ( 'NONE',  ( 9.037499999999999645, -2.886751345948125991, -5.000000000000000000 ) ) ;
#9271 = CARTESIAN_POINT ( 'NONE',  ( 8.746875000614515727, -4.119189519843965641, -2.378215178125001383 ) ) ;
#9272 = CARTESIAN_POINT ( 'NONE',  ( 21.29062500061451502, -3.027376345333614438, 5.243569643749998122 ) ) ;
#9273 = CARTESIAN_POINT ( 'NONE',  ( 11.25000000000000000, -4.330127018922190985, -2.500000000000001332 ) ) ;
#9274 = CARTESIAN_POINT ( 'NONE',  ( 4.040625000614517681, 6.054752690667223547, 3.707466751127219781E-16 ) ) ;
#9275 = CARTESIAN_POINT ( 'NONE',  ( 19.42499999999999716, 6.123233995736764310E-16, -4.999999999999998224 ) ) ;
#9276 = EDGE_CURVE ( 'NONE', #20937, #2237, #27968, .T. ) ;
#9277 = CARTESIAN_POINT ( 'NONE',  ( 19.07812500061451644, -4.541064518000419881, 2.621784821874995952 ) ) ;
#9278 = CARTESIAN_POINT ( 'NONE',  ( -3.999999999999999112, 18.72500000122903074, 27.69059892324149885 ) ) ;
#9279 = CARTESIAN_POINT ( 'NONE',  ( 22.61250000122903003, -4.330127018922190985, -2.500000000000001332 ) ) ;
#9280 = CARTESIAN_POINT ( 'NONE',  ( 2.655984681222220721E-16, 19.05312499938548143, 25.66244784525396483 ) ) ;
#9281 = CARTESIAN_POINT ( 'NONE',  ( 29.74687500061451217, 6.054752690667223547, 3.707466751127219781E-16 ) ) ;
#9282 = EDGE_CURVE ( 'NONE', #8125, #8998, #10487, .T. ) ;
#9283 = ORIENTED_EDGE ( 'NONE', *, *, #54421, .F. ) ;
#9284 = CARTESIAN_POINT ( 'NONE',  ( 20.39062500061451644, -3.027376345333614438, 5.243569643749998122 ) ) ;
#9285 = CARTESIAN_POINT ( 'NONE',  ( 23.72812500061451502, 6.421520780324663323E-16, -5.243569643749999010 ) ) ;
#9286 = CARTESIAN_POINT ( 'NONE',  ( 25.02187500061451431, -6.054752690667223547, -1.112240025338166033E-15 ) ) ;
#9287 = CARTESIAN_POINT ( 'NONE',  ( 10.01250000000000107, 2.886751345948129099, -4.999999999999998224 ) ) ;
#9288 = CARTESIAN_POINT ( 'NONE',  ( 11.31562500061451892, 3.027376345333611329, 5.243569643749999010 ) ) ;
#9289 = CARTESIAN_POINT ( 'NONE',  ( 26.50312500061451360, 4.541064518000418104, -2.621784821874998173 ) ) ;
#9290 = CARTESIAN_POINT ( 'NONE',  ( 16.99687500061451573, -3.027376345333610441, -5.243569643749999898 ) ) ;
#9291 = CARTESIAN_POINT ( 'NONE',  ( 9.890625000614516438, 6.054752690667223547, 3.707466751127219781E-16 ) ) ;
#9292 = CARTESIAN_POINT ( 'NONE',  ( 1.999999999999997335, 14.61874999877096570, 33.46410161513775705 ) ) ;
#9293 = CARTESIAN_POINT ( 'NONE',  ( -4.243569643749999898, 18.86562500061451431, 27.54997392385601529 ) ) ;
#9294 = CARTESIAN_POINT ( 'NONE',  ( 24.86250000122903359, -4.330127018922190985, -2.500000000000001332 ) ) ;
#9295 = CARTESIAN_POINT ( 'NONE',  ( 20.14687500061451786, -2.746126346562641984, -4.756430356249999214 ) ) ;
#9296 = CARTESIAN_POINT ( 'NONE',  ( 15.29062500061451502, 6.054752690667223547, 3.707466751127219781E-16 ) ) ;
#9297 = CARTESIAN_POINT ( 'NONE',  ( 8.821875000614518569, -6.054752690667223547, -1.112240025338166033E-15 ) ) ;
#9298 = CARTESIAN_POINT ( 'NONE',  ( 6.609375000614519102, -4.541064518000417216, -2.621784821875001281 ) ) ;
#9299 = EDGE_CURVE ( 'NONE', #27538, #53550, #65663, .T. ) ;
#9300 = ORIENTED_EDGE ( 'NONE', *, *, #55763, .T. ) ;
#9301 = CARTESIAN_POINT ( 'NONE',  ( 29.25937500061451502, 4.541064518000418104, -2.621784821874998173 ) ) ;
#9302 = CARTESIAN_POINT ( 'NONE',  ( 20.65312500061451573, 4.541064518000418104, -2.621784821874998173 ) ) ;
#9303 = CARTESIAN_POINT ( 'NONE',  ( 17.25937500061451502, 0.000000000000000000, 5.243569643749999010 ) ) ;
#9304 = CARTESIAN_POINT ( 'NONE',  ( 21.47812500061451502, 6.421520780324663323E-16, -5.243569643749999010 ) ) ;
#9305 = CARTESIAN_POINT ( 'NONE',  ( -2.000000000000000000, 11.82500000000000107, 26.53589838486224650 ) ) ;
#9306 = CARTESIAN_POINT ( 'NONE',  ( 26.72812500061451502, -4.541064518000419881, 2.621784821874995952 ) ) ;
#9307 = CARTESIAN_POINT ( 'NONE',  ( 7.537500001229033408, 4.330127018922191873, 2.499999999999999556 ) ) ;
#9308 = ORIENTED_EDGE ( 'NONE', *, *, #63007, .T. ) ;
#9309 = CARTESIAN_POINT ( 'NONE',  ( 28.98750000000000071, 5.773502691896255534, 3.535250795749688894E-16 ) ) ;
#9310 = CARTESIAN_POINT ( 'NONE',  ( -1.999999999999997113, 16.92500000000000426, -26.53589838486224295 ) ) ;
#9311 = CARTESIAN_POINT ( 'NONE',  ( 25.95000000122903216, 5.773502691896255534, 3.535250795749688894E-16 ) ) ;
#9312 = CARTESIAN_POINT ( 'NONE',  ( -7.967954043666661671E-16, 14.44062499938548427, 34.33755215474603517 ) ) ;
#9313 = ADVANCED_FACE ( 'NONE', ( #42480 ), #65003, .T. ) ;
#9314 = CARTESIAN_POINT ( 'NONE',  ( 7.246875000614518392, 6.054752690667223547, 3.707466751127219781E-16 ) ) ;
#9315 = CARTESIAN_POINT ( 'NONE',  ( 3.999999999999999112, 15.27500000000000036, 30.00000000000000000 ) ) ;
#9316 = CARTESIAN_POINT ( 'NONE',  ( 14.09062500061451750, -3.027376345333614438, 5.243569643749998122 ) ) ;
#9317 = CARTESIAN_POINT ( 'NONE',  ( 9.609375000614518214, 0.000000000000000000, 5.243569643749999010 ) ) ;
#9318 = CARTESIAN_POINT ( 'NONE',  ( 27.03750000122903430, -4.330127018922194537, 2.499999999999995559 ) ) ;
#9319 = CARTESIAN_POINT ( 'NONE',  ( 17.70937500061451431, 0.000000000000000000, 5.243569643749999010 ) ) ;
#9320 = CARTESIAN_POINT ( 'NONE',  ( 6.234375000614519102, 6.421520780324663323E-16, -5.243569643749999010 ) ) ;
#9321 = CARTESIAN_POINT ( 'NONE',  ( 4.575260086717170438, 2.016679235498957112, 4.840250765194281435 ) ) ;
#9322 = CARTESIAN_POINT ( 'NONE',  ( 5.953125000614519102, 0.000000000000000000, 5.243569643749999010 ) ) ;
#9323 = CARTESIAN_POINT ( 'NONE',  ( 15.17812500061451608, 6.421520780324663323E-16, -5.243569643749999010 ) ) ;
#9324 = ORIENTED_EDGE ( 'NONE', *, *, #68758, .T. ) ;
#9325 = CARTESIAN_POINT ( 'NONE',  ( 12.17812500061451608, 4.541064518000418104, 2.621784821874999949 ) ) ;
#9326 = CARTESIAN_POINT ( 'NONE',  ( 5.850000001229035185, -2.886751345948129988, 4.999999999999997335 ) ) ;
#9327 = CARTESIAN_POINT ( 'NONE',  ( 9.178125000614517859, -4.541064518000419881, 2.621784821874995952 ) ) ;
#9328 = CARTESIAN_POINT ( 'NONE',  ( 22.17187500061451644, 2.746126346562643317, 4.756430356249998326 ) ) ;
#9329 = CARTESIAN_POINT ( 'NONE',  ( 9.074999999999999289, 6.123233995736764310E-16, -4.999999999999998224 ) ) ;
#9330 = CARTESIAN_POINT ( 'NONE',  ( 4.950000001229033941, -2.886751345948129988, 4.999999999999997335 ) ) ;
#9331 = CARTESIAN_POINT ( 'NONE',  ( 18.03749999999999787, -2.886751345948125991, -5.000000000000000000 ) ) ;
#9332 =( BOUNDED_CURVE ( )  B_SPLINE_CURVE ( 2, ( #5890, #55052, #38046, #60571, #32876, #60942, #5534 ),
 .UNSPECIFIED., .F., .F. ) 
 B_SPLINE_CURVE_WITH_KNOTS ( ( 3, 2, 2, 3 ),
 ( 0.4600000000000000200, 0.4633333333333333748, 0.4666666666666667851, 0.4700000000000001399 ),
 .UNSPECIFIED. ) 
 CURVE ( )  GEOMETRIC_REPRESENTATION_ITEM ( )  RATIONAL_B_SPLINE_CURVE ( ( 1.000000000000000000, 0.8660254037844387076, 1.000000000000000000, 0.8660254037844387076, 1.000000000000000000, 0.8660254037844320463, 1.000000000000006661 ) ) 
 REPRESENTATION_ITEM ( '' )  );
#9333 = CARTESIAN_POINT ( 'NONE',  ( 18.42187500061451644, 3.027376345333613106, -5.243569643749998122 ) ) ;
#9334 = CARTESIAN_POINT ( 'NONE',  ( 16.23750000122903359, -4.330127018922194537, 2.499999999999995559 ) ) ;
#9335 = CARTESIAN_POINT ( 'NONE',  ( 21.15000000000000213, -4.330127018922190985, -2.500000000000001332 ) ) ;
#9336 = CARTESIAN_POINT ( 'NONE',  ( -4.243569643749999898, 15.30312500061451608, -30.00000000000000000 ) ) ;
#9337 = CARTESIAN_POINT ( 'NONE',  ( 3.193447721043152665, 3.847322660365763536, 3.562742055761627835 ) ) ;
#9338 = CARTESIAN_POINT ( 'NONE',  ( 1.592000809091587073E-14, 15.05000000122903714, -34.00000000000000000 ) ) ;
#9339 = PLANE ( 'NONE',  #60749 ) ;
#9340 = CARTESIAN_POINT ( 'NONE',  ( 28.22812500061451502, 6.421520780324663323E-16, -5.243569643749999010 ) ) ;
#9341 = FILL_AREA_STYLE_COLOUR ( '', #57528 ) ;
#9342 = CARTESIAN_POINT ( 'NONE',  ( 3.999999999999998668, 14.52500000122903323, 27.69059892324149530 ) ) ;
#9343 = CARTESIAN_POINT ( 'NONE',  ( 17.14687500061451786, 6.054752690667223547, 3.707466751127219781E-16 ) ) ;
#9344 = CARTESIAN_POINT ( 'NONE',  ( 29.58749999999999858, -2.886751345948129988, 4.999999999999997335 ) ) ;
#9345 = CARTESIAN_POINT ( 'NONE',  ( 10.71562500061451928, 3.027376345333613106, -5.243569643749998122 ) ) ;
#9346 = CARTESIAN_POINT ( 'NONE',  ( 7.256250001229033408, -4.330127018922190985, -2.500000000000001332 ) ) ;
#9347 = CARTESIAN_POINT ( 'NONE',  ( 24.64687500061451431, -3.027376345333610441, -5.243569643749999898 ) ) ;
#9348 = CARTESIAN_POINT ( 'NONE',  ( 15.87187500061451573, -4.119189519843968306, 2.378215178124996054 ) ) ;
#9349 = CARTESIAN_POINT ( 'NONE',  ( 8.165625000614516793, 3.027376345333611329, 5.243569643749999010 ) ) ;
#9350 = CARTESIAN_POINT ( 'NONE',  ( 12.60937500061451821, 4.541064518000418104, -2.621784821874998173 ) ) ;
#9351 = VERTEX_POINT ( 'NONE', #43215 ) ;
#9352 = CARTESIAN_POINT ( 'NONE',  ( 24.45937500061451786, 0.000000000000000000, 5.243569643749999010 ) ) ;
#9353 = CARTESIAN_POINT ( 'NONE',  ( 27.77812500061451573, 6.421520780324663323E-16, -5.243569643749999010 ) ) ;
#9354 = DIRECTION ( 'NONE',  ( -1.000000000000000000, -0.000000000000000000, -0.000000000000000000 ) ) ;
#9355 = CARTESIAN_POINT ( 'NONE',  ( 6.750000000000002665, -4.330127018922190985, -2.500000000000001332 ) ) ;
#9356 = CARTESIAN_POINT ( 'NONE',  ( 17.02500000122903145, 2.886751345948126879, 4.999999999999999112 ) ) ;
#9357 = DIRECTION ( 'NONE',  ( -0.000000000000000000, -1.000000000000000000, -0.000000000000000000 ) ) ;
#9358 = CARTESIAN_POINT ( 'NONE',  ( 8.784375000614515372, -2.746126346562642428, -4.756430356249999214 ) ) ;
#9359 = ORIENTED_EDGE ( 'NONE', *, *, #42162, .T. ) ;
#9360 = CARTESIAN_POINT ( 'NONE',  ( 14.66249999999999964, 2.886751345948126879, 4.999999999999999112 ) ) ;
#9361 = CARTESIAN_POINT ( 'NONE',  ( 19.08750000000000213, 5.773502691896255534, 3.535250795749688894E-16 ) ) ;
#9362 = CARTESIAN_POINT ( 'NONE',  ( 10.22812500061451679, 6.421520780324663323E-16, -5.243569643749999010 ) ) ;
#9363 = ORIENTED_EDGE ( 'NONE', *, *, #18203, .T. ) ;
#9364 = CARTESIAN_POINT ( 'NONE',  ( -1.999999999999997113, 11.07500000000000107, -26.53589838486224295 ) ) ;
#9365 = CARTESIAN_POINT ( 'NONE',  ( 4.243569643749999898, 16.89687500061451786, -27.54997392385601529 ) ) ;
#9366 = CARTESIAN_POINT ( 'NONE',  ( 4.340625000614515727, -3.027376345333610441, -5.243569643749999898 ) ) ;
#9367 = CARTESIAN_POINT ( 'NONE',  ( 19.78125000122902932, -4.330127018922194537, 2.499999999999995559 ) ) ;
#9368 = CARTESIAN_POINT ( 'NONE',  ( 9.150000000000002132, 4.330127018922192761, -2.499999999999997780 ) ) ;
#9369 = CARTESIAN_POINT ( 'NONE',  ( 1.626862140677534273E-15, 13.36250000000000071, -26.00000000000000355 ) ) ;
#9370 = VERTEX_POINT ( 'NONE', #25853 ) ;
#9371 = CARTESIAN_POINT ( 'NONE',  ( 4.243569643749999010, 11.96562500061451750, 27.54997392385601174 ) ) ;
#9372 = CARTESIAN_POINT ( 'NONE',  ( 26.42812500061451431, 6.421520780324663323E-16, -5.243569643749999010 ) ) ;
#9373 = CARTESIAN_POINT ( 'NONE',  ( 13.57500000000000107, 6.123233995736764310E-16, -4.999999999999998224 ) ) ;
#9374 = DIRECTION ( 'NONE',  ( 0.000000000000000000, 0.000000000000000000, 1.000000000000000000 ) ) ;
#9375 = CARTESIAN_POINT ( 'NONE',  ( 20.67187500061451289, 3.027376345333613106, -5.243569643749998122 ) ) ;
#9376 = CARTESIAN_POINT ( 'NONE',  ( 18.66562500061451146, -6.054752690667223547, -1.112240025338166033E-15 ) ) ;
#9377 = CARTESIAN_POINT ( 'NONE',  ( 9.001249775931846008E-16, 13.16562500061459140, -25.09994784771203058 ) ) ;
#9378 = CARTESIAN_POINT ( 'NONE',  ( 22.50000000122903288, -2.886751345948129988, 4.999999999999997335 ) ) ;
#9379 =( BOUNDED_CURVE ( )  B_SPLINE_CURVE ( 2, ( #24765, #69489, #41409, #19208, #64292, #52851, #2605, #13679, #36585 ),
 .UNSPECIFIED., .F., .F. ) 
 B_SPLINE_CURVE_WITH_KNOTS ( ( 3, 2, 2, 2, 3 ),
 ( 0.7717391304347825942, 0.7753623188405797118, 0.7826086956521739468, 0.7898550724637680709, 0.7934782608695651884 ),
 .UNSPECIFIED. ) 
 CURVE ( )  GEOMETRIC_REPRESENTATION_ITEM ( )  RATIONAL_B_SPLINE_CURVE ( ( 0.9330127018922194093, 0.9330127018922194093, 1.000000000000000000, 0.8660254037844387076, 1.000000000000000000, 0.8660254037844387076, 1.000000000000000000, 0.9330127018922194093, 0.9330127018922194093 ) ) 
 REPRESENTATION_ITEM ( '' )  );
#9380 = CARTESIAN_POINT ( 'NONE',  ( 3.928125000614516527, 6.421520780324663323E-16, -5.243569643749999010 ) ) ;
#9381 = CARTESIAN_POINT ( 'NONE',  ( 25.92187500061451644, -5.492252693125287522, -1.008910452111647106E-15 ) ) ;
#9382 = CARTESIAN_POINT ( 'NONE',  ( 22.41562500061451502, 3.027376345333612662, -5.243569643749998122 ) ) ;
#9383 = CARTESIAN_POINT ( 'NONE',  ( 8.409375000614518925, -4.119189519843965641, -2.378215178125001383 ) ) ;
#9384 = CARTESIAN_POINT ( 'NONE',  ( -1.878215178125001827, 15.19062499938548427, 33.25316411605952283 ) ) ;
#9386 = EDGE_CURVE ( 'NONE', #64526, #47560, #45612, .T. ) ;
#9385 = CARTESIAN_POINT ( 'NONE',  ( 16.28437500061452070, 4.541064518000418104, 2.621784821874999949 ) ) ;
#9387 = CARTESIAN_POINT ( 'NONE',  ( 17.40937500061451715, -4.541064518000417216, -2.621784821875001281 ) ) ;
#9388 = CARTESIAN_POINT ( 'NONE',  ( 24.38437500061451502, 4.541064518000418104, 2.621784821874999949 ) ) ;
#9389 = CARTESIAN_POINT ( 'NONE',  ( -3.000416591977282496E-16, 13.44687500061451679, 25.09994784771203058 ) ) ;
#9390 = CARTESIAN_POINT ( 'NONE',  ( 4.490625000614516971, 6.054752690667223547, 3.707466751127219781E-16 ) ) ;
#9392 =( BOUNDED_CURVE ( )  B_SPLINE_CURVE ( 2, ( #36518, #63138, #24699, #35067, #8083, #42069, #57593, #1828, #30613 ),
 .UNSPECIFIED., .F., .F. ) 
 B_SPLINE_CURVE_WITH_KNOTS ( ( 3, 2, 2, 2, 3 ),
 ( 0.6413043478260869179, 0.6449275362318840354, 0.6521739130434782705, 0.6594202898550725056, 0.6630434782608696231 ),
 .UNSPECIFIED. ) 
 CURVE ( )  GEOMETRIC_REPRESENTATION_ITEM ( )  RATIONAL_B_SPLINE_CURVE ( ( 0.9330127018922194093, 0.9330127018922194093, 1.000000000000000000, 0.8660254037844387076, 1.000000000000000000, 0.8660254037844387076, 1.000000000000000000, 0.9330127018922182991, 0.9330127018922192983 ) ) 
 REPRESENTATION_ITEM ( '' )  );
#9391 = CARTESIAN_POINT ( 'NONE',  ( 28.04062500061451502, -3.027376345333614438, 5.243569643749998122 ) ) ;
#9393 = CARTESIAN_POINT ( 'NONE',  ( 28.97812500061451502, -4.541064518000419881, 2.621784821874995952 ) ) ;
#9394 = CARTESIAN_POINT ( 'NONE',  ( 1.138803498474273873E-14, 15.08749999999999858, 34.00000000000000000 ) ) ;
#9395 = CARTESIAN_POINT ( 'NONE',  ( 4.000000000000000000, 18.38749999999999929, 32.30940107675849049 ) ) ;
#9396 = CARTESIAN_POINT ( 'NONE',  ( 6.346875000614517148, 6.054752690667223547, 3.707466751127219781E-16 ) ) ;
#9397 = CARTESIAN_POINT ( 'NONE',  ( 15.33750000122903323, -4.330127018922194537, 2.499999999999995559 ) ) ;
#9398 = CARTESIAN_POINT ( 'NONE',  ( 9.900000001229033231, -2.886751345948129988, 4.999999999999997335 ) ) ;
#9399 = CARTESIAN_POINT ( 'NONE',  ( 5.915625000614515905, 3.027376345333611329, 5.243569643749999010 ) ) ;
#9400 = CARTESIAN_POINT ( 'NONE',  ( 4.000000000000000000, 15.63124999877096499, 27.69059892324149530 ) ) ;
#9401 = CARTESIAN_POINT ( 'NONE',  ( 21.73125000122903216, 6.123233995736764310E-16, -4.999999999999998224 ) ) ;
#9402 = CARTESIAN_POINT ( 'NONE',  ( 13.88437500061451679, 6.421520780324663323E-16, -5.243569643749999010 ) ) ;
#9403 = FACE_OUTER_BOUND ( 'NONE', #72136, .T. ) ;
#9404 = ORIENTED_EDGE ( 'NONE', *, *, #43004, .F. ) ;
#9405 = CARTESIAN_POINT ( 'NONE',  ( 21.40312500061451573, -4.541064518000417216, -2.621784821875001281 ) ) ;
#9406 = CARTESIAN_POINT ( 'NONE',  ( 7.453125000614516438, -4.541064518000417216, -2.621784821875001281 ) ) ;
#9407 = CARTESIAN_POINT ( 'NONE',  ( 24.00937500061451502, 0.000000000000000000, 5.243569643749999010 ) ) ;
#9408 = CARTESIAN_POINT ( 'NONE',  ( 8.128125000614515372, 4.541064518000418104, 2.621784821874999949 ) ) ;
#9409 = CARTESIAN_POINT ( 'NONE',  ( 45.00000000000000000, 0.000000000000000000, 0.000000000000000000 ) ) ;
#9410 = CARTESIAN_POINT ( 'NONE',  ( 7.237500001229035362, -4.330127018922194537, 2.499999999999995559 ) ) ;
#9411 = CARTESIAN_POINT ( 'NONE',  ( 21.32812500061451644, -4.541064518000419881, 2.621784821874995952 ) ) ;
#9412 =( BOUNDED_CURVE ( )  B_SPLINE_CURVE ( 2, ( #26642, #38076, #32542, #55080, #4480, #27370, #72063, #21443, #14807 ),
 .UNSPECIFIED., .F., .F. ) 
 B_SPLINE_CURVE_WITH_KNOTS ( ( 3, 2, 2, 2, 3 ),
 ( 0.4305555555555555802, 0.4351851851851851749, 0.4444444444444444198, 0.4537037037037037202, 0.4583333333333333703 ),
 .UNSPECIFIED. ) 
 CURVE ( )  GEOMETRIC_REPRESENTATION_ITEM ( )  RATIONAL_B_SPLINE_CURVE ( ( 0.9330127018922194093, 0.9330127018922197424, 1.000000000000000000, 0.8660254037844387076, 1.000000000000000000, 0.8660254037844387076, 1.000000000000000000, 0.9330127018922189652, 0.9330127018922194093 ) ) 
 REPRESENTATION_ITEM ( '' )  );
#9413 = CARTESIAN_POINT ( 'NONE',  ( -3.999999999999999556, 19.62500000122903643, -32.30940107675850470 ) ) ;
#9414 = CARTESIAN_POINT ( 'NONE',  ( 10.50000000122903465, -2.886751345948125991, -5.000000000000000000 ) ) ;
#9415 = CARTESIAN_POINT ( 'NONE',  ( 20.05312500061451431, -4.541064518000417216, -2.621784821875001281 ) ) ;
#9416 = CARTESIAN_POINT ( 'NONE',  ( 16.79062500061451857, -3.027376345333614438, 5.243569643749998122 ) ) ;
#9417 = CARTESIAN_POINT ( 'NONE',  ( 28.77187500061451431, 2.746126346562645981, -4.756430356249997438 ) ) ;
#9418 = CARTESIAN_POINT ( 'NONE',  ( 19.04999999999999716, 4.330127018922192761, -2.499999999999997780 ) ) ;
#9419 = CARTESIAN_POINT ( 'NONE',  ( 10.23750000122903359, 4.330127018922191873, 2.499999999999999556 ) ) ;
#9420 = EDGE_CURVE ( 'NONE', #40801, #61496, #142, .T. ) ;
#9421 = CARTESIAN_POINT ( 'NONE',  ( 8.278125000614515727, -4.541064518000419881, 2.621784821874995952 ) ) ;
#9422 = CARTESIAN_POINT ( 'NONE',  ( 10.22812500061451679, 6.421520780324663323E-16, -5.243569643749999010 ) ) ;
#9423 = CARTESIAN_POINT ( 'NONE',  ( 22.27500000122903145, 2.886751345948129099, -4.999999999999998224 ) ) ;
#9424 = CARTESIAN_POINT ( 'NONE',  ( 22.50937500061451857, 4.541064518000418104, -2.621784821874998173 ) ) ;
#9425 = CARTESIAN_POINT ( 'NONE',  ( 4.753125000614515372, -4.541064518000417216, -2.621784821875001281 ) ) ;
#9426 = EDGE_CURVE ( 'NONE', #61742, #60154, #35485, .T. ) ;
#9427 = CARTESIAN_POINT ( 'NONE',  ( 5.475000001229035185, -5.773502691896255534, -1.060575238724906372E-15 ) ) ;
#9428 = CARTESIAN_POINT ( 'NONE',  ( 5.821875000614519458, 3.027376345333613106, -5.243569643749998122 ) ) ;
#9429 = CARTESIAN_POINT ( 'NONE',  ( 23.70937500061451786, -4.541064518000417216, -2.621784821875001281 ) ) ;
#9430 = DIRECTION ( 'NONE',  ( -1.000000000000000000, -0.000000000000000000, -0.000000000000000000 ) ) ;
#9431 = CARTESIAN_POINT ( 'NONE',  ( 18.96562500061451573, 3.027376345333611329, 5.243569643749999010 ) ) ;
#9432 = CARTESIAN_POINT ( 'NONE',  ( 24.94687500061451502, -3.027376345333614438, 5.243569643749998122 ) ) ;
#9433 = CARTESIAN_POINT ( 'NONE',  ( -1.878215178125001827, 19.35312499938548214, 33.25316411605952283 ) ) ;
#9434 = CARTESIAN_POINT ( 'NONE',  ( 12.45000000122903394, 5.773502691896255534, 3.535250795749688401E-16 ) ) ;
#9435 = CARTESIAN_POINT ( 'NONE',  ( 11.08125000122903181, 4.330127018922191873, 2.499999999999999556 ) ) ;
#9436 = CARTESIAN_POINT ( 'NONE',  ( 6.234375000614519102, 6.421520780324663323E-16, -5.243569643749999010 ) ) ;
#9437 = CARTESIAN_POINT ( 'NONE',  ( 15.10312500061451502, -4.541064518000417216, -2.621784821875001281 ) ) ;
#9438 = CARTESIAN_POINT ( 'NONE',  ( 12.64687500061451608, 6.054752690667223547, 3.707466751127219781E-16 ) ) ;
#9439 = EDGE_LOOP ( 'NONE', ( #4636, #28828, #41026, #59962 ) ) ;
#9440 = CARTESIAN_POINT ( 'NONE',  ( 22.23750000122903003, 6.123233995736764310E-16, -4.999999999999998224 ) ) ;
#9441 = CARTESIAN_POINT ( 'NONE',  ( 24.85312500061451502, 0.000000000000000000, 5.243569643749999010 ) ) ;
#9442 = CARTESIAN_POINT ( 'NONE',  ( 10.42500000000000071, 6.123233995736764310E-16, -4.999999999999998224 ) ) ;
#9443 = CARTESIAN_POINT ( 'NONE',  ( -1.071796769724479903, 20.46740381056766367, 34.00000000000000000 ) ) ;
#9444 = CARTESIAN_POINT ( 'NONE',  ( 14.24999999999999822, 0.000000000000000000, 4.999999999999998224 ) ) ;
#9445 = CARTESIAN_POINT ( 'NONE',  ( 24.03750000122903430, 6.123233995736764310E-16, -4.999999999999998224 ) ) ;
#9446 = CARTESIAN_POINT ( 'NONE',  ( 19.56562500061451715, -6.054752690667223547, -1.112240025338166033E-15 ) ) ;
#9447 = ORIENTED_EDGE ( 'NONE', *, *, #59745, .F. ) ;
#9448 = CARTESIAN_POINT ( 'NONE',  ( 21.22500000000000142, 6.123233995736764310E-16, -4.999999999999998224 ) ) ;
#9449 = CARTESIAN_POINT ( 'NONE',  ( 23.85937500061451644, 4.541064518000418104, -2.621784821874998173 ) ) ;
#9450 = VERTEX_POINT ( 'NONE', #53554 ) ;
#9451 = CARTESIAN_POINT ( 'NONE',  ( 2.977075986255253159, -4.017098088058328464, -3.370162576270459454 ) ) ;
#9452 = CARTESIAN_POINT ( 'NONE',  ( 11.54062500061451857, -3.027376345333610441, -5.243569643749999898 ) ) ;
#9453 = CARTESIAN_POINT ( 'NONE',  ( 3.853125000614517681, -4.541064518000417216, -2.621784821875001281 ) ) ;
#9454 = CARTESIAN_POINT ( 'NONE',  ( 15.15937500061451537, 2.746126346562645981, -4.756430356249997438 ) ) ;
#9455 = CARTESIAN_POINT ( 'NONE',  ( 27.44062500061451715, 6.054752690667223547, 3.707466751127219781E-16 ) ) ;
#9456 = CARTESIAN_POINT ( 'NONE',  ( 17.28750000000000142, 5.773502691896255534, 3.535250795749688894E-16 ) ) ;
#9457 = CARTESIAN_POINT ( 'NONE',  ( 25.76249999999999929, 2.886751345948129099, -4.999999999999998224 ) ) ;
#9458 = CARTESIAN_POINT ( 'NONE',  ( 1.999999999999998668, 10.85000000000000142, -33.46410161513775705 ) ) ;
#9459 = CARTESIAN_POINT ( 'NONE',  ( 6.159375000614517148, -4.541064518000417216, -2.621784821875001281 ) ) ;
#9460 = CARTESIAN_POINT ( 'NONE',  ( 16.92187500061451999, -6.054752690667223547, -1.112240025338166033E-15 ) ) ;
#9461 = CARTESIAN_POINT ( 'NONE',  ( 26.02499999999999858, -4.330127018922194537, 2.499999999999995559 ) ) ;
#9462 = ORIENTED_EDGE ( 'NONE', *, *, #18001, .F. ) ;
#9463 = CARTESIAN_POINT ( 'NONE',  ( 27.06562500061451004, 3.027376345333611329, 5.243569643749999010 ) ) ;
#9464 = CARTESIAN_POINT ( 'NONE',  ( 28.54687500061451644, -3.027376345333614438, 5.243569643749998122 ) ) ;
#9465 = CARTESIAN_POINT ( 'NONE',  ( 3.271875000614519635, 3.027376345333611329, 5.243569643749999010 ) ) ;
#9466 = CARTESIAN_POINT ( 'NONE',  ( 12.63749999999999929, -2.886751345948125991, -5.000000000000000000 ) ) ;
#9467 = CARTESIAN_POINT ( 'NONE',  ( 12.06562500061451537, 3.027376345333613106, -5.243569643749998122 ) ) ;
#9468 = CARTESIAN_POINT ( 'NONE',  ( 25.85625000122903216, 4.330127018922192761, -2.499999999999997780 ) ) ;
#9469 = CARTESIAN_POINT ( 'NONE',  ( 4.897546610576117843, 1.006994139586731674, -5.145967878999484491 ) ) ;
#9470 = CARTESIAN_POINT ( 'NONE',  ( 28.22812500061451502, 6.421520780324663323E-16, -5.243569643749999010 ) ) ;
#9471 = CARTESIAN_POINT ( 'NONE',  ( 15.26250000122903216, 0.000000000000000000, 4.999999999999998224 ) ) ;
#9472 = CARTESIAN_POINT ( 'NONE',  ( 3.881554241669678884, -3.151751365348489653, -4.190642664303462439 ) ) ;
#9473 = CARTESIAN_POINT ( 'NONE',  ( 16.05937500061451573, -4.119189519843965641, -2.378215178125001383 ) ) ;
#9474 = CARTESIAN_POINT ( 'NONE',  ( 4.978125000614518569, 4.541064518000418104, 2.621784821874999949 ) ) ;
#9475 = CARTESIAN_POINT ( 'NONE',  ( 22.65937500061451715, 0.000000000000000000, 5.243569643749999010 ) ) ;
#9476 = CARTESIAN_POINT ( 'NONE',  ( -2.121784821874999949, 16.63437500061451857, 26.32496088578401938 ) ) ;
#9477 = ADVANCED_FACE ( 'NONE', ( #54299 ), #5865, .T. ) ;
#9478 = CARTESIAN_POINT ( 'NONE',  ( 23.55937500061451573, 0.000000000000000000, 5.243569643749999010 ) ) ;
#9479 = CARTESIAN_POINT ( 'NONE',  ( 5.662500000000000533, 2.886751345948126879, 4.999999999999999112 ) ) ;
#9480 = CARTESIAN_POINT ( 'NONE',  ( 8.484601909799253346E-16, 11.67500000122903359, 34.61880215351700230 ) ) ;
#9481 = CARTESIAN_POINT ( 'NONE',  ( 13.37812500061451715, 6.421520780324663323E-16, -5.243569643749999010 ) ) ;
#9482 = CARTESIAN_POINT ( 'NONE',  ( 5.362500001229033586, 0.000000000000000000, 4.999999999999998224 ) ) ;
#9483 = CARTESIAN_POINT ( 'NONE',  ( 9.721875000614517148, -6.054752690667223547, -1.112240025338166033E-15 ) ) ;
#9484 = CARTESIAN_POINT ( 'NONE',  ( 1.999999999999998668, 15.80000000000000071, -33.46410161513775705 ) ) ;
#9485 = CARTESIAN_POINT ( 'NONE',  ( 9.253125000614517148, -4.541064518000417216, -2.621784821875001281 ) ) ;
#9486 = CARTESIAN_POINT ( 'NONE',  ( 14.85937500061451644, 4.541064518000418104, -2.621784821874998173 ) ) ;
#9487 = CARTESIAN_POINT ( 'NONE',  ( 20.36250000122903359, -4.330127018922190985, -2.500000000000001332 ) ) ;
#9488 = CARTESIAN_POINT ( 'NONE',  ( 10.39687500061451786, 6.054752690667223547, 3.707466751127219781E-16 ) ) ;
#9489 = CARTESIAN_POINT ( 'NONE',  ( 11.69062500061451360, 6.054752690667223547, 3.707466751127219781E-16 ) ) ;
#9490 = CARTESIAN_POINT ( 'NONE',  ( 29.08125000122903003, 4.330127018922191873, 2.499999999999999556 ) ) ;
#9491 = CARTESIAN_POINT ( 'NONE',  ( 20.37187500061451573, 3.027376345333611329, 5.243569643749999010 ) ) ;
#9492 = DIRECTION ( 'NONE',  ( 0.000000000000000000, -0.7071067811865487940, -0.7071067811865464625 ) ) ;
#9493 = FACE_OUTER_BOUND ( 'NONE', #36924, .T. ) ;
#9494 = CARTESIAN_POINT ( 'NONE',  ( 3.189326098586207081, 3.850849880488091515, -3.445552266572465605 ) ) ;
#9495 = CARTESIAN_POINT ( 'NONE',  ( -3.000416591977282496E-16, 14.34687500061451715, -34.90005215228797653 ) ) ;
#9496 = CARTESIAN_POINT ( 'NONE',  ( 15.33750000122903323, -4.330127018922194537, 2.499999999999995559 ) ) ;
#9497 = CARTESIAN_POINT ( 'NONE',  ( 10.88437500061451679, 4.541064518000418104, 2.621784821874999949 ) ) ;
#9498 = CARTESIAN_POINT ( 'NONE',  ( -4.243569643749999898, 18.90312500061451573, -30.00000000000000000 ) ) ;
#9499 = CARTESIAN_POINT ( 'NONE',  ( 16.68750000122903288, -4.330127018922194537, 2.499999999999995559 ) ) ;
#9500 = CARTESIAN_POINT ( 'NONE',  ( 9.853125000614516793, 4.541064518000418104, -2.621784821874998173 ) ) ;
#9501 = ORIENTED_EDGE ( 'NONE', *, *, #16801, .F. ) ;
#9502 = CARTESIAN_POINT ( 'NONE',  ( 16.68750000000000000, -2.886751345948125991, -5.000000000000000000 ) ) ;
#9503 = CARTESIAN_POINT ( 'NONE',  ( 19.12500000122902932, 2.886751345948062486, -5.000000000000113687 ) ) ;
#9504 = CARTESIAN_POINT ( 'NONE',  ( 10.84687500061451715, 6.054752690667223547, 3.707466751127219781E-16 ) ) ;
#9505 = CARTESIAN_POINT ( 'NONE',  ( 0.000000000000000000, 27.50000000000000000, 26.00000000000000000 ) ) ;
#9506 = CARTESIAN_POINT ( 'NONE',  ( 9.675000001229035362, 2.886751345948129099, -4.999999999999998224 ) ) ;
#9507 = CARTESIAN_POINT ( 'NONE',  ( 19.20000000122903572, 5.773502691896255534, 3.535250795749688894E-16 ) ) ;
#9508 = CARTESIAN_POINT ( 'NONE',  ( 15.44062500061451537, -3.027376345333614438, 5.243569643749998122 ) ) ;
#9509 = CARTESIAN_POINT ( 'NONE',  ( 19.45312500061451644, 0.000000000000000000, 5.243569643749999010 ) ) ;
#9510 = CARTESIAN_POINT ( 'NONE',  ( 26.73750000122903003, 6.123233995736764310E-16, -4.999999999999998224 ) ) ;
#9511 = CARTESIAN_POINT ( 'NONE',  ( 2.990625000614519191, -3.027376345333610441, -5.243569643749999898 ) ) ;
#9512 = CARTESIAN_POINT ( 'NONE',  ( 24.14999999999999858, 0.000000000000000000, 4.999999999999998224 ) ) ;
#9513 = CARTESIAN_POINT ( 'NONE',  ( 2.655984681222220721E-16, 14.10312499938548392, 25.66244784525396483 ) ) ;
#9514 = CARTESIAN_POINT ( 'NONE',  ( 26.43750000000000000, -2.886751345948129988, 4.999999999999997335 ) ) ;
#9515 = CARTESIAN_POINT ( 'NONE',  ( 26.03437500061451715, 6.421520780324663323E-16, -5.243569643749999010 ) ) ;
#9516 = DIRECTION ( 'NONE',  ( -1.000000000000000000, -0.000000000000000000, -0.000000000000000000 ) ) ;
#9517 = ADVANCED_FACE ( 'NONE', ( #45034 ), #66468, .T. ) ;
#9518 = CARTESIAN_POINT ( 'NONE',  ( 12.82500000122903394, 2.886751345948129099, -4.999999999999998224 ) ) ;
#9519 = CARTESIAN_POINT ( 'NONE',  ( 3.600000000000002309, -4.330127018922190985, -2.500000000000001332 ) ) ;
#9520 = CARTESIAN_POINT ( 'NONE',  ( 14.69999999999999929, 0.000000000000000000, 4.999999999999998224 ) ) ;
#9521 = CARTESIAN_POINT ( 'NONE',  ( 8.296875000614516438, -3.027376345333614438, 5.243569643749998122 ) ) ;
#9522 = CARTESIAN_POINT ( 'NONE',  ( 25.00312500061451715, -4.541064518000417216, -2.621784821875001281 ) ) ;
#9523 = CARTESIAN_POINT ( 'NONE',  ( 9.243750001229033231, 5.773502691896255534, 3.535250795749688401E-16 ) ) ;
#9524 = CARTESIAN_POINT ( 'NONE',  ( 5.549999999999998934, 4.330127018922192761, -2.499999999999997780 ) ) ;
#9525 = CARTESIAN_POINT ( 'NONE',  ( -2.498395430326213790E-14, 16.66250000000000497, 26.00000000000000000 ) ) ;
#9526 = CARTESIAN_POINT ( 'NONE',  ( 4.209375000614516971, 0.000000000000000000, 5.243569643749999010 ) ) ;
#9527 = CARTESIAN_POINT ( 'NONE',  ( 7.696875000614516793, 6.054752690667223547, 3.707466751127219781E-16 ) ) ;
#9528 = CARTESIAN_POINT ( 'NONE',  ( 5.062500000000000888, 2.886751345948129099, -4.999999999999998224 ) ) ;
#9529 = CARTESIAN_POINT ( 'NONE',  ( 9.001249775931846008E-16, 13.61562500061459602, 34.90005215228797653 ) ) ;
#9530 = CARTESIAN_POINT ( 'NONE',  ( 22.57499999999999929, 6.123233995736764310E-16, -4.999999999999998224 ) ) ;
#9531 = FACE_OUTER_BOUND ( 'NONE', #69545, .T. ) ;
#9532 = CARTESIAN_POINT ( 'NONE',  ( 3.412500000000002309, 2.886751345948126879, 4.999999999999999112 ) ) ;
#9533 = EDGE_LOOP ( 'NONE', ( #13204, #49395, #6349, #33646 ) ) ;
#9534 = CARTESIAN_POINT ( 'NONE',  ( 17.54062500061451502, 6.054752690667223547, 3.707466751127219781E-16 ) ) ;
#9535 = CARTESIAN_POINT ( 'NONE',  ( 11.27812500061451573, 4.541064518000418104, 2.621784821874999949 ) ) ;
#9536 = CARTESIAN_POINT ( 'NONE',  ( 21.04687500061451644, 4.119189519843966529, -2.378215178124998275 ) ) ;
#9537 = CARTESIAN_POINT ( 'NONE',  ( 6.196875000614515905, -3.027376345333610441, -5.243569643749999898 ) ) ;
#9538 = CARTESIAN_POINT ( 'NONE',  ( 22.76249999999999574, 2.886751345948126879, 4.999999999999999112 ) ) ;
#9539 = CARTESIAN_POINT ( 'NONE',  ( 20.51250000122903216, 4.330127018922192761, -2.499999999999997780 ) ) ;
#9540 = CARTESIAN_POINT ( 'NONE',  ( 16.10625000122903216, 0.000000000000000000, 4.999999999999998224 ) ) ;
#9541 = CARTESIAN_POINT ( 'NONE',  ( 9.196875000614518569, -3.027376345333614438, 5.243569643749998122 ) ) ;
#9542 = CARTESIAN_POINT ( 'NONE',  ( 13.20937500061451786, 0.000000000000000000, 5.243569643749999010 ) ) ;
#9543 = CARTESIAN_POINT ( 'NONE',  ( 23.55937500061451573, 0.000000000000000000, 5.243569643749999010 ) ) ;
#9544 = CARTESIAN_POINT ( 'NONE',  ( 5.810221930991193690E-16, 14.80624999877096570, 26.00000000000000000 ) ) ;
#9545 = CARTESIAN_POINT ( 'NONE',  ( 13.12500000000000178, 6.123233995736764310E-16, -4.999999999999998224 ) ) ;
#9546 = CARTESIAN_POINT ( 'NONE',  ( 17.18437500061451573, 4.541064518000418104, 2.621784821874999949 ) ) ;
#9547 = CARTESIAN_POINT ( 'NONE',  ( 8.559375000614515727, 4.541064518000418104, -2.621784821874998173 ) ) ;
#9548 = CARTESIAN_POINT ( 'NONE',  ( 1.878215178125000495, 13.16562499938548392, 26.74683588394047007 ) ) ;
#9549 = CARTESIAN_POINT ( 'NONE',  ( 20.24999999999999645, -4.330127018922190985, -2.500000000000001332 ) ) ;
#9550 = CARTESIAN_POINT ( 'NONE',  ( 4.000000000000000000, 16.13749999999999929, 27.69059892324149530 ) ) ;
#9551 = CARTESIAN_POINT ( 'NONE',  ( -1.999999999999997113, 9.837500001229035007, -26.53589838486224295 ) ) ;
#9552 = CARTESIAN_POINT ( 'NONE',  ( 24.00937500061451502, 0.000000000000000000, 4.756430356249998326 ) ) ;
#9553 = CARTESIAN_POINT ( 'NONE',  ( 12.77812500061451750, -4.541064518000419881, 2.621784821874995952 ) ) ;
#9554 = CARTESIAN_POINT ( 'NONE',  ( 29.33437500061451431, 4.541064518000418104, 2.621784821874999949 ) ) ;
#9555 = CARTESIAN_POINT ( 'NONE',  ( 13.33125000122903359, 4.330127018922191873, 2.499999999999999556 ) ) ;
#9556 = CARTESIAN_POINT ( 'NONE',  ( 0.000000000000000000, 20.00000000000000000, -33.99999999999999289 ) ) ;
#9557 = CARTESIAN_POINT ( 'NONE',  ( 12.78749999999999964, 5.773502691896255534, 3.535250795749688894E-16 ) ) ;
#9558 = EDGE_CURVE ( 'NONE', #54392, #54059, #19640, .T. ) ;
#9559 = CARTESIAN_POINT ( 'NONE',  ( 3.999999999999999112, 18.53750000122903430, 30.00000000000000000 ) ) ;
#9560 = CARTESIAN_POINT ( 'NONE',  ( 11.32500000122903394, -5.773502691896255534, -1.060575238724906372E-15 ) ) ;
#9561 = CARTESIAN_POINT ( 'NONE',  ( 21.38437500061451502, -4.541064518000419881, 2.621784821874995952 ) ) ;
#9562 = CARTESIAN_POINT ( 'NONE',  ( 16.24687500061451573, 6.054752690667223547, 3.707466751127219781E-16 ) ) ;
#9563 = DIRECTION ( 'NONE',  ( -0.000000000000000000, -1.000000000000000000, -0.000000000000000000 ) ) ;
#9564 = ORIENTED_EDGE ( 'NONE', *, *, #43169, .T. ) ;
#9565 = CARTESIAN_POINT ( 'NONE',  ( 17.54062500061451502, 6.054752690667223547, 3.707466751127219781E-16 ) ) ;
#9566 = CARTESIAN_POINT ( 'NONE',  ( 27.71250000122903145, 4.330127018922192761, -2.499999999999997780 ) ) ;
#9567 = CARTESIAN_POINT ( 'NONE',  ( 17.33437500061451431, -4.541064518000419881, 2.621784821874995952 ) ) ;
#9568 = CARTESIAN_POINT ( 'NONE',  ( 3.590625000614518836, 6.054752690667223547, 3.707466751127219781E-16 ) ) ;
#9569 = CARTESIAN_POINT ( 'NONE',  ( 20.20312500061451644, 4.541064518000418104, -2.621784821874998173 ) ) ;
#9570 = CARTESIAN_POINT ( 'NONE',  ( 3.999999999999999112, 18.42500000000000071, -30.00000000000000000 ) ) ;
#9571 = CARTESIAN_POINT ( 'NONE',  ( 27.79687500061451999, -3.027376345333610441, -5.243569643749999898 ) ) ;
#9572 = CARTESIAN_POINT ( 'NONE',  ( 2.121784821875001281, 12.30312500061451608, 33.67503911421598417 ) ) ;
#9573 = CARTESIAN_POINT ( 'NONE',  ( 17.06250000122903288, 0.000000000000000000, 4.999999999999998224 ) ) ;
#9574 = CARTESIAN_POINT ( 'NONE',  ( 10.95937500061451964, 0.000000000000000000, 4.756430356249998326 ) ) ;
#9575 = CARTESIAN_POINT ( 'NONE',  ( 26.16562500061451502, 3.027376345333611329, 5.243569643749999010 ) ) ;
#9576 = CARTESIAN_POINT ( 'NONE',  ( 3.999999999999998668, 18.70624999877096784, 32.30940107675850470 ) ) ;
#9577 = CARTESIAN_POINT ( 'NONE',  ( 19.73437500061451644, 6.421520780324663323E-16, -5.243569643749999010 ) ) ;
#9578 = CARTESIAN_POINT ( 'NONE',  ( 22.12500000122903288, -5.773502691896255534, -1.060575238724906372E-15 ) ) ;
#9579 = CARTESIAN_POINT ( 'NONE',  ( 22.94062500061451715, 6.054752690667223547, 3.707466751127219781E-16 ) ) ;
#9580 = CARTESIAN_POINT ( 'NONE',  ( 18.12187500061451573, 3.027376345333611329, 5.243569643749999010 ) ) ;
#9581 = CARTESIAN_POINT ( 'NONE',  ( 11.46562500061451573, -6.054752690667223547, -1.112240025338166033E-15 ) ) ;
#9582 = CARTESIAN_POINT ( 'NONE',  ( 4.243569643749999898, 15.13437500061451679, 30.00000000000000000 ) ) ;
#9583 = CARTESIAN_POINT ( 'NONE',  ( 17.31562500061451715, -6.054752690667223547, -1.112240025338166033E-15 ) ) ;
#9584 = CARTESIAN_POINT ( 'NONE',  ( 10.05000000000000071, 4.330127018922192761, -2.499999999999997780 ) ) ;
#9585 = VERTEX_POINT ( 'NONE', #22484 ) ;
#9586 = ORIENTED_EDGE ( 'NONE', *, *, #68789, .F. ) ;
#9587 = CARTESIAN_POINT ( 'NONE',  ( 22.46250000000000213, -5.773502691896255534, -1.060575238724906372E-15 ) ) ;
#9588 = CARTESIAN_POINT ( 'NONE',  ( 4.243569643749999898, 18.24687500061451928, -27.54997392385601529 ) ) ;
#9589 = CARTESIAN_POINT ( 'NONE',  ( 13.23750000122903359, 6.123233995736764310E-16, -4.999999999999998224 ) ) ;
#9590 = CARTESIAN_POINT ( 'NONE',  ( 23.99062500061451786, -3.027376345333614438, 5.243569643749998122 ) ) ;
#9591 = CARTESIAN_POINT ( 'NONE',  ( 6.328125000614515550, 4.541064518000418104, 2.621784821874999949 ) ) ;
#9592 = CARTESIAN_POINT ( 'NONE',  ( 16.53750000122903430, 4.330127018922191873, 2.499999999999999556 ) ) ;
#9593 = CARTESIAN_POINT ( 'NONE',  ( 21.32812500061451644, -4.541064518000419881, 2.621784821874995952 ) ) ;
#9594 = CARTESIAN_POINT ( 'NONE',  ( 22.19999999999999574, 4.330127018922192761, -2.499999999999997780 ) ) ;
#9595 = CARTESIAN_POINT ( 'NONE',  ( 26.91562500061451146, 3.027376345333613106, -5.243569643749998122 ) ) ;
#9596 = CARTESIAN_POINT ( 'NONE',  ( 7.115625000614516082, 3.027376345333613106, -5.243569643749998122 ) ) ;
#9597 = VERTEX_POINT ( 'NONE', #39863 ) ;
#9598 = PRODUCT ( 'spindle', 'spindle', '', ( #20087 ) ) ;
#9599 = CARTESIAN_POINT ( 'NONE',  ( 24.29062500061451502, 6.054752690667223547, 3.707466751127219781E-16 ) ) ;
#9600 = CARTESIAN_POINT ( 'NONE',  ( 5.128125000614516260, -4.541064518000419881, 2.621784821874995952 ) ) ;
#9601 = CARTESIAN_POINT ( 'NONE',  ( 11.93437500061451573, -4.119189519843968306, 2.378215178124996054 ) ) ;
#9602 = CARTESIAN_POINT ( 'NONE',  ( 4.340625000614515727, -3.027376345333610441, -5.243569643749999898 ) ) ;
#9603 = CARTESIAN_POINT ( 'NONE',  ( 4.000000000000000000, 13.55000000122903359, -27.69059892324149530 ) ) ;
#9604 = CARTESIAN_POINT ( 'NONE',  ( -1.999999999999997113, 10.62500000000000000, -26.53589838486224295 ) ) ;
#9605 = AXIS2_PLACEMENT_3D ( 'NONE', #21651, #55287, #49016 ) ;
#9606 = CARTESIAN_POINT ( 'NONE',  ( 10.01250000000000107, 2.886751345948129099, -4.999999999999998224 ) ) ;
#9607 =( BOUNDED_SURFACE ( )  B_SPLINE_SURFACE ( 1, 2, ( 
 ( #36345, #19330, #48531, #24884, #64413, #41885, #58860, #2731, #48162, #8270, #30800, #13072, #18966, #37067, #7903, #70325, #25246, #53703, #47795, #20062, #69605, #58494, #14168, #13424, #35611, #19701, #25992, #53333, #42254, #52609, #13806, #42618, #64777, #70687, #36702, #59224, #8632, #41173, #58131, #2366, #3472, #18608, #3096, #47070, #31161, #30441, #35974, #25625, #52970, #65142, #14533, #59591, #41526, #63682, #64045, #7537, #9004, #31536, #54076, #30070, #2015, #47429, #24526, #69960, #40248, #69416, #1097, #23605, #52054, #17687, #63847, #35058, #63129, #50967, #46150, #12525, #62769, #57585, #6988, #23964, #6632, #29519, #363, #28789, #18771, #12160, #51693, #34688, #28430, #39894, #40608, #45792, #1458, #46512, #68327, #29161, #23241, #56855, #69051, #57219, #18413, #35415, #57940, #5897, #40979, #68690, #22870, #18050, #17335, #24328, #6261, #56504, #63494, #12882, #7347, #51330, #29877, #45428, #67962, #41337, #52413, #1821, #62407, #46877, #11806, #13238, #34323, #732, #59763, #37242, #65680, #35776, #64212, #25053, #58299, #3637, #48700, #42787, #19873, #26161, #7708, #53502, #30606, #47968, #19503, #71223, #2894, #25425, #31337, #70125, #43160, #70496, #20235, #20601, #42426, #2533, #48336, #53134, #30242, #53878, #3270, #64947, #25798, #65308, #14339, #52775, #70861, #2177, #13601, #36873, #24690, #47596, #59391, #14698, #42060, #8801, #36509, #9170, #64583, #30967, #13971, #31705, #47234, #54240, #69767, #19135, #41689, #59029, #36147, #8431, #58666, #8074, #26905, #38336, #27629, #60491, #27266, #10268, #9897, #33513, #32801, #4376, #54602, #44633, #21704, #44261, #5093, #21339, #60865, #71965, #44982, #22074, #55337, #15426, #60127, #66794, #61237, #26530, #56062, #61592, #32070, #50162, #49431, #4732, #5455, #66418, #49799, #72692, #32433, #67162, #20973, #27995, #9536, #43894, #72324, #54970, #16523, #4007, #49070, #50524, #39075, #15796, #16165, #10993, #55699, #15068, #10631, #73052, #22434, #38717, #33161, #37605, #71598, #43526, #66048, #37970, #51610, #23880, #34602, #6541, #61958, #67877, #12795, #56771, #46067, #1010, #29434, #23517, #68965, #45343, #34237, #63040, #62325, #11362, #68602, #1730, #57131, #29075, #28345, #17606, #18322, #17963, #46427, #40524, #40166, #12081, #16884, #33880, #51244, #52328, #67519, #51971, #22790, #12439, #6175, #11721, #57501, #28705, #40895, #62685, #34972, #17249, #24243, #39809, #56425, #6903, #1370, #63409, #39438, #35331, #647, #5814, #57854, #23155, #50882, #7263, #282, #45709, #68243, #29792, #41251, #36427, #9086, #69684, #47883, #42702, #58941, #13512, #59304, #64126, #31623, #42339, #14250, #8349, #64862, #31247, #53419, #63762, #36789, #13151, #24604, #30878, #35693, #36059, #2810, #3184, #7987, #25338, #47512, #53788, #58579, #41974, #30523, #19788, #54157, #8715, #25711, #70772, #48248, #53050, #20148, #19414, #65224, #3553, #2444, #70041, #14614, #19049, #70412, #64495, #41607, #37153, #59678, #58213, #13887, #46792, #24967, #69328, #18687, #7618, #30154, #52688, #2094, #47152, #39990, #60405, #21254, #4290, #71139, #9454, #10184, #15345, #55256, #16081, #37885, #49350, #65965, #26444, #27181, #32346, #38630, #5012, #27546, #48614, #66708, #43807, #65595, #66332, #60043, #68064, #48984, #26075, #33078, #61154, #4652, #71513, #9814, #20512, #43069, #11901, #10549, #60777, #14984, #50078, #31984, #55616, #54884, #26816, #465, #22973, #56954, #37522, #54518, #71881, #3921, #17432, #62503, #45535, #32719, #34426, #20889, #15710, #43443, #38248, #49715, #72243, #21620, #44178, #1921, #40709, #13704, #69152, #63948, #69864, #18511, #18142, #29614, #46246, #6725, #7444, #12621, #69510, #58395, #7808, #28890, #46975, #24063, #45888, #1553, #40341, #47331, #29259, #6358, #13333, #18870, #35515, #51789, #63227, #831, #51429, #64314, #41432, #41076, #23339, #30345, #12257, #35871, #35156, #68786, #52873, #2271, #36247, #68420, #34788, #57680, #17782, #19230, #41784, #24787, #63590, #62862, #57321, #46609, #1190, #12978, #7085, #23698, #58034, #29970, #24426, #52150, #52511, #48437, #43262, #49173, #70962, #25524, #71329, #2996, #43627, #54344, #26263, #20335, #3738, #65783, #65411, #53231, #48800, #25150, #36607, #42888, #2628, #48067, #14801, #15165, #19968, #37344, #59494, #37702, #70593, #53978, #42521, #31806, #21076, #20704, #60223, #9637, #32171, #65047, #54704, #31438, #4109, #66149, #14437, #8907, #26637, #31064, #59867, #3376, #53602, #9271, #71704, #47690, #25897, #15527, #36971, #58761, #8171, #30699, #70226, #19600, #42156, #64683, #14068, #59128, #8535, #16263, #10002, #21437, #22175, #27365, #67263, #28094, #45080, #55439, #33263, #49896, #11091, #377, #33619, #56163, #62064, #5557, #21804, #50622, #10731, #27, #45443, #72421, #61333, #22533 ),
 ( #50980, #44368, #55801, #38818, #32537, #43994, #44728, #66895, #16621, #67616, #5191, #27729, #4831, #38443, #39176, #50267, #16982, #39539, #11458, #60593, #33979, #72792, #4474, #61692, #72058, #5911, #60969, #38069, #56518, #28445, #22885, #10369, #67976, #55074, #27004, #49534, #66516, #15896, #32899, #69430, #23255, #46892, #46164, #6647, #41352, #18787, #47250, #17349, #45805, #29174, #39908, #58313, #30258, #24344, #1473, #7724, #62421, #35073, #12175, #29533, #1111, #52791, #57599, #7002, #12897, #51708, #24706, #52068, #1836, #2192, #23979, #57232, #29891, #34703, #11820, #35430, #57954, #46527, #7362, #63862, #69069, #34337, #52430, #56871, #68341, #18428, #6275, #23618, #40994, #13252, #68704, #63510, #18064, #40625, #35790, #17701, #28803, #51344, #63144, #746, #12539, #40262, #62783, #13617, #32086, #9187, #42077, #70514, #31722, #37259, #69783, #42804, #60143, #3654, #14356, #19890, #26548, #2912, #42443, #64965, #36891, #53896, #26177, #59410, #8818, #64228, #70141, #15084, #59045, #48353, #3287, #54258, #25815, #71240, #47611, #36525, #65326, #64599, #36162, #70878, #4023, #31355, #20252, #30620, #14717, #20620, #59781, #48718, #43178, #65697, #37621, #19150, #58680, #53518, #54617, #41704, #9552, #25068, #8090, #8449, #13986, #53150, #30985, #2549, #19519, #25443, #47986, #5830, #49447, #43543, #61610, #16540, #11011, #71617, #56082, #21354, #60508, #44649, #71981, #9914, #28013, #56440, #15812, #49089, #22091, #66064, #38733, #11377, #43910, #50180, #44999, #61253, #67536, #44279, #38354, #15442, #5474, #55715, #5110, #39093, #55354, #21720, #32816, #20990, #50541, #72339, #66434, #37986, #27644, #67179, #32452, #16899, #22450, #54987, #33532, #60881, #66810, #39454, #27282, #10647, #73069, #10286, #16182, #61975, #49815, #33177, #33896, #4748, #4393, #26922, #72708, #22807, #12097, #12459, #23171, #29811, #45359, #67893, #63782, #40914, #663, #29092, #63427, #68983, #28362, #1388, #18706, #35348, #46084, #51628, #58233, #34618, #1028, #23534, #68620, #34990, #57872, #17982, #40541, #17265, #28720, #46811, #17623, #6920, #57519, #12814, #29450, #52346, #6192, #68260, #23897, #45725, #39827, #51987, #35711, #63057, #46445, #62342, #18340, #1749, #7282, #24262, #69348, #41270, #13171, #50898, #11737, #57148, #298, #34254, #56787, #51261, #40182, #62703, #6560, #70793, #24987, #9105, #2830, #30897, #36079, #37540, #8007, #2113, #20168, #48269, #42722, #30176, #14632, #53069, #19069, #3203, #30542, #41625, #59698, #15003, #47532, #7638, #53809, #24624, #70432, #43087, #2464, #8733, #3572, #19807, #26095, #25358, #70060, #47171, #37172, #14270, #36808, #65243, #13908, #53439, #64515, #52707, #31643, #47903, #19434, #69703, #59323, #25731, #64145, #48633, #54175, #13532, #71158, #65614, #58600, #20530, #41995, #36447, #58961, #8369, #42360, #64882, #31267, #55273, #10200, #15364, #16820, #60424, #54538, #72626, #27564, #22010, #9473, #67096, #32364, #71533, #55633, #9835, #20908, #39012, #67457, #26835, #60062, #33094, #3940, #49733, #22369, #54902, #61171, #55996, #72260, #5389, #4668, #49369, #26463, #16454, #66726, #16097, #50095, #66350, #32736, #43826, #32003, #61527, #27198, #4310, #49002, #38647, #5026, #43460, #27927, #33452, #65984, #44566, #71899, #21637, #50460, #38267, #44195, #10925, #21272, #72987, #37906, #44921, #15728, #60795, #10566, #34173, #40825, #33818, #56362, #1664, #51902, #11658, #40103, #1300, #6835, #39374, #12369, #29723, #46361, #57066, #62616, #69260, #45645, #12013, #34536, #6473, #23454, #68895, #29008, #51545, #5752, #39745, #57786, #28641, #17897, #45999, #23810, #68536, #63342, #17185, #6110, #34904, #56709, #28286, #40457, #46725, #946, #62973, #220, #57431, #12728, #29370, #18252, #35264, #7195, #52261, #61893, #50817, #23088, #24173, #11298, #68179, #22725, #45278, #67811, #62261, #51179, #583, #17541, #13087, #18980, #37081, #7917, #70338, #25262, #53717, #47809, #20075, #69618, #58507, #14181, #13439, #35625, #19715, #26005, #58872, #53345, #52623, #41899, #42631, #42267, #48176, #64790, #64426, #36358, #41187, #58145, #2379, #3487, #18622, #3109, #47084, #36715, #30454, #35989, #8645, #52983, #65155, #13818, #8282, #41541, #48544, #64059, #7551, #31174, #59237, #25638, #63696, #70700, #24897, #30085, #14545, #47442, #2029, #59605, #24540, #69974, #19344, #9019, #30812, #2743, #54089, #31549, #72170, #67007, #60701, #16368, #66258, #60335, #37455, #27475, #4580, #27110, #61079, #4218, #43734, #54812, #27845, #4941, #21182, #71442, #42996, #49643, #44104, #9383, #38923, #44476, #14913, #33006, #9744, #15636, #61442, #49279, #32644, #10477, #65896, #55545, #3850, #10835, #65527, #26746, #55185, #15276, #72532, #59974, #31915, #33371, #50007, #43372, #71812, #21920, #38556, #71071 ) ),
 .UNSPECIFIED., .F., .F., .F. ) 
 B_SPLINE_SURFACE_WITH_KNOTS ( ( 2, 2 ),
 ( 3, 2, 2, 2, 2, 2, 2, 2, 2, 2, 2, 2, 2, 2, 2, 2, 2, 2, 2, 2, 2, 2, 2, 2, 2, 2, 2, 2, 2, 2, 2, 2, 2, 2, 2, 2, 2, 2, 2, 2, 2, 2, 2, 2, 2, 2, 2, 2, 2, 2, 2, 2, 2, 2, 2, 2, 2, 2, 2, 2, 2, 2, 2, 2, 2, 2, 2, 2, 2, 2, 2, 2, 2, 2, 2, 2, 2, 2, 2, 2, 2, 2, 2, 2, 2, 2, 2, 2, 2, 2, 2, 2, 2, 2, 2, 2, 2, 2, 2, 2, 2, 2, 2, 2, 2, 2, 2, 2, 2, 2, 2, 2, 2, 2, 2, 2, 2, 2, 2, 2, 2, 2, 2, 2, 2, 2, 2, 2, 2, 2, 2, 2, 2, 2, 2, 2, 2, 2, 2, 2, 2, 2, 2, 2, 2, 2, 2, 2, 2, 2, 2, 2, 2, 2, 2, 2, 2, 2, 2, 2, 2, 2, 2, 2, 2, 2, 2, 2, 2, 2, 2, 2, 2, 2, 2, 2, 2, 2, 2, 2, 2, 2, 2, 2, 2, 2, 2, 2, 2, 2, 2, 2, 2, 2, 2, 2, 2, 2, 2, 2, 2, 2, 2, 2, 2, 2, 2, 2, 2, 2, 2, 2, 2, 2, 2, 2, 2, 2, 2, 2, 2, 2, 2, 2, 2, 2, 2, 2, 2, 2, 2, 2, 2, 2, 2, 2, 2, 2, 2, 2, 2, 2, 2, 2, 2, 2, 2, 2, 2, 2, 2, 2, 2, 2, 2, 2, 2, 2, 2, 2, 2, 2, 2, 2, 2, 2, 2, 2, 2, 2, 2, 2, 2, 2, 2, 2, 2, 2, 2, 2, 2, 2, 2, 2, 2, 2, 2, 2, 2, 2, 2, 2, 2, 2, 2, 2, 2, 2, 2, 2, 3 ),
 ( 0.000000000000000000, 1.000000000000000000 ),
 ( 0.000000000000000000, 0.003333333333333333547, 0.006666666666666667095, 0.01000000000000000021, 0.01333333333333333419, 0.01666666666666666644, 0.02000000000000000042, 0.02333333333333333440, 0.02666666666666666838, 0.02999999999999999889, 0.03333333333333333287, 0.03666666666666666685, 0.04000000000000000083, 0.04333333333333333481, 0.04666666666666666879, 0.05000000000000000278, 0.05333333333333333676, 0.05666666666666666380, 0.05999999999999999778, 0.06333333333333333870, 0.06666666666666666574, 0.07000000000000000666, 0.07333333333333333370, 0.07666666666666666075, 0.08000000000000000167, 0.08333333333333332871, 0.08666666666666666963, 0.08999999999999999667, 0.09333333333333333759, 0.09666666666666666463, 0.1000000000000000056, 0.1033333333333333326, 0.1066666666666666735, 0.1100000000000000006, 0.1133333333333333276, 0.1166666666666666685, 0.1199999999999999956, 0.1233333333333333365, 0.1266666666666666774, 0.1300000000000000044, 0.1333333333333333315, 0.1366666666666666585, 0.1400000000000000133, 0.1433333333333333404, 0.1466666666666666674, 0.1499999999999999944, 0.1533333333333333215, 0.1566666666666666763, 0.1600000000000000033, 0.1633333333333333304, 0.1666666666666666574, 0.1700000000000000122, 0.1733333333333333393, 0.1766666666666666663, 0.1799999999999999933, 0.1833333333333333204, 0.1866666666666666752, 0.1900000000000000022, 0.1933333333333333293, 0.1966666666666666563, 0.2000000000000000111, 0.2033333333333333381, 0.2066666666666666652, 0.2099999999999999922, 0.2133333333333333470, 0.2166666666666666741, 0.2200000000000000011, 0.2233333333333333282, 0.2266666666666666552, 0.2300000000000000100, 0.2333333333333333370, 0.2366666666666666641, 0.2399999999999999911, 0.2433333333333333459, 0.2466666666666666730, 0.2500000000000000000, 0.2533333333333333548, 0.2566666666666666541, 0.2600000000000000089, 0.2633333333333333082, 0.2666666666666666630, 0.2700000000000000178, 0.2733333333333333171, 0.2766666666666666718, 0.2800000000000000266, 0.2833333333333333259, 0.2866666666666666807, 0.2899999999999999800, 0.2933333333333333348, 0.2966666666666666896, 0.2999999999999999889, 0.3033333333333333437, 0.3066666666666666430, 0.3099999999999999978, 0.3133333333333333526, 0.3166666666666666519, 0.3200000000000000067, 0.3233333333333333059, 0.3266666666666666607, 0.3300000000000000155, 0.3333333333333333148, 0.3366666666666666696, 0.3400000000000000244, 0.3433333333333333237, 0.3466666666666666785, 0.3499999999999999778, 0.3533333333333333326, 0.3566666666666666874, 0.3599999999999999867, 0.3633333333333333415, 0.3666666666666666408, 0.3699999999999999956, 0.3733333333333333504, 0.3766666666666666496, 0.3800000000000000044, 0.3833333333333333592, 0.3866666666666666585, 0.3900000000000000133, 0.3933333333333333126, 0.3966666666666666674, 0.4000000000000000222, 0.4033333333333333215, 0.4066666666666666763, 0.4099999999999999756, 0.4133333333333333304, 0.4166666666666666852, 0.4199999999999999845, 0.4233333333333333393, 0.4266666666666666941, 0.4299999999999999933, 0.4333333333333333481, 0.4366666666666666474, 0.4400000000000000022, 0.4433333333333333570, 0.4466666666666666563, 0.4500000000000000111, 0.4533333333333333104, 0.4566666666666666652, 0.4600000000000000200, 0.4633333333333333193, 0.4666666666666666741, 0.4699999999999999734, 0.4733333333333333282, 0.4766666666666666829, 0.4799999999999999822, 0.4833333333333333370, 0.4866666666666666918, 0.4899999999999999911, 0.4933333333333333459, 0.4966666666666666452, 0.5000000000000000000, 0.5033333333333332993, 0.5066666666666667096, 0.5100000000000000089, 0.5133333333333333082, 0.5166666666666667185, 0.5200000000000000178, 0.5233333333333333171, 0.5266666666666666163, 0.5300000000000000266, 0.5333333333333333259, 0.5366666666666666252, 0.5400000000000000355, 0.5433333333333333348, 0.5466666666666666341, 0.5500000000000000444, 0.5533333333333333437, 0.5566666666666666430, 0.5600000000000000533, 0.5633333333333333526, 0.5666666666666666519, 0.5699999999999999512, 0.5733333333333333615, 0.5766666666666666607, 0.5799999999999999600, 0.5833333333333333703, 0.5866666666666666696, 0.5899999999999999689, 0.5933333333333333792, 0.5966666666666666785, 0.5999999999999999778, 0.6033333333333333881, 0.6066666666666666874, 0.6099999999999999867, 0.6133333333333332860, 0.6166666666666666963, 0.6199999999999999956, 0.6233333333333332948, 0.6266666666666667052, 0.6300000000000000044, 0.6333333333333333037, 0.6366666666666667140, 0.6400000000000000133, 0.6433333333333333126, 0.6466666666666666119, 0.6500000000000000222, 0.6533333333333333215, 0.6566666666666666208, 0.6600000000000000311, 0.6633333333333333304, 0.6666666666666666297, 0.6700000000000000400, 0.6733333333333333393, 0.6766666666666666385, 0.6800000000000000488, 0.6833333333333333481, 0.6866666666666666474, 0.6899999999999999467, 0.6933333333333333570, 0.6966666666666666563, 0.6999999999999999556, 0.7033333333333333659, 0.7066666666666666652, 0.7099999999999999645, 0.7133333333333333748, 0.7166666666666666741, 0.7199999999999999734, 0.7233333333333333837, 0.7266666666666666829, 0.7299999999999999822, 0.7333333333333332815, 0.7366666666666666918, 0.7399999999999999911, 0.7433333333333332904, 0.7466666666666667007, 0.7500000000000000000, 0.7533333333333332993, 0.7566666666666667096, 0.7600000000000000089, 0.7633333333333333082, 0.7666666666666667185, 0.7700000000000000178, 0.7733333333333333171, 0.7766666666666666163, 0.7800000000000000266, 0.7833333333333333259, 0.7866666666666666252, 0.7900000000000000355, 0.7933333333333333348, 0.7966666666666666341, 0.8000000000000000444, 0.8033333333333333437, 0.8066666666666666430, 0.8100000000000000533, 0.8133333333333333526, 0.8166666666666666519, 0.8199999999999999512, 0.8233333333333333615, 0.8266666666666666607, 0.8299999999999999600, 0.8333333333333333703, 0.8366666666666666696, 0.8399999999999999689, 0.8433333333333333792, 0.8466666666666666785, 0.8499999999999999778, 0.8533333333333333881, 0.8566666666666666874, 0.8599999999999999867, 0.8633333333333332860, 0.8666666666666666963, 0.8699999999999999956, 0.8733333333333332948, 0.8766666666666667052, 0.8800000000000000044, 0.8833333333333333037, 0.8866666666666667140, 0.8900000000000000133, 0.8933333333333333126, 0.8966666666666666119, 0.9000000000000000222, 0.9033333333333333215, 0.9066666666666666208, 0.9100000000000000311, 0.9133333333333333304, 0.9166666666666666297, 0.9200000000000000400, 0.9233333333333333393, 0.9266666666666666385, 0.9300000000000000488, 0.9333333333333333481, 0.9366666666666666474, 0.9399999999999999467, 0.9433333333333333570, 0.9466666666666666563, 0.9499999999999999556, 0.9533333333333333659, 0.9566666666666666652, 0.9599999999999999645, 0.9633333333333333748, 0.9666666666666666741, 0.9699999999999999734, 0.9733333333333333837, 0.9766666666666666829, 0.9799999999999999822, 0.9833333333333332815, 0.9866666666666666918, 0.9899999999999999911, 0.9933333333333332904, 0.9966666666666667007, 1.000000000000000000 ),
 .UNSPECIFIED. ) 
 GEOMETRIC_REPRESENTATION_ITEM ( )  RATIONAL_B_SPLINE_SURFACE ( (
 ( 1.000000000000000000, 0.8660254037844387076, 1.000000000000000000, 0.8660254037844387076, 1.000000000000000000, 0.8660254037844387076, 1.000000000000000000, 0.8660254037844387076, 1.000000000000000000, 0.8660254037844387076, 1.000000000000000000, 0.8660254037844387076, 1.000000000000000000, 0.8660254037844387076, 1.000000000000000000, 0.8660254037844387076, 1.000000000000000000, 0.8660254037844387076, 1.000000000000000000, 0.8660254037844387076, 1.000000000000000000, 0.8660254037844387076, 1.000000000000000000, 0.8660254037844387076, 1.000000000000000000, 0.8660254037844387076, 1.000000000000000000, 0.8660254037844387076, 1.000000000000000000, 0.8660254037844387076, 1.000000000000000000, 0.8660254037844387076, 1.000000000000000000, 0.8660254037844387076, 1.000000000000000000, 0.8660254037844387076, 1.000000000000000000, 0.8660254037844387076, 1.000000000000000000, 0.8660254037844387076, 1.000000000000000000, 0.8660254037844387076, 1.000000000000000000, 0.8660254037844387076, 1.000000000000000000, 0.8660254037844387076, 1.000000000000000000, 0.8660254037844387076, 1.000000000000000000, 0.8660254037844387076, 1.000000000000000000, 0.8660254037844387076, 1.000000000000000000, 0.8660254037844387076, 1.000000000000000000, 0.8660254037844387076, 1.000000000000000000, 0.8660254037844387076, 1.000000000000000000, 0.8660254037844387076, 1.000000000000000000, 0.8660254037844387076, 1.000000000000000000, 0.8660254037844387076, 1.000000000000000000, 0.8660254037844387076, 1.000000000000000000, 0.8660254037844387076, 1.000000000000000000, 0.8660254037844387076, 1.000000000000000000, 0.8660254037844387076, 1.000000000000000000, 0.8660254037844387076, 1.000000000000000000, 0.8660254037844387076, 1.000000000000000000, 0.8660254037844387076, 1.000000000000000000, 0.8660254037844387076, 1.000000000000000000, 0.8660254037844387076, 1.000000000000000000, 0.8660254037844387076, 1.000000000000000000, 0.8660254037844387076, 1.000000000000000000, 0.8660254037844387076, 1.000000000000000000, 0.8660254037844387076, 1.000000000000000000, 0.8660254037844387076, 1.000000000000000000, 0.8660254037844387076, 1.000000000000000000, 0.8660254037844387076, 1.000000000000000000, 0.8660254037844387076, 1.000000000000000000, 0.8660254037844387076, 1.000000000000000000, 0.8660254037844387076, 1.000000000000000000, 0.8660254037844387076, 1.000000000000000000, 0.8660254037844387076, 1.000000000000000000, 0.8660254037844387076, 1.000000000000000000, 0.8660254037844387076, 1.000000000000000000, 0.8660254037844387076, 1.000000000000000000, 0.8660254037844387076, 1.000000000000000000, 0.8660254037844387076, 1.000000000000000000, 0.8660254037844387076, 1.000000000000000000, 0.8660254037844387076, 1.000000000000000000, 0.8660254037844387076, 1.000000000000000000, 0.8660254037844387076, 1.000000000000000000, 0.8660254037844387076, 1.000000000000000000, 0.8660254037844387076, 1.000000000000000000, 0.8660254037844387076, 1.000000000000000000, 0.8660254037844387076, 1.000000000000000000, 0.8660254037844387076, 1.000000000000000000, 0.8660254037844387076, 1.000000000000000000, 0.8660254037844387076, 1.000000000000000000, 0.8660254037844387076, 1.000000000000000000, 0.8660254037844387076, 1.000000000000000000, 0.8660254037844387076, 1.000000000000000000, 0.8660254037844387076, 1.000000000000000000, 0.8660254037844387076, 1.000000000000000000, 0.8660254037844387076, 1.000000000000000000, 0.8660254037844387076, 1.000000000000000000, 0.8660254037844387076, 1.000000000000000000, 0.8660254037844387076, 1.000000000000000000, 0.8660254037844387076, 1.000000000000000000, 0.8660254037844387076, 1.000000000000000000, 0.8660254037844387076, 1.000000000000000000, 0.8660254037844387076, 1.000000000000000000, 0.8660254037844387076, 1.000000000000000000, 0.8660254037844387076, 1.000000000000000000, 0.8660254037844387076, 1.000000000000000000, 0.8660254037844387076, 1.000000000000000000, 0.8660254037844387076, 1.000000000000000000, 0.8660254037844387076, 1.000000000000000000, 0.8660254037844387076, 1.000000000000000000, 0.8660254037844387076, 1.000000000000000000, 0.8660254037844387076, 1.000000000000000000, 0.8660254037844387076, 1.000000000000000000, 0.8660254037844387076, 1.000000000000000000, 0.8660254037844387076, 1.000000000000000000, 0.8660254037844387076, 1.000000000000000000, 0.8660254037844387076, 1.000000000000000000, 0.8660254037844387076, 1.000000000000000000, 0.8660254037844387076, 1.000000000000000000, 0.8660254037844387076, 1.000000000000000000, 0.8660254037844387076, 1.000000000000000000, 0.8660254037844387076, 1.000000000000000000, 0.8660254037844387076, 1.000000000000000000, 0.8660254037844387076, 1.000000000000000000, 0.8660254037844387076, 1.000000000000000000, 0.8660254037844387076, 1.000000000000000000, 0.8660254037844387076, 1.000000000000000000, 0.8660254037844387076, 1.000000000000000000, 0.8660254037844387076, 1.000000000000000000, 0.8660254037844387076, 1.000000000000000000, 0.8660254037844387076, 1.000000000000000000, 0.8660254037844387076, 1.000000000000000000, 0.8660254037844387076, 1.000000000000000000, 0.8660254037844387076, 1.000000000000000000, 0.8660254037844387076, 1.000000000000000000, 0.8660254037844387076, 1.000000000000000000, 0.8660254037844387076, 1.000000000000000000, 0.8660254037844387076, 1.000000000000000000, 0.8660254037844387076, 1.000000000000000000, 0.8660254037844387076, 1.000000000000000000, 0.8660254037844387076, 1.000000000000000000, 0.8660254037844387076, 1.000000000000000000, 0.8660254037844387076, 1.000000000000000000, 0.8660254037844387076, 1.000000000000000000, 0.8660254037844387076, 1.000000000000000000, 0.8660254037844387076, 1.000000000000000000, 0.8660254037844387076, 1.000000000000000000, 0.8660254037844387076, 1.000000000000000000, 0.8660254037844387076, 1.000000000000000000, 0.8660254037844387076, 1.000000000000000000, 0.8660254037844387076, 1.000000000000000000, 0.8660254037844387076, 1.000000000000000000, 0.8660254037844387076, 1.000000000000000000, 0.8660254037844387076, 1.000000000000000000, 0.8660254037844387076, 1.000000000000000000, 0.8660254037844387076, 1.000000000000000000, 0.8660254037844387076, 1.000000000000000000, 0.8660254037844387076, 1.000000000000000000, 0.8660254037844387076, 1.000000000000000000, 0.8660254037844387076, 1.000000000000000000, 0.8660254037844387076, 1.000000000000000000, 0.8660254037844387076, 1.000000000000000000, 0.8660254037844387076, 1.000000000000000000, 0.8660254037844387076, 1.000000000000000000, 0.8660254037844387076, 1.000000000000000000, 0.8660254037844387076, 1.000000000000000000, 0.8660254037844387076, 1.000000000000000000, 0.8660254037844387076, 1.000000000000000000, 0.8660254037844387076, 1.000000000000000000, 0.8660254037844387076, 1.000000000000000000, 0.8660254037844387076, 1.000000000000000000, 0.8660254037844387076, 1.000000000000000000, 0.8660254037844387076, 1.000000000000000000, 0.8660254037844387076, 1.000000000000000000, 0.8660254037844387076, 1.000000000000000000, 0.8660254037844387076, 1.000000000000000000, 0.8660254037844387076, 1.000000000000000000, 0.8660254037844387076, 1.000000000000000000, 0.8660254037844387076, 1.000000000000000000, 0.8660254037844387076, 1.000000000000000000, 0.8660254037844387076, 1.000000000000000000, 0.8660254037844387076, 1.000000000000000000, 0.8660254037844387076, 1.000000000000000000, 0.8660254037844387076, 1.000000000000000000, 0.8660254037844387076, 1.000000000000000000, 0.8660254037844387076, 1.000000000000000000, 0.8660254037844387076, 1.000000000000000000, 0.8660254037844387076, 1.000000000000000000, 0.8660254037844387076, 1.000000000000000000, 0.8660254037844387076, 1.000000000000000000, 0.8660254037844387076, 1.000000000000000000, 0.8660254037844387076, 1.000000000000000000, 0.8660254037844387076, 1.000000000000000000, 0.8660254037844387076, 1.000000000000000000, 0.8660254037844387076, 1.000000000000000000, 0.8660254037844387076, 1.000000000000000000, 0.8660254037844387076, 1.000000000000000000, 0.8660254037844387076, 1.000000000000000000, 0.8660254037844387076, 1.000000000000000000, 0.8660254037844387076, 1.000000000000000000, 0.8660254037844387076, 1.000000000000000000, 0.8660254037844387076, 1.000000000000000000, 0.8660254037844387076, 1.000000000000000000, 0.8660254037844387076, 1.000000000000000000, 0.8660254037844387076, 1.000000000000000000, 0.8660254037844387076, 1.000000000000000000, 0.8660254037844387076, 1.000000000000000000, 0.8660254037844387076, 1.000000000000000000, 0.8660254037844387076, 1.000000000000000000, 0.8660254037844387076, 1.000000000000000000, 0.8660254037844387076, 1.000000000000000000, 0.8660254037844387076, 1.000000000000000000, 0.8660254037844387076, 1.000000000000000000, 0.8660254037844387076, 1.000000000000000000, 0.8660254037844387076, 1.000000000000000000, 0.8660254037844387076, 1.000000000000000000, 0.8660254037844387076, 1.000000000000000000, 0.8660254037844387076, 1.000000000000000000, 0.8660254037844387076, 1.000000000000000000, 0.8660254037844387076, 1.000000000000000000, 0.8660254037844387076, 1.000000000000000000, 0.8660254037844387076, 1.000000000000000000, 0.8660254037844387076, 1.000000000000000000, 0.8660254037844387076, 1.000000000000000000, 0.8660254037844387076, 1.000000000000000000, 0.8660254037844387076, 1.000000000000000000, 0.8660254037844387076, 1.000000000000000000, 0.8660254037844387076, 1.000000000000000000, 0.8660254037844387076, 1.000000000000000000, 0.8660254037844387076, 1.000000000000000000, 0.8660254037844387076, 1.000000000000000000, 0.8660254037844387076, 1.000000000000000000, 0.8660254037844387076, 1.000000000000000000, 0.8660254037844387076, 1.000000000000000000, 0.8660254037844387076, 1.000000000000000000, 0.8660254037844387076, 1.000000000000000000, 0.8660254037844387076, 1.000000000000000000, 0.8660254037844387076, 1.000000000000000000, 0.8660254037844387076, 1.000000000000000000, 0.8660254037844387076, 1.000000000000000000, 0.8660254037844387076, 1.000000000000000000, 0.8660254037844387076, 1.000000000000000000, 0.8660254037844387076, 1.000000000000000000, 0.8660254037844387076, 1.000000000000000000, 0.8660254037844387076, 1.000000000000000000, 0.8660254037844387076, 1.000000000000000000, 0.8660254037844387076, 1.000000000000000000, 0.8660254037844387076, 1.000000000000000000, 0.8660254037844387076, 1.000000000000000000, 0.8660254037844387076, 1.000000000000000000, 0.8660254037844387076, 1.000000000000000000, 0.8660254037844387076, 1.000000000000000000, 0.8660254037844387076, 1.000000000000000000, 0.8660254037844387076, 1.000000000000000000, 0.8660254037844387076, 1.000000000000000000, 0.8660254037844387076, 1.000000000000000000, 0.8660254037844387076, 1.000000000000000000, 0.8660254037844387076, 1.000000000000000000, 0.8660254037844387076, 1.000000000000000000, 0.8660254037844387076, 1.000000000000000000, 0.8660254037844387076, 1.000000000000000000, 0.8660254037844387076, 1.000000000000000000, 0.8660254037844387076, 1.000000000000000000, 0.8660254037844387076, 1.000000000000000000, 0.8660254037844387076, 1.000000000000000000, 0.8660254037844387076, 1.000000000000000000, 0.8660254037844387076, 1.000000000000000000, 0.8660254037844387076, 1.000000000000000000, 0.8660254037844387076, 1.000000000000000000, 0.8660254037844387076, 1.000000000000000000, 0.8660254037844387076, 1.000000000000000000, 0.8660254037844387076, 1.000000000000000000, 0.8660254037844387076, 1.000000000000000000, 0.8660254037844387076, 1.000000000000000000, 0.8660254037844387076, 1.000000000000000000, 0.8660254037844387076, 1.000000000000000000, 0.8660254037844387076, 1.000000000000000000, 0.8660254037844387076, 1.000000000000000000, 0.8660254037844387076, 1.000000000000000000, 0.8660254037844387076, 1.000000000000000000, 0.8660254037844387076, 1.000000000000000000, 0.8660254037844387076, 1.000000000000000000, 0.8660254037844387076, 1.000000000000000000, 0.8660254037844387076, 1.000000000000000000, 0.8660254037844387076, 1.000000000000000000, 0.8660254037844387076, 1.000000000000000000, 0.8660254037844387076, 1.000000000000000000, 0.8660254037844387076, 1.000000000000000000, 0.8660254037844387076, 1.000000000000000000, 0.8660254037844387076, 1.000000000000000000, 0.8660254037844387076, 1.000000000000000000, 0.8660254037844387076, 1.000000000000000000, 0.8660254037844387076, 1.000000000000000000, 0.8660254037844387076, 1.000000000000000000, 0.8660254037844387076, 1.000000000000000000, 0.8660254037844387076, 1.000000000000000000, 0.8660254037844387076, 1.000000000000000000, 0.8660254037844387076, 1.000000000000000000, 0.8660254037844387076, 1.000000000000000000, 0.8660254037844387076, 1.000000000000000000, 0.8660254037844387076, 1.000000000000000000, 0.8660254037844387076, 1.000000000000000000, 0.8660254037844387076, 1.000000000000000000, 0.8660254037844387076, 1.000000000000000000, 0.8660254037844387076, 1.000000000000000000, 0.8660254037844387076, 1.000000000000000000, 0.8660254037844387076, 1.000000000000000000, 0.8660254037844387076, 1.000000000000000000, 0.8660254037844387076, 1.000000000000000000, 0.8660254037844387076, 1.000000000000000000, 0.8660254037844387076, 1.000000000000000000, 0.8660254037844387076, 1.000000000000000000, 0.8660254037844387076, 1.000000000000000000, 0.8660254037844387076, 1.000000000000000000, 0.8660254037844387076, 1.000000000000000000, 0.8660254037844387076, 1.000000000000000000, 0.8660254037844387076, 1.000000000000000000, 0.8660254037844387076, 1.000000000000000000, 0.8660254037844387076, 1.000000000000000000, 0.8660254037844387076, 1.000000000000000000, 0.8660254037844387076, 1.000000000000000000),
 ( 1.000000000000000000, 0.8660254037844387076, 1.000000000000000000, 0.8660254037844387076, 1.000000000000000000, 0.8660254037844387076, 1.000000000000000000, 0.8660254037844387076, 1.000000000000000000, 0.8660254037844387076, 1.000000000000000000, 0.8660254037844387076, 1.000000000000000000, 0.8660254037844387076, 1.000000000000000000, 0.8660254037844387076, 1.000000000000000000, 0.8660254037844387076, 1.000000000000000000, 0.8660254037844387076, 1.000000000000000000, 0.8660254037844387076, 1.000000000000000000, 0.8660254037844387076, 1.000000000000000000, 0.8660254037844387076, 1.000000000000000000, 0.8660254037844387076, 1.000000000000000000, 0.8660254037844387076, 1.000000000000000000, 0.8660254037844387076, 1.000000000000000000, 0.8660254037844387076, 1.000000000000000000, 0.8660254037844387076, 1.000000000000000000, 0.8660254037844387076, 1.000000000000000000, 0.8660254037844387076, 1.000000000000000000, 0.8660254037844387076, 1.000000000000000000, 0.8660254037844387076, 1.000000000000000000, 0.8660254037844387076, 1.000000000000000000, 0.8660254037844387076, 1.000000000000000000, 0.8660254037844387076, 1.000000000000000000, 0.8660254037844387076, 1.000000000000000000, 0.8660254037844387076, 1.000000000000000000, 0.8660254037844387076, 1.000000000000000000, 0.8660254037844387076, 1.000000000000000000, 0.8660254037844387076, 1.000000000000000000, 0.8660254037844387076, 1.000000000000000000, 0.8660254037844387076, 1.000000000000000000, 0.8660254037844387076, 1.000000000000000000, 0.8660254037844387076, 1.000000000000000000, 0.8660254037844387076, 1.000000000000000000, 0.8660254037844387076, 1.000000000000000000, 0.8660254037844387076, 1.000000000000000000, 0.8660254037844387076, 1.000000000000000000, 0.8660254037844387076, 1.000000000000000000, 0.8660254037844387076, 1.000000000000000000, 0.8660254037844387076, 1.000000000000000000, 0.8660254037844387076, 1.000000000000000000, 0.8660254037844387076, 1.000000000000000000, 0.8660254037844387076, 1.000000000000000000, 0.8660254037844387076, 1.000000000000000000, 0.8660254037844387076, 1.000000000000000000, 0.8660254037844387076, 1.000000000000000000, 0.8660254037844387076, 1.000000000000000000, 0.8660254037844387076, 1.000000000000000000, 0.8660254037844387076, 1.000000000000000000, 0.8660254037844387076, 1.000000000000000000, 0.8660254037844387076, 1.000000000000000000, 0.8660254037844387076, 1.000000000000000000, 0.8660254037844387076, 1.000000000000000000, 0.8660254037844387076, 1.000000000000000000, 0.8660254037844387076, 1.000000000000000000, 0.8660254037844387076, 1.000000000000000000, 0.8660254037844387076, 1.000000000000000000, 0.8660254037844387076, 1.000000000000000000, 0.8660254037844387076, 1.000000000000000000, 0.8660254037844387076, 1.000000000000000000, 0.8660254037844387076, 1.000000000000000000, 0.8660254037844387076, 1.000000000000000000, 0.8660254037844387076, 1.000000000000000000, 0.8660254037844387076, 1.000000000000000000, 0.8660254037844387076, 1.000000000000000000, 0.8660254037844387076, 1.000000000000000000, 0.8660254037844387076, 1.000000000000000000, 0.8660254037844387076, 1.000000000000000000, 0.8660254037844387076, 1.000000000000000000, 0.8660254037844387076, 1.000000000000000000, 0.8660254037844387076, 1.000000000000000000, 0.8660254037844387076, 1.000000000000000000, 0.8660254037844387076, 1.000000000000000000, 0.8660254037844387076, 1.000000000000000000, 0.8660254037844387076, 1.000000000000000000, 0.8660254037844387076, 1.000000000000000000, 0.8660254037844387076, 1.000000000000000000, 0.8660254037844387076, 1.000000000000000000, 0.8660254037844387076, 1.000000000000000000, 0.8660254037844387076, 1.000000000000000000, 0.8660254037844387076, 1.000000000000000000, 0.8660254037844387076, 1.000000000000000000, 0.8660254037844387076, 1.000000000000000000, 0.8660254037844387076, 1.000000000000000000, 0.8660254037844387076, 1.000000000000000000, 0.8660254037844387076, 1.000000000000000000, 0.8660254037844387076, 1.000000000000000000, 0.8660254037844387076, 1.000000000000000000, 0.8660254037844387076, 1.000000000000000000, 0.8660254037844387076, 1.000000000000000000, 0.8660254037844387076, 1.000000000000000000, 0.8660254037844387076, 1.000000000000000000, 0.8660254037844387076, 1.000000000000000000, 0.8660254037844387076, 1.000000000000000000, 0.8660254037844387076, 1.000000000000000000, 0.8660254037844387076, 1.000000000000000000, 0.8660254037844387076, 1.000000000000000000, 0.8660254037844387076, 1.000000000000000000, 0.8660254037844387076, 1.000000000000000000, 0.8660254037844387076, 1.000000000000000000, 0.8660254037844387076, 1.000000000000000000, 0.8660254037844387076, 1.000000000000000000, 0.8660254037844387076, 1.000000000000000000, 0.8660254037844387076, 1.000000000000000000, 0.8660254037844387076, 1.000000000000000000, 0.8660254037844387076, 1.000000000000000000, 0.8660254037844387076, 1.000000000000000000, 0.8660254037844387076, 1.000000000000000000, 0.8660254037844387076, 1.000000000000000000, 0.8660254037844387076, 1.000000000000000000, 0.8660254037844387076, 1.000000000000000000, 0.8660254037844387076, 1.000000000000000000, 0.8660254037844387076, 1.000000000000000000, 0.8660254037844387076, 1.000000000000000000, 0.8660254037844387076, 1.000000000000000000, 0.8660254037844387076, 1.000000000000000000, 0.8660254037844387076, 1.000000000000000000, 0.8660254037844387076, 1.000000000000000000, 0.8660254037844387076, 1.000000000000000000, 0.8660254037844387076, 1.000000000000000000, 0.8660254037844387076, 1.000000000000000000, 0.8660254037844387076, 1.000000000000000000, 0.8660254037844387076, 1.000000000000000000, 0.8660254037844387076, 1.000000000000000000, 0.8660254037844387076, 1.000000000000000000, 0.8660254037844387076, 1.000000000000000000, 0.8660254037844387076, 1.000000000000000000, 0.8660254037844387076, 1.000000000000000000, 0.8660254037844387076, 1.000000000000000000, 0.8660254037844387076, 1.000000000000000000, 0.8660254037844387076, 1.000000000000000000, 0.8660254037844387076, 1.000000000000000000, 0.8660254037844387076, 1.000000000000000000, 0.8660254037844387076, 1.000000000000000000, 0.8660254037844387076, 1.000000000000000000, 0.8660254037844387076, 1.000000000000000000, 0.8660254037844387076, 1.000000000000000000, 0.8660254037844387076, 1.000000000000000000, 0.8660254037844387076, 1.000000000000000000, 0.8660254037844387076, 1.000000000000000000, 0.8660254037844387076, 1.000000000000000000, 0.8660254037844387076, 1.000000000000000000, 0.8660254037844387076, 1.000000000000000000, 0.8660254037844387076, 1.000000000000000000, 0.8660254037844387076, 1.000000000000000000, 0.8660254037844387076, 1.000000000000000000, 0.8660254037844387076, 1.000000000000000000, 0.8660254037844387076, 1.000000000000000000, 0.8660254037844387076, 1.000000000000000000, 0.8660254037844387076, 1.000000000000000000, 0.8660254037844387076, 1.000000000000000000, 0.8660254037844387076, 1.000000000000000000, 0.8660254037844387076, 1.000000000000000000, 0.8660254037844387076, 1.000000000000000000, 0.8660254037844387076, 1.000000000000000000, 0.8660254037844387076, 1.000000000000000000, 0.8660254037844387076, 1.000000000000000000, 0.8660254037844387076, 1.000000000000000000, 0.8660254037844387076, 1.000000000000000000, 0.8660254037844387076, 1.000000000000000000, 0.8660254037844387076, 1.000000000000000000, 0.8660254037844387076, 1.000000000000000000, 0.8660254037844387076, 1.000000000000000000, 0.8660254037844387076, 1.000000000000000000, 0.8660254037844387076, 1.000000000000000000, 0.8660254037844387076, 1.000000000000000000, 0.8660254037844387076, 1.000000000000000000, 0.8660254037844387076, 1.000000000000000000, 0.8660254037844387076, 1.000000000000000000, 0.8660254037844387076, 1.000000000000000000, 0.8660254037844387076, 1.000000000000000000, 0.8660254037844387076, 1.000000000000000000, 0.8660254037844387076, 1.000000000000000000, 0.8660254037844387076, 1.000000000000000000, 0.8660254037844387076, 1.000000000000000000, 0.8660254037844387076, 1.000000000000000000, 0.8660254037844387076, 1.000000000000000000, 0.8660254037844387076, 1.000000000000000000, 0.8660254037844387076, 1.000000000000000000, 0.8660254037844387076, 1.000000000000000000, 0.8660254037844387076, 1.000000000000000000, 0.8660254037844387076, 1.000000000000000000, 0.8660254037844387076, 1.000000000000000000, 0.8660254037844387076, 1.000000000000000000, 0.8660254037844387076, 1.000000000000000000, 0.8660254037844387076, 1.000000000000000000, 0.8660254037844387076, 1.000000000000000000, 0.8660254037844387076, 1.000000000000000000, 0.8660254037844387076, 1.000000000000000000, 0.8660254037844387076, 1.000000000000000000, 0.8660254037844387076, 1.000000000000000000, 0.8660254037844387076, 1.000000000000000000, 0.8660254037844387076, 1.000000000000000000, 0.8660254037844387076, 1.000000000000000000, 0.8660254037844387076, 1.000000000000000000, 0.8660254037844387076, 1.000000000000000000, 0.8660254037844387076, 1.000000000000000000, 0.8660254037844387076, 1.000000000000000000, 0.8660254037844387076, 1.000000000000000000, 0.8660254037844387076, 1.000000000000000000, 0.8660254037844387076, 1.000000000000000000, 0.8660254037844387076, 1.000000000000000000, 0.8660254037844387076, 1.000000000000000000, 0.8660254037844387076, 1.000000000000000000, 0.8660254037844387076, 1.000000000000000000, 0.8660254037844387076, 1.000000000000000000, 0.8660254037844387076, 1.000000000000000000, 0.8660254037844387076, 1.000000000000000000, 0.8660254037844387076, 1.000000000000000000, 0.8660254037844387076, 1.000000000000000000, 0.8660254037844387076, 1.000000000000000000, 0.8660254037844387076, 1.000000000000000000, 0.8660254037844387076, 1.000000000000000000, 0.8660254037844387076, 1.000000000000000000, 0.8660254037844387076, 1.000000000000000000, 0.8660254037844387076, 1.000000000000000000, 0.8660254037844387076, 1.000000000000000000, 0.8660254037844387076, 1.000000000000000000, 0.8660254037844387076, 1.000000000000000000, 0.8660254037844387076, 1.000000000000000000, 0.8660254037844387076, 1.000000000000000000, 0.8660254037844387076, 1.000000000000000000, 0.8660254037844387076, 1.000000000000000000, 0.8660254037844387076, 1.000000000000000000, 0.8660254037844387076, 1.000000000000000000, 0.8660254037844387076, 1.000000000000000000, 0.8660254037844387076, 1.000000000000000000, 0.8660254037844387076, 1.000000000000000000, 0.8660254037844387076, 1.000000000000000000, 0.8660254037844387076, 1.000000000000000000, 0.8660254037844387076, 1.000000000000000000, 0.8660254037844387076, 1.000000000000000000, 0.8660254037844387076, 1.000000000000000000, 0.8660254037844387076, 1.000000000000000000, 0.8660254037844387076, 1.000000000000000000, 0.8660254037844387076, 1.000000000000000000, 0.8660254037844387076, 1.000000000000000000, 0.8660254037844387076, 1.000000000000000000, 0.8660254037844387076, 1.000000000000000000, 0.8660254037844387076, 1.000000000000000000, 0.8660254037844387076, 1.000000000000000000, 0.8660254037844387076, 1.000000000000000000, 0.8660254037844387076, 1.000000000000000000, 0.8660254037844387076, 1.000000000000000000, 0.8660254037844387076, 1.000000000000000000, 0.8660254037844387076, 1.000000000000000000, 0.8660254037844387076, 1.000000000000000000, 0.8660254037844387076, 1.000000000000000000, 0.8660254037844387076, 1.000000000000000000, 0.8660254037844387076, 1.000000000000000000, 0.8660254037844387076, 1.000000000000000000, 0.8660254037844387076, 1.000000000000000000, 0.8660254037844387076, 1.000000000000000000, 0.8660254037844387076, 1.000000000000000000, 0.8660254037844387076, 1.000000000000000000, 0.8660254037844387076, 1.000000000000000000, 0.8660254037844387076, 1.000000000000000000, 0.8660254037844387076, 1.000000000000000000, 0.8660254037844387076, 1.000000000000000000, 0.8660254037844387076, 1.000000000000000000, 0.8660254037844387076, 1.000000000000000000, 0.8660254037844387076, 1.000000000000000000, 0.8660254037844387076, 1.000000000000000000, 0.8660254037844387076, 1.000000000000000000, 0.8660254037844387076, 1.000000000000000000, 0.8660254037844387076, 1.000000000000000000, 0.8660254037844387076, 1.000000000000000000, 0.8660254037844387076, 1.000000000000000000, 0.8660254037844387076, 1.000000000000000000, 0.8660254037844387076, 1.000000000000000000, 0.8660254037844387076, 1.000000000000000000, 0.8660254037844387076, 1.000000000000000000, 0.8660254037844387076, 1.000000000000000000, 0.8660254037844387076, 1.000000000000000000, 0.8660254037844387076, 1.000000000000000000, 0.8660254037844387076, 1.000000000000000000, 0.8660254037844387076, 1.000000000000000000, 0.8660254037844387076, 1.000000000000000000, 0.8660254037844387076, 1.000000000000000000, 0.8660254037844387076, 1.000000000000000000, 0.8660254037844387076, 1.000000000000000000, 0.8660254037844387076, 1.000000000000000000, 0.8660254037844387076, 1.000000000000000000, 0.8660254037844387076, 1.000000000000000000, 0.8660254037844387076, 1.000000000000000000, 0.8660254037844387076, 1.000000000000000000, 0.8660254037844387076, 1.000000000000000000, 0.8660254037844387076, 1.000000000000000000, 0.8660254037844387076, 1.000000000000000000, 0.8660254037844387076, 1.000000000000000000, 0.8660254037844387076, 1.000000000000000000, 0.8660254037844387076, 1.000000000000000000, 0.8660254037844387076, 1.000000000000000000, 0.8660254037844387076, 1.000000000000000000, 0.8660254037844387076, 1.000000000000000000, 0.8660254037844387076, 1.000000000000000000, 0.8660254037844387076, 1.000000000000000000, 0.8660254037844387076, 1.000000000000000000, 0.8660254037844387076, 1.000000000000000000) ) ) 
 REPRESENTATION_ITEM ( '' )  SURFACE ( )  );
#9608 = CARTESIAN_POINT ( 'NONE',  ( 11.22187500061451892, 3.027376345333613106, -5.243569643749998122 ) ) ;
#9609 = CARTESIAN_POINT ( 'NONE',  ( 5.625000001229036428, 2.886751345948129099, -4.999999999999998224 ) ) ;
#9610 = CARTESIAN_POINT ( 'NONE',  ( 15.27187500061451786, 3.027376345333613106, -5.243569643749998122 ) ) ;
#9611 = CARTESIAN_POINT ( 'NONE',  ( 5.296875000614518214, -3.027376345333610441, -5.243569643749999898 ) ) ;
#9612 = DIRECTION ( 'NONE',  ( 0.000000000000000000, 0.000000000000000000, 1.000000000000000000 ) ) ;
#9613 = DIRECTION ( 'NONE',  ( 0.000000000000000000, 0.000000000000000000, -1.000000000000000000 ) ) ;
#9614 = CARTESIAN_POINT ( 'NONE',  ( 12.19687500061451679, 6.054752690667223547, 3.707466751127219781E-16 ) ) ;
#9615 = FACE_OUTER_BOUND ( 'NONE', #70642, .T. ) ;
#9616 = CARTESIAN_POINT ( 'NONE',  ( 23.20312500061451644, -4.541064518000417216, -2.621784821875001281 ) ) ;
#9617 = CARTESIAN_POINT ( 'NONE',  ( 3.999999999999999112, 11.67500000000000071, 30.00000000000000000 ) ) ;
#9618 = CARTESIAN_POINT ( 'NONE',  ( -4.243569643749999898, 18.86562500061459247, 27.54997392385601529 ) ) ;
#9619 = CARTESIAN_POINT ( 'NONE',  ( 23.78437500061451360, 6.421520780324663323E-16, -5.243569643749999010 ) ) ;
#9620 = CARTESIAN_POINT ( 'NONE',  ( 4.142324674002726859, 2.800292288406700969, -4.194544246395793152 ) ) ;
#9621 = CARTESIAN_POINT ( 'NONE',  ( 3.628125000614518036, 4.541064518000418104, 2.621784821874999949 ) ) ;
#9622 = EDGE_CURVE ( 'NONE', #29484, #44903, #11414, .T. ) ;
#9623 = CARTESIAN_POINT ( 'NONE',  ( 20.18437500061451217, 5.492252693125287522, 3.363034840372157021E-16 ) ) ;
#9624 = CARTESIAN_POINT ( 'NONE',  ( 17.84062500061451573, -3.027376345333610441, -5.243569643749999898 ) ) ;
#9625 = CARTESIAN_POINT ( 'NONE',  ( 15.27187500061451786, 3.027376345333613106, -5.243569643749998122 ) ) ;
#9626 = CARTESIAN_POINT ( 'NONE',  ( 7.321875000614517681, -4.119189519843968306, 2.378215178124996054 ) ) ;
#9627 = CARTESIAN_POINT ( 'NONE',  ( 26.77500000122903145, 2.886751345948129099, -4.999999999999998224 ) ) ;
#9628 = CARTESIAN_POINT ( 'NONE',  ( 5.934375000614517504, 4.541064518000418104, 2.621784821874999949 ) ) ;
#9629 = CARTESIAN_POINT ( 'NONE',  ( 16.35937500061451644, 0.000000000000000000, 5.243569643749999010 ) ) ;
#9630 = CARTESIAN_POINT ( 'NONE',  ( 23.32499999999999929, -4.330127018922194537, 2.499999999999995559 ) ) ;
#9631 = CARTESIAN_POINT ( 'NONE',  ( 16.83750000122903145, 6.123233995736764310E-16, -4.999999999999998224 ) ) ;
#9632 = CARTESIAN_POINT ( 'NONE',  ( 25.58437500061451431, 6.421520780324663323E-16, -5.243569643749999010 ) ) ;
#9633 = CARTESIAN_POINT ( 'NONE',  ( 16.62187500061451573, 3.027376345333613106, -5.243569643749998122 ) ) ;
#9634 = CARTESIAN_POINT ( 'NONE',  ( -7.967954043666661671E-16, 13.99062499938548498, 34.33755215474603517 ) ) ;
#9635 = CARTESIAN_POINT ( 'NONE',  ( 29.81250000000000000, 2.886751345948129099, -4.999999999999998224 ) ) ;
#9636 = CARTESIAN_POINT ( 'NONE',  ( 7.687500000000000000, -2.886751345948125991, -5.000000000000000000 ) ) ;
#9637 = CARTESIAN_POINT ( 'NONE',  ( 9.271875000614517859, 5.824947211148865298E-16, -4.756430356249998326 ) ) ;
#9638 = CARTESIAN_POINT ( 'NONE',  ( 20.69062500061451715, 6.054752690667223547, 3.707466751127219781E-16 ) ) ;
#9639 = CARTESIAN_POINT ( 'NONE',  ( 8.474999999999999645, -4.330127018922194537, 2.499999999999995559 ) ) ;
#9640 = CARTESIAN_POINT ( 'NONE',  ( 3.215625000614518836, 3.027376345333611329, 5.243569643749999010 ) ) ;
#9641 = CARTESIAN_POINT ( 'NONE',  ( 19.94999999999999929, 4.330127018922192761, -2.499999999999997780 ) ) ;
#9642 = EDGE_CURVE ( 'NONE', #30208, #47001, #7663, .T. ) ;
#9643 = CARTESIAN_POINT ( 'NONE',  ( 18.29062500061451502, -3.027376345333610441, -5.243569643749999898 ) ) ;
#9644 = CARTESIAN_POINT ( 'NONE',  ( 14.62500000000000000, 4.330127018922191873, 2.499999999999999556 ) ) ;
#9645 = CARTESIAN_POINT ( 'NONE',  ( 22.80000000122903359, 5.773502691896255534, 3.535250795749688894E-16 ) ) ;
#9646 = CARTESIAN_POINT ( 'NONE',  ( 2.923357432354301455, -4.056350739605543154, 3.322806236625610588 ) ) ;
#9647 = CARTESIAN_POINT ( 'NONE',  ( 28.77187500061451431, 3.027376345333613106, -5.243569643749998122 ) ) ;
#9648 = ORIENTED_EDGE ( 'NONE', *, *, #15704, .F. ) ;
#9649 = CARTESIAN_POINT ( 'NONE',  ( 17.84062500061451573, -3.027376345333610441, -5.243569643749999898 ) ) ;
#9650 = CARTESIAN_POINT ( 'NONE',  ( 24.81562500061451715, 3.027376345333611329, 5.243569643749999010 ) ) ;
#9651 = CARTESIAN_POINT ( 'NONE',  ( 25.84687500061451360, -3.027376345333614438, 5.243569643749998122 ) ) ;
#9652 = CARTESIAN_POINT ( 'NONE',  ( 10.05000000000000071, 4.330127018922192761, -2.499999999999997780 ) ) ;
#9653 = CARTESIAN_POINT ( 'NONE',  ( 11.12812500061451715, 6.421520780324663323E-16, -5.243569643749999010 ) ) ;
#9654 = CARTESIAN_POINT ( 'NONE',  ( 25.71562500061451573, 3.027376345333611329, 5.243569643749999010 ) ) ;
#9655 = CARTESIAN_POINT ( 'NONE',  ( 18.00937500061451502, 4.541064518000418104, -2.621784821874998173 ) ) ;
#9656 = CARTESIAN_POINT ( 'NONE',  ( 18.57187500061451857, 3.027376345333611329, 5.243569643749999010 ) ) ;
#9657 = CARTESIAN_POINT ( 'NONE',  ( 3.065815551951259543, -3.949781639713015657, 3.065815551951216467 ) ) ;
#9658 = CARTESIAN_POINT ( 'NONE',  ( -4.243569643749997233, 9.996875000614517504, 32.45002607614398471 ) ) ;
#9659 = CARTESIAN_POINT ( 'NONE',  ( 23.40000000122903145, -2.886751345948129988, 4.999999999999997335 ) ) ;
#9660 = CARTESIAN_POINT ( 'NONE',  ( 16.17187500061451644, 2.746126346562645981, -4.756430356249997438 ) ) ;
#9661 = CARTESIAN_POINT ( 'NONE',  ( 13.86562500061451431, 3.027376345333612662, -5.243569643749998122 ) ) ;
#9662 = PRODUCT_DEFINITION_FORMATION_WITH_SPECIFIED_SOURCE ( 'ANY', '', #23145, .NOT_KNOWN. ) ;
#9663 = CARTESIAN_POINT ( 'NONE',  ( 8.296875000614516438, -3.027376345333614438, 5.243569643749998122 ) ) ;
#9664 = CARTESIAN_POINT ( 'NONE',  ( 6.984375000614516438, -4.541064518000419881, 2.621784821874995952 ) ) ;
#9665 = ORIENTED_EDGE ( 'NONE', *, *, #12071, .T. ) ;
#9666 = CARTESIAN_POINT ( 'NONE',  ( 29.78437500061451715, 4.541064518000418104, 2.621784821874999949 ) ) ;
#9667 = CARTESIAN_POINT ( 'NONE',  ( 20.24062500061451431, 6.054752690667223547, 3.707466751127219781E-16 ) ) ;
#9668 = CARTESIAN_POINT ( 'NONE',  ( 23.37187500061451573, 3.027376345333613106, -5.243569643749998122 ) ) ;
#9669 = CARTESIAN_POINT ( 'NONE',  ( 20.09062500061451573, -3.027376345333610441, -5.243569643749999898 ) ) ;
#9670 = CARTESIAN_POINT ( 'NONE',  ( 3.999999999999999112, 11.67500000000000071, 30.00000000000000000 ) ) ;
#9671 = CARTESIAN_POINT ( 'NONE',  ( 25.90312500061451573, -4.541064518000417216, -2.621784821875001281 ) ) ;
#9672 = CARTESIAN_POINT ( 'NONE',  ( 7.837500001229035007, 6.123233995736764310E-16, -4.999999999999998224 ) ) ;
#9673 = ORIENTED_EDGE ( 'NONE', *, *, #70375, .F. ) ;
#9674 = CARTESIAN_POINT ( 'NONE',  ( 3.187500001229033764, -4.330127018922194537, 2.499999999999995559 ) ) ;
#9675 = CARTESIAN_POINT ( 'NONE',  ( -1.999999999999997113, 15.12500000000000000, -26.53589838486224295 ) ) ;
#9676 = CARTESIAN_POINT ( 'NONE',  ( 21.97500000122903074, 2.886751345948126879, 4.999999999999999112 ) ) ;
#9677 = CARTESIAN_POINT ( 'NONE',  ( 3.756430356250000546, 14.59062499938548463, 27.83122392262697886 ) ) ;
#9678 = CARTESIAN_POINT ( 'NONE',  ( 6.159375000614517148, -4.541064518000417216, -2.621784821875001281 ) ) ;
#9679 = CARTESIAN_POINT ( 'NONE',  ( 12.86250000000000071, 2.886751345948126879, 4.999999999999998224 ) ) ;
#9680 = CARTESIAN_POINT ( 'NONE',  ( 11.50312500061451892, -4.541064518000417216, -2.621784821875001281 ) ) ;
#9681 = CARTESIAN_POINT ( 'NONE',  ( 9.159375000614515372, 0.000000000000000000, 5.243569643749999010 ) ) ;
#9682 = CARTESIAN_POINT ( 'NONE',  ( 26.88750000122903216, 4.330127018922191873, 2.499999999999999556 ) ) ;
#9683 = CARTESIAN_POINT ( 'NONE',  ( 14.29687500061451821, -3.027376345333610441, -5.243569643749999898 ) ) ;
#9684 = CARTESIAN_POINT ( 'NONE',  ( 5.784375000614517148, 6.421520780324663323E-16, -5.243569643749999010 ) ) ;
#9685 = CARTESIAN_POINT ( 'NONE',  ( 29.39999999999999858, 4.330127018922192761, -2.499999999999997780 ) ) ;
#9686 = CARTESIAN_POINT ( 'NONE',  ( 4.903125000614516615, 4.541064518000418104, -2.621784821874998173 ) ) ;
#9687 = CARTESIAN_POINT ( 'NONE',  ( 15.77812500061451573, 4.541064518000418104, 2.621784821874999949 ) ) ;
#9688 = ORIENTED_EDGE ( 'NONE', *, *, #61648, .F. ) ;
#9689 = CARTESIAN_POINT ( 'NONE',  ( 12.66562500061451502, 3.027376345333611329, 5.243569643749999010 ) ) ;
#9690 = CARTESIAN_POINT ( 'NONE',  ( 8.278125000614515727, -4.541064518000419881, 2.621784821874995952 ) ) ;
#9691 = CARTESIAN_POINT ( 'NONE',  ( 20.82187500061451857, 2.746126346562643317, 4.756430356249998326 ) ) ;
#9692 = CARTESIAN_POINT ( 'NONE',  ( 9.000000000000001776, -4.330127018922190985, -2.500000000000001332 ) ) ;
#9693 = CARTESIAN_POINT ( 'NONE',  ( 3.487500001229035362, 4.330127018922191873, 2.499999999999999556 ) ) ;
#9694 = CARTESIAN_POINT ( 'NONE',  ( 17.02499999999999858, -4.330127018922194537, 2.499999999999995559 ) ) ;
#9695 = CARTESIAN_POINT ( 'NONE',  ( 17.82187500061451502, -6.054752690667223547, -1.112240025338166033E-15 ) ) ;
#9696 = CARTESIAN_POINT ( 'NONE',  ( 14.73750000122903359, 4.330127018922191873, 2.499999999999999556 ) ) ;
#9697 = CARTESIAN_POINT ( 'NONE',  ( 21.97500000000000142, -4.330127018922194537, 2.499999999999995559 ) ) ;
#9698 = CARTESIAN_POINT ( 'NONE',  ( 2.121784821875001281, 17.25312500061451715, -26.32496088578401938 ) ) ;
#9699 = CARTESIAN_POINT ( 'NONE',  ( 20.77500000000000213, 6.123233995736764310E-16, -4.999999999999998224 ) ) ;
#9700 = CARTESIAN_POINT ( 'NONE',  ( 24.01875000122903359, 2.886751345948142866, -4.999999999999973355 ) ) ;
#9701 = CARTESIAN_POINT ( 'NONE',  ( 29.65312500061451573, 4.541064518000418104, -2.621784821874998173 ) ) ;
#9702 = DIRECTION ( 'NONE',  ( -1.000000000000000000, -0.000000000000000000, -0.000000000000000000 ) ) ;
#9703 = CARTESIAN_POINT ( 'NONE',  ( 15.94687500061451502, -3.027376345333614438, 5.243569643749998122 ) ) ;
#9704 = CARTESIAN_POINT ( 'NONE',  ( 26.62500000000000000, 6.123233995736764310E-16, -4.999999999999998224 ) ) ;
#9705 = CARTESIAN_POINT ( 'NONE',  ( 11.20312500061451644, 4.541064518000418104, -2.621784821874998173 ) ) ;
#9706 = VECTOR ( 'NONE', #2051, 1000.000000000000000 ) ;
#9707 = CARTESIAN_POINT ( 'NONE',  ( 28.88437500061451502, -2.746126346562646425, 4.756430356249996549 ) ) ;
#9708 = CARTESIAN_POINT ( 'NONE',  ( 21.12187500061451573, 3.027376345333613106, -5.243569643749998122 ) ) ;
#9709 = CARTESIAN_POINT ( 'NONE',  ( 14.10937500061451644, -5.492252693125287522, -1.008910452111647106E-15 ) ) ;
#9710 = CARTESIAN_POINT ( 'NONE',  ( 6.515625000614516438, -6.054752690667223547, -1.112240025338166033E-15 ) ) ;
#9711 = CARTESIAN_POINT ( 'NONE',  ( 14.18437500061451750, -4.541064518000419881, 2.621784821874995952 ) ) ;
#9712 = ORIENTED_EDGE ( 'NONE', *, *, #8453, .F. ) ;
#9713 = CARTESIAN_POINT ( 'NONE',  ( 23.07187500061451857, 3.027376345333611329, 5.243569643749999010 ) ) ;
#9714 = CARTESIAN_POINT ( 'NONE',  ( 3.861486210907941086, 3.177525289277527420, -28.92245512961235576 ) ) ;
#9715 = ADVANCED_FACE ( 'NONE', ( #11042 ), #27315, .T. ) ;
#9716 = CARTESIAN_POINT ( 'NONE',  ( 24.71250000000000213, -5.773502691896255534, -1.060575238724906372E-15 ) ) ;
#9717 = CARTESIAN_POINT ( 'NONE',  ( 6.524999999999999467, 4.330127018922191873, 2.499999999999999556 ) ) ;
#9718 = CARTESIAN_POINT ( 'NONE',  ( 16.46250000122903501, 4.330127018922192761, -2.499999999999997780 ) ) ;
#9719 = CARTESIAN_POINT ( 'NONE',  ( -1.487416814333745711E-14, 16.62500000122903288, 34.00000000000000000 ) ) ;
#9720 = CARTESIAN_POINT ( 'NONE',  ( 8.146875000614516082, 0.000000000000000000, 4.756430356249998326 ) ) ;
#9721 = ORIENTED_EDGE ( 'NONE', *, *, #25362, .T. ) ;
#9722 = CARTESIAN_POINT ( 'NONE',  ( 14.88750000000000107, -2.886751345948125991, -5.000000000000000000 ) ) ;
#9723 = CARTESIAN_POINT ( 'NONE',  ( 16.01249999999999929, 2.886751345948126879, 4.999999999999999112 ) ) ;
#9724 = CARTESIAN_POINT ( 'NONE',  ( 12.51562500061451821, 3.027376345333613106, -5.243569643749998122 ) ) ;
#9725 = ORIENTED_EDGE ( 'NONE', *, *, #38684, .F. ) ;
#9726 = CARTESIAN_POINT ( 'NONE',  ( -3.999999999999997335, 17.00000000122903288, -27.69059892324149530 ) ) ;
#9727 = CARTESIAN_POINT ( 'NONE',  ( 2.121784821875001281, 17.75937500061451502, -26.32496088578401938 ) ) ;
#9728 = CARTESIAN_POINT ( 'NONE',  ( 4.490625000614516971, 6.054752690667223547, 3.707466751127219781E-16 ) ) ;
#9729 = CARTESIAN_POINT ( 'NONE',  ( 1.878215178124997609, 14.36562499938548321, 33.25316411605952993 ) ) ;
#9730 = CARTESIAN_POINT ( 'NONE',  ( 10.95000000000000107, 4.330127018922192761, -2.499999999999997780 ) ) ;
#9731 = CARTESIAN_POINT ( 'NONE',  ( 3.046343057529203424, 3.964819538874875704, 3.046343057529141696 ) ) ;
#9732 = ORIENTED_EDGE ( 'NONE', *, *, #28241, .F. ) ;
#9733 = CARTESIAN_POINT ( 'NONE',  ( 2.121784821875001281, 11.85312500061451857, 33.67503911421598417 ) ) ;
#9734 = CARTESIAN_POINT ( 'NONE',  ( 23.39062500061451289, 6.054752690667223547, 3.707466751127219781E-16 ) ) ;
#9735 = CARTESIAN_POINT ( 'NONE',  ( 29.55000000000000071, 0.000000000000000000, 4.999999999999998224 ) ) ;
#9736 = CARTESIAN_POINT ( 'NONE',  ( -3.756430356249999214, 19.12812499938548427, 27.83122392262697531 ) ) ;
#9737 = CARTESIAN_POINT ( 'NONE',  ( 20.89687500061452141, -3.027376345333614438, 5.243569643749998122 ) ) ;
#9738 = CARTESIAN_POINT ( 'NONE',  ( 19.11562500061451431, -6.054752690667223547, -1.112240025338166033E-15 ) ) ;
#9739 = CARTESIAN_POINT ( 'NONE',  ( 2.121784821875001281, 13.65312500061459566, -26.32496088578401938 ) ) ;
#9740 = CARTESIAN_POINT ( 'NONE',  ( 24.07500000122903216, 2.886751345948129099, -4.999999999999998224 ) ) ;
#9741 = CARTESIAN_POINT ( 'NONE',  ( 3.890625000614517326, -3.027376345333610441, -5.243569643749999898 ) ) ;
#9742 = CARTESIAN_POINT ( 'NONE',  ( 24.00937500061451502, 0.000000000000000000, 4.756430356249998326 ) ) ;
#9743 = CARTESIAN_POINT ( 'NONE',  ( 20.95312500061451999, -4.541064518000417216, -2.621784821875001281 ) ) ;
#9744 = CARTESIAN_POINT ( 'NONE',  ( 8.221875000614518925, 2.746126346562643317, 4.756430356249998326 ) ) ;
#9745 = CARTESIAN_POINT ( 'NONE',  ( 1.878215178124997609, 19.31562499938548427, 33.25316411605952993 ) ) ;
#9746 = CARTESIAN_POINT ( 'NONE',  ( 15.94687500061451502, -3.027376345333614438, 5.243569643749998122 ) ) ;
#9747 = CARTESIAN_POINT ( 'NONE',  ( 13.84687500061451537, -3.027376345333610441, -5.243569643749999898 ) ) ;
#9748 = CARTESIAN_POINT ( 'NONE',  ( 21.64687500061451786, 6.054752690667223547, 3.707466751127219781E-16 ) ) ;
#9749 = CARTESIAN_POINT ( 'NONE',  ( 4.243569643749999898, 11.49687500061451928, 32.45002607614398471 ) ) ;
#9750 = CARTESIAN_POINT ( 'NONE',  ( 4.528125000614516615, 4.541064518000418104, 2.621784821874999949 ) ) ;
#9751 = CARTESIAN_POINT ( 'NONE',  ( 25.94062500061451715, -3.027376345333610441, -5.243569643749999898 ) ) ;
#9752 = CARTESIAN_POINT ( 'NONE',  ( 26.27812500061451573, -4.541064518000419881, 2.621784821874995952 ) ) ;
#9753 = DIRECTION ( 'NONE',  ( -1.000000000000000000, -0.000000000000000000, -0.000000000000000000 ) ) ;
#9754 = CARTESIAN_POINT ( 'NONE',  ( 7.275000000000000355, 6.123233995736764310E-16, -4.999999999999998224 ) ) ;
#9755 = CARTESIAN_POINT ( 'NONE',  ( 7.771875000614516971, 3.027376345333611329, 5.243569643749999010 ) ) ;
#9756 = SHAPE_DEFINITION_REPRESENTATION ( #20177, #25944 ) ;
#9757 = CARTESIAN_POINT ( 'NONE',  ( 14.06250000122903288, -4.330127018922190985, -2.500000000000001332 ) ) ;
#9758 = CARTESIAN_POINT ( 'NONE',  ( 10.46250000122903323, -4.330127018922190985, -2.500000000000001332 ) ) ;
#9759 = CARTESIAN_POINT ( 'NONE',  ( 3.703125000614516882, 0.000000000000000000, 5.243569643749999010 ) ) ;
#9760 = CARTESIAN_POINT ( 'NONE',  ( -3.999999999999999556, 15.33124999877096606, 27.69059892324149175 ) ) ;
#9761 = CARTESIAN_POINT ( 'NONE',  ( 18.24375000122903501, 5.773502691896255534, 3.535250795749688894E-16 ) ) ;
#9762 = CARTESIAN_POINT ( 'NONE',  ( 13.73437500061451821, -4.541064518000419881, 2.621784821874995952 ) ) ;
#9763 = CARTESIAN_POINT ( 'NONE',  ( 1.510657702057710734E-15, 19.10000000122903430, -33.99999999999999289 ) ) ;
#9764 = VERTEX_POINT ( 'NONE', #28397 ) ;
#9765 = CARTESIAN_POINT ( 'NONE',  ( 20.39062500061451644, -3.027376345333614438, 5.243569643749998122 ) ) ;
#9766 = CARTESIAN_POINT ( 'NONE',  ( 6.215625000614517504, 3.027376345333613106, -5.243569643749998122 ) ) ;
#9767 = CARTESIAN_POINT ( 'NONE',  ( 24.98437500061451644, -4.541064518000419881, 2.621784821874995952 ) ) ;
#9768 = CARTESIAN_POINT ( 'NONE',  ( 8.428125000614517859, 6.421520780324663323E-16, -5.243569643749999010 ) ) ;
#9769 = CYLINDRICAL_SURFACE ( 'NONE', #68674, 4.999999999999998224 ) ;
#9770 =( BOUNDED_CURVE ( )  B_SPLINE_CURVE ( 2, ( #41492, #64012, #13392, #35937, #58460, #7871, #30407 ),
 .UNSPECIFIED., .F., .F. ) 
 B_SPLINE_CURVE_WITH_KNOTS ( ( 3, 2, 2, 3 ),
 ( 0.4916666666666666408, 0.4944444444444444642, 0.4972222222222222321, 0.5000000000000000000 ),
 .UNSPECIFIED. ) 
 CURVE ( )  GEOMETRIC_REPRESENTATION_ITEM ( )  RATIONAL_B_SPLINE_CURVE ( ( 1.000000000000000000, 0.8660254037844387076, 1.000000000000000000, 0.8660254037844387076, 1.000000000000000000, 0.8660254037844387076, 1.000000000000000000 ) ) 
 REPRESENTATION_ITEM ( '' )  );
#9771 = CARTESIAN_POINT ( 'NONE',  ( 7.162500001229032520, 0.000000000000000000, 4.999999999999998224 ) ) ;
#9772 = CARTESIAN_POINT ( 'NONE',  ( 22.34062500061451573, -3.027376345333610441, -5.243569643749999898 ) ) ;
#9773 = CARTESIAN_POINT ( 'NONE',  ( -2.828200636599751609E-16, 18.20000000122903216, -34.61880215351700230 ) ) ;
#9774 = CARTESIAN_POINT ( 'NONE',  ( 9.862500001229033586, 0.000000000000000000, 4.999999999999998224 ) ) ;
#9775 = CARTESIAN_POINT ( 'NONE',  ( 19.00312500061451715, 0.000000000000000000, 5.243569643749999010 ) ) ;
#9776 = CARTESIAN_POINT ( 'NONE',  ( 15.44062500061451537, -3.027376345333614438, 5.243569643749998122 ) ) ;
#9777 = CARTESIAN_POINT ( 'NONE',  ( 28.02187500061451431, 2.746126346562643317, 4.756430356249998326 ) ) ;
#9778 = CARTESIAN_POINT ( 'NONE',  ( 15.56250000000000000, 2.886751345948126879, 4.999999999999999112 ) ) ;
#9779 = CARTESIAN_POINT ( 'NONE',  ( 12.03750000122903430, 4.330127018922191873, 2.499999999999999556 ) ) ;
#9780 = CARTESIAN_POINT ( 'NONE',  ( 9.103125000614515017, 0.000000000000000000, 5.243569643749999010 ) ) ;
#9781 = CARTESIAN_POINT ( 'NONE',  ( 10.56562500061451715, -6.054752690667223547, -1.112240025338166033E-15 ) ) ;
#9782 = EDGE_CURVE ( 'NONE', #40370, #8399, #66844, .T. ) ;
#9783 = CARTESIAN_POINT ( 'NONE',  ( 20.43750000122903643, 6.123233995736764310E-16, -4.999999999999998224 ) ) ;
#9784 = CARTESIAN_POINT ( 'NONE',  ( 18.98437500061451644, 4.541064518000418104, 2.621784821874999949 ) ) ;
#9785 = CARTESIAN_POINT ( 'NONE',  ( 4.655204990825274614, -3.615897911723494840, 4.224220389412703724 ) ) ;
#9786 = CARTESIAN_POINT ( 'NONE',  ( 5.925000001229033586, -5.773502691896255534, -1.060575238724906372E-15 ) ) ;
#9787 = CARTESIAN_POINT ( 'NONE',  ( 3.834375000614519635, -4.541064518000419881, 2.621784821874995952 ) ) ;
#9788 = CARTESIAN_POINT ( 'NONE',  ( 22.09687500061451715, 6.054752690667223547, 3.707466751127219781E-16 ) ) ;
#9789 = CARTESIAN_POINT ( 'NONE',  ( -1.071796769724496556, 15.14240381056766616, 33.99999999999998579 ) ) ;
#9790 = CARTESIAN_POINT ( 'NONE',  ( 18.51562500061451289, 3.027376345333611329, 5.243569643749999010 ) ) ;
#9791 = CARTESIAN_POINT ( 'NONE',  ( 23.22187500061451715, -6.054752690667223547, -1.112240025338166033E-15 ) ) ;
#9792 = CARTESIAN_POINT ( 'NONE',  ( 1.878215178124997609, 18.97812499938548214, 33.25316411605952993 ) ) ;
#9793 = CARTESIAN_POINT ( 'NONE',  ( -2.000000000000000000, 11.03750000122903430, -33.46410161513775705 ) ) ;
#9794 = CARTESIAN_POINT ( 'NONE',  ( 27.72187500061451715, -6.054752690667223547, -1.112240025338166033E-15 ) ) ;
#9795 = CARTESIAN_POINT ( 'NONE',  ( 20.63437500061451502, 5.492252693125287522, 3.363034840372157021E-16 ) ) ;
#9796 = CARTESIAN_POINT ( 'NONE',  ( 14.35312500061451679, 4.541064518000418104, -2.621784821874998173 ) ) ;
#9797 = CARTESIAN_POINT ( 'NONE',  ( 12.53437500061451537, 6.421520780324663323E-16, -5.243569643749999010 ) ) ;
#9798 = ORIENTED_EDGE ( 'NONE', *, *, #56271, .F. ) ;
#9799 = CARTESIAN_POINT ( 'NONE',  ( 13.35000000000000142, 0.000000000000000000, 4.999999999999998224 ) ) ;
#9800 = CARTESIAN_POINT ( 'NONE',  ( 22.00312500061451360, 4.541064518000418104, -2.621784821874998173 ) ) ;
#9801 = CARTESIAN_POINT ( 'NONE',  ( 1.999999999999998668, 17.15000000000000213, 26.53589838486224650 ) ) ;
#9802 = CARTESIAN_POINT ( 'NONE',  ( 14.47499999999999964, 6.123233995736764310E-16, -4.999999999999998224 ) ) ;
#9803 = CARTESIAN_POINT ( 'NONE',  ( 14.62500000000000000, 4.330127018922191873, 2.499999999999999556 ) ) ;
#9804 = CARTESIAN_POINT ( 'NONE',  ( 23.77500000122903145, 2.886751345948126879, 4.999999999999999112 ) ) ;
#9805 = CARTESIAN_POINT ( 'NONE',  ( 19.11562500061451431, -6.054752690667223547, -1.112240025338166033E-15 ) ) ;
#9806 = ORIENTED_EDGE ( 'NONE', *, *, #49507, .F. ) ;
#9807 = CARTESIAN_POINT ( 'NONE',  ( 21.67500000000000071, 6.123233995736764310E-16, -4.999999999999998224 ) ) ;
#9808 =( BOUNDED_CURVE ( )  B_SPLINE_CURVE ( 2, ( #8517, #8888, #63571, #12959, #35496, #69493, #58016 ),
 .UNSPECIFIED., .F., .F. ) 
 B_SPLINE_CURVE_WITH_KNOTS ( ( 3, 2, 2, 3 ),
 ( 0.6916666666666666519, 0.6944444444444444198, 0.6972222222222221877, 0.6999999999999999556 ),
 .UNSPECIFIED. ) 
 CURVE ( )  GEOMETRIC_REPRESENTATION_ITEM ( )  RATIONAL_B_SPLINE_CURVE ( ( 1.000000000000000000, 0.8660254037844387076, 1.000000000000000000, 0.8660254037844387076, 1.000000000000000000, 0.8660254037844387076, 1.000000000000000000 ) ) 
 REPRESENTATION_ITEM ( '' )  );
#9809 = CARTESIAN_POINT ( 'NONE',  ( 24.19687500061451857, -3.027376345333610441, -5.243569643749999898 ) ) ;
#9810 = EDGE_LOOP ( 'NONE', ( #28610, #60092, #63638, #63542, #4644, #38636, #26963, #63152 ) ) ;
#9811 = CARTESIAN_POINT ( 'NONE',  ( 19.20000000000000284, 0.000000000000000000, 4.999999999999998224 ) ) ;
#9812 = CARTESIAN_POINT ( 'NONE',  ( 10.11562500061451608, -6.054752690667223547, -1.112240025338166033E-15 ) ) ;
#9813 = CARTESIAN_POINT ( 'NONE',  ( 4.453125000614517326, 4.541064518000418104, -2.621784821874998173 ) ) ;
#9814 = CARTESIAN_POINT ( 'NONE',  ( 14.14687500061451431, -4.119189519843965641, -2.378215178125001383 ) ) ;
#9815 = CARTESIAN_POINT ( 'NONE',  ( 27.74062500061451431, -3.027376345333610441, -5.243569643749999898 ) ) ;
#9816 = CARTESIAN_POINT ( 'NONE',  ( 16.31250000000000000, 2.886751345948129099, -4.999999999999998224 ) ) ;
#9817 = CARTESIAN_POINT ( 'NONE',  ( 23.85000000000000142, -4.330127018922190985, -2.500000000000001332 ) ) ;
#9818 = CARTESIAN_POINT ( 'NONE',  ( 2.121784821875001281, 19.05312500061451431, 33.67503911421598417 ) ) ;
#9819 = CARTESIAN_POINT ( 'NONE',  ( 5.859375000614519102, 4.541064518000418104, -2.621784821874998173 ) ) ;
#9820 = CARTESIAN_POINT ( 'NONE',  ( 17.25937500061451502, 0.000000000000000000, 5.243569643749999010 ) ) ;
#9821 = CARTESIAN_POINT ( 'NONE',  ( 28.88437500061451502, 4.541064518000418104, 2.621784821874999949 ) ) ;
#9822 = ORIENTED_EDGE ( 'NONE', *, *, #47475, .T. ) ;
#9823 = CARTESIAN_POINT ( 'NONE',  ( 27.44062500061451715, 6.054752690667223547, 3.707466751127219781E-16 ) ) ;
#9824 = CARTESIAN_POINT ( 'NONE',  ( 27.12187500061451573, 3.027376345333611329, 5.243569643749999010 ) ) ;
#9826 = ADVANCED_FACE ( 'NONE', ( #67212 ), #50935, .F. ) ;
#9825 = CARTESIAN_POINT ( 'NONE',  ( 2.934375000614518392, -4.541064518000419881, 2.621784821874995952 ) ) ;
#9827 = AXIS2_PLACEMENT_3D ( 'NONE', #36442, #47899, #72255 ) ;
#9828 = CARTESIAN_POINT ( 'NONE',  ( 14.21249999999999858, 2.886751345948126879, 4.999999999999999112 ) ) ;
#9829 = CARTESIAN_POINT ( 'NONE',  ( 11.46562500061451573, -6.054752690667223547, -1.112240025338166033E-15 ) ) ;
#9830 = CYLINDRICAL_SURFACE ( 'NONE', #59888, 4.999999999999998224 ) ;
#9831 = CARTESIAN_POINT ( 'NONE',  ( 0.000000000000000000, 20.00000000000000000, -33.99999999999999289 ) ) ;
#9832 = CARTESIAN_POINT ( 'NONE',  ( 29.72812500061451502, 4.541064518000418104, 2.621784821874999949 ) ) ;
#9833 = CARTESIAN_POINT ( 'NONE',  ( 16.87500000122903288, 2.886751345948129099, -4.999999999999998224 ) ) ;
#9834 = DIRECTION ( 'NONE',  ( 0.000000000000000000, 0.000000000000000000, -1.000000000000000000 ) ) ;
#9835 = CARTESIAN_POINT ( 'NONE',  ( 15.87187500061451573, 2.746126346562643317, 4.756430356249998326 ) ) ;
#9836 = CARTESIAN_POINT ( 'NONE',  ( 6.440625000614517148, -3.027376345333614438, 5.243569643749998122 ) ) ;
#9837 = CARTESIAN_POINT ( 'NONE',  ( 20.74687500061451573, 6.054752690667223547, 3.707466751127219781E-16 ) ) ;
#9838 = CARTESIAN_POINT ( 'NONE',  ( 4.243569643749999010, 16.52187500061451786, 27.54997392385601174 ) ) ;
#9839 = CARTESIAN_POINT ( 'NONE',  ( 21.08437500061451786, 6.421520780324663323E-16, -5.243569643749999010 ) ) ;
#9840 = CARTESIAN_POINT ( 'NONE',  ( 6.225000000000001421, -4.330127018922194537, 2.499999999999995559 ) ) ;
#9841 = CARTESIAN_POINT ( 'NONE',  ( 2.121784821874999061, 19.70937500061451786, 26.32496088578401583 ) ) ;
#9842 = CARTESIAN_POINT ( 'NONE',  ( 12.06562500061451537, 3.027376345333613106, -5.243569643749998122 ) ) ;
#9843 = CARTESIAN_POINT ( 'NONE',  ( 5.512500001229033941, -4.330127018922190985, -2.500000000000001332 ) ) ;
#9844 = CARTESIAN_POINT ( 'NONE',  ( 8.259375000614518569, 0.000000000000000000, 5.243569643749999010 ) ) ;
#9845 = DIRECTION ( 'NONE',  ( 0.000000000000000000, 0.000000000000000000, -1.000000000000000000 ) ) ;
#9846 = CARTESIAN_POINT ( 'NONE',  ( 9.028125000614517504, 4.541064518000418104, 2.621784821874999949 ) ) ;
#9847 = CARTESIAN_POINT ( 'NONE',  ( 13.88437500061451679, 6.421520780324663323E-16, -5.243569643749999010 ) ) ;
#9848 = CARTESIAN_POINT ( 'NONE',  ( 3.456510739548324551, -3.612829017181165892, -3.800327499238720819 ) ) ;
#9849 = CARTESIAN_POINT ( 'NONE',  ( 20.77500000122903145, -5.773502691896255534, -1.060575238724906372E-15 ) ) ;
#9850 = CARTESIAN_POINT ( 'NONE',  ( 7.846875000614518036, -3.027376345333614438, 5.243569643749998122 ) ) ;
#9851 = CARTESIAN_POINT ( 'NONE',  ( 11.61562500061451608, 3.027376345333613106, -5.243569643749998122 ) ) ;
#9852 = CARTESIAN_POINT ( 'NONE',  ( 24.91875000122902861, 2.886751345948129099, -4.999999999999998224 ) ) ;
#9853 = CARTESIAN_POINT ( 'NONE',  ( 21.57187500061451502, 3.027376345333613106, -5.243569643749998122 ) ) ;
#9854 = CARTESIAN_POINT ( 'NONE',  ( 45.00000000000000000, 1.494782592887780703, 8.874999999999982236 ) ) ;
#9855 = CARTESIAN_POINT ( 'NONE',  ( -3.183805653906653266, 3.859810113929996067, 27.56566125170668258 ) ) ;
#9856 = CARTESIAN_POINT ( 'NONE',  ( -3.999999999999999112, 20.00000000000000000, -30.00000000000000000 ) ) ;
#9857 = CARTESIAN_POINT ( 'NONE',  ( -4.243569643749999898, 11.27187500061451786, -32.45002607614398471 ) ) ;
#9858 = CARTESIAN_POINT ( 'NONE',  ( 14.77500000122903501, 2.886751345948126879, 4.999999999999999112 ) ) ;
#9859 = CARTESIAN_POINT ( 'NONE',  ( 4.243569643749999898, 15.94062500061451537, -27.54997392385601529 ) ) ;
#9860 = CARTESIAN_POINT ( 'NONE',  ( 18.33750000122903501, 4.330127018922191873, 2.499999999999999556 ) ) ;
#9861 = CARTESIAN_POINT ( 'NONE',  ( 9.028125000614517504, 4.541064518000418104, 2.621784821874999949 ) ) ;
#9862 = ORIENTED_EDGE ( 'NONE', *, *, #2528, .F. ) ;
#9863 = CARTESIAN_POINT ( 'NONE',  ( 16.42500000000000071, 4.330127018922191873, 2.499999999999999556 ) ) ;
#9864 = CARTESIAN_POINT ( 'NONE',  ( 45.00000000000000000, 6.123233995736764310E-16, -4.999999999999998224 ) ) ;
#9865 = CARTESIAN_POINT ( 'NONE',  ( 23.95312500061451289, 0.000000000000000000, 5.243569643749999010 ) ) ;
#9866 = CARTESIAN_POINT ( 'NONE',  ( 10.02187500061451964, 3.027376345333611329, 5.243569643749999010 ) ) ;
#9867 = CARTESIAN_POINT ( 'NONE',  ( 4.000000000000000000, 16.94374999877096499, 30.00000000000000000 ) ) ;
#9868 = CARTESIAN_POINT ( 'NONE',  ( 9.862500001229033586, 0.000000000000000000, 4.999999999999998224 ) ) ;
#9869 = CARTESIAN_POINT ( 'NONE',  ( 19.23750000122903714, 4.330127018922191873, 2.499999999999999556 ) ) ;
#9870 = CARTESIAN_POINT ( 'NONE',  ( 15.17812500061451608, 6.421520780324663323E-16, -5.243569643749999010 ) ) ;
#9871 = CARTESIAN_POINT ( 'NONE',  ( 17.65312500061451573, 0.000000000000000000, 5.243569643749999010 ) ) ;
#9872 = CARTESIAN_POINT ( 'NONE',  ( 24.67500000122903359, 2.886751345948126879, 4.999999999999999112 ) ) ;
#9873 = CARTESIAN_POINT ( 'NONE',  ( 29.32500000122903216, -5.773502691896255534, -1.060575238724906372E-15 ) ) ;
#9874 = CARTESIAN_POINT ( 'NONE',  ( 26.32499999999999929, 4.330127018922191873, 2.499999999999999556 ) ) ;
#9875 = CARTESIAN_POINT ( 'NONE',  ( -1.878215178124999163, 14.59062499938548463, 26.74683588394047007 ) ) ;
#9876 = CARTESIAN_POINT ( 'NONE',  ( 26.82187500061451857, -6.054752690667223547, -1.112240025338166033E-15 ) ) ;
#9877 = CARTESIAN_POINT ( 'NONE',  ( 26.45625000122903003, 0.000000000000000000, 4.999999999999998224 ) ) ;
#9878 = CARTESIAN_POINT ( 'NONE',  ( 12.45000000122903394, 5.773502691896255534, 3.535250795749688894E-16 ) ) ;
#9879 = CARTESIAN_POINT ( 'NONE',  ( 3.562500000000000444, -5.773502691896255534, -1.060575238724906372E-15 ) ) ;
#9880 = EDGE_CURVE ( 'NONE', #49995, #52378, #66590, .T. ) ;
#9881 = FACE_OUTER_BOUND ( 'NONE', #12309, .T. ) ;
#9882 = CARTESIAN_POINT ( 'NONE',  ( 6.421875000614519102, 3.027376345333611329, 5.243569643749999010 ) ) ;
#9883 = CARTESIAN_POINT ( 'NONE',  ( 27.25312500061451360, -4.541064518000417216, -2.621784821875001281 ) ) ;
#9884 = CARTESIAN_POINT ( 'NONE',  ( 1.878215178125000495, 12.82812499938548356, 26.74683588394047007 ) ) ;
#9885 = CARTESIAN_POINT ( 'NONE',  ( 3.999999999999998668, 10.47500000122903430, 27.69059892324149530 ) ) ;
#9886 = CARTESIAN_POINT ( 'NONE',  ( 3.662819313031858925, -3.403491542531015046, 3.773569494236241439 ) ) ;
#9887 = CARTESIAN_POINT ( 'NONE',  ( 5.409375000614516260, 4.541064518000418104, -2.621784821874998173 ) ) ;
#9888 = CARTESIAN_POINT ( 'NONE',  ( 9.834375000614517859, 6.421520780324663323E-16, -5.243569643749999010 ) ) ;
#9889 = CARTESIAN_POINT ( 'NONE',  ( 29.63437500061451502, 6.421520780324663323E-16, -5.243569643749999010 ) ) ;
#9890 = CARTESIAN_POINT ( 'NONE',  ( -2.121784821874999949, 12.52812500061459211, 26.32496088578401938 ) ) ;
#9891 = CARTESIAN_POINT ( 'NONE',  ( 21.37499999999999645, 4.330127018922191873, 2.499999999999999556 ) ) ;
#9892 = CARTESIAN_POINT ( 'NONE',  ( 28.61249999999999716, 2.886751345948126879, 4.999999999999999112 ) ) ;
#9893 = CARTESIAN_POINT ( 'NONE',  ( 4.462500000000001243, -5.773502691896255534, -1.060575238724906372E-15 ) ) ;
#9894 = EDGE_LOOP ( 'NONE', ( #48810, #60628, #27456, #29996 ) ) ;
#9895 = CARTESIAN_POINT ( 'NONE',  ( 17.99062500061451786, 6.054752690667223547, 3.707466751127219781E-16 ) ) ;
#9896 = CARTESIAN_POINT ( 'NONE',  ( 11.39062500061451644, -3.027376345333614438, 5.243569643749998122 ) ) ;
#9897 = CARTESIAN_POINT ( 'NONE',  ( 22.32187500061451502, 5.824947211148865298E-16, -4.756430356249998326 ) ) ;
#9898 = CARTESIAN_POINT ( 'NONE',  ( 7.321875000614516793, 3.027376345333611329, 5.243569643749999010 ) ) ;
#9899 = CARTESIAN_POINT ( 'NONE',  ( 23.21250000000000213, 2.886751345948126879, 4.999999999999999112 ) ) ;
#9900 = CARTESIAN_POINT ( 'NONE',  ( 20.43750000122903643, 6.123233995736764310E-16, -4.999999999999998224 ) ) ;
#9901 = CARTESIAN_POINT ( 'NONE',  ( 1.999999999999997335, 19.62500000000000000, 33.46410161513775705 ) ) ;
#9902 = CARTESIAN_POINT ( 'NONE',  ( 5.971875000614516260, 3.027376345333611329, 5.243569643749999010 ) ) ;
#9903 = CARTESIAN_POINT ( 'NONE',  ( 12.98437500061451821, 6.421520780324663323E-16, -5.243569643749999010 ) ) ;
#9904 = CARTESIAN_POINT ( 'NONE',  ( 23.78437500061451360, 6.421520780324663323E-16, -5.243569643749999010 ) ) ;
#9905 = CARTESIAN_POINT ( 'NONE',  ( -1.071796769724488563, 16.49240381056766580, 34.00000000000000000 ) ) ;
#9906 = VERTEX_POINT ( 'NONE', #55748 ) ;
#9907 = CARTESIAN_POINT ( 'NONE',  ( 12.30000000000000249, 4.330127018922192761, -2.499999999999997780 ) ) ;
#9908 = CARTESIAN_POINT ( 'NONE',  ( 18.15937500061451715, 0.000000000000000000, 5.243569643749999010 ) ) ;
#9909 = CARTESIAN_POINT ( 'NONE',  ( 9.571875000614518569, 3.027376345333611329, 5.243569643749999010 ) ) ;
#9910 = CARTESIAN_POINT ( 'NONE',  ( -1.878215178125001827, 14.74062499938548321, 33.25316411605952283 ) ) ;
#9911 = CARTESIAN_POINT ( 'NONE',  ( 21.11249999999999716, -5.773502691896255534, -1.060575238724906372E-15 ) ) ;
#9912 = CARTESIAN_POINT ( 'NONE',  ( 4.000000000000000000, 14.33750000000000213, 27.69059892324149530 ) ) ;
#9913 = CARTESIAN_POINT ( 'NONE',  ( -1.999999999999999112, 17.14999999999999858, 26.53589838486224650 ) ) ;
#9914 = CARTESIAN_POINT ( 'NONE',  ( 23.14687500061451786, -2.746126346562646425, 4.756430356249996549 ) ) ;
#9915 = CARTESIAN_POINT ( 'NONE',  ( 12.81562500061451537, -6.054752690667223547, -1.112240025338166033E-15 ) ) ;
#9916 = CARTESIAN_POINT ( 'NONE',  ( 28.99687500061451573, -3.027376345333614438, 5.243569643749998122 ) ) ;
#9917 = CARTESIAN_POINT ( 'NONE',  ( 6.862500001229034474, -4.330127018922190985, -2.500000000000001332 ) ) ;
#9918 = CARTESIAN_POINT ( 'NONE',  ( 28.43437500061451573, 4.541064518000418104, 2.621784821874999949 ) ) ;
#9919 = CARTESIAN_POINT ( 'NONE',  ( 11.43750000000000000, 5.773502691896255534, 3.535250795749688894E-16 ) ) ;
#9920 = CARTESIAN_POINT ( 'NONE',  ( -2.828200636599751609E-16, 16.85000000122903430, 25.38119784648299770 ) ) ;
#9921 = CARTESIAN_POINT ( 'NONE',  ( 12.33750000122903145, 6.123233995736764310E-16, -4.999999999999998224 ) ) ;
#9922 = CARTESIAN_POINT ( 'NONE',  ( 23.55937500061451573, 0.000000000000000000, 5.243569643749999010 ) ) ;
#9923 = CARTESIAN_POINT ( 'NONE',  ( 17.29687500061451999, -3.027376345333614438, 5.243569643749998122 ) ) ;
#9924 = CARTESIAN_POINT ( 'NONE',  ( 4.003212292754231072, 2.995723341028087017, -4.303571541022567892 ) ) ;
#9925 = ORIENTED_EDGE ( 'NONE', *, *, #54220, .F. ) ;
#9926 = VECTOR ( 'NONE', #65748, 1000.000000000000000 ) ;
#9927 = CARTESIAN_POINT ( 'NONE',  ( 16.15312500061451573, 4.541064518000418104, -2.621784821874998173 ) ) ;
#9928 = CARTESIAN_POINT ( 'NONE',  ( 29.02500000122903145, 2.886751345948129099, -4.999999999999998224 ) ) ;
#9929 = CARTESIAN_POINT ( 'NONE',  ( 18.08437500061451431, 4.541064518000418104, 2.621784821874999949 ) ) ;
#9930 = CARTESIAN_POINT ( 'NONE',  ( 5.672204065618859481, 8.235970573989483512, -28.03398296844422433 ) ) ;
#9931 = CARTESIAN_POINT ( 'NONE',  ( 20.05312500061451431, -4.541064518000417216, -2.621784821875001281 ) ) ;
#9932 = DIRECTION ( 'NONE',  ( -1.000000000000000000, -0.000000000000000000, -0.000000000000000000 ) ) ;
#9933 = EDGE_CURVE ( 'NONE', #57422, #50074, #15216, .T. ) ;
#9934 = CARTESIAN_POINT ( 'NONE',  ( 29.63437500061451502, 6.421520780324663323E-16, -5.243569643749999010 ) ) ;
#9935 = CARTESIAN_POINT ( 'NONE',  ( 4.243569643749999010, 11.96562500061451750, 27.54997392385601174 ) ) ;
#9936 = CARTESIAN_POINT ( 'NONE',  ( 17.59687500061451715, 6.054752690667223547, 3.707466751127219781E-16 ) ) ;
#9937 = CARTESIAN_POINT ( 'NONE',  ( 16.83750000122903145, 6.123233995736764310E-16, -4.999999999999998224 ) ) ;
#9938 = CARTESIAN_POINT ( 'NONE',  ( 10.65937500061451715, -4.119189519843965641, -2.378215178125001383 ) ) ;
#9939 = CARTESIAN_POINT ( 'NONE',  ( 9.001249775931846008E-16, 19.52187500061451786, -25.09994784771203058 ) ) ;
#9940 = CARTESIAN_POINT ( 'NONE',  ( 19.88437500061451857, 4.541064518000418104, 2.621784821874999949 ) ) ;
#9941 = CARTESIAN_POINT ( 'NONE',  ( 21.48750000122903003, 4.330127018922191873, 2.499999999999999556 ) ) ;
#9942 = CARTESIAN_POINT ( 'NONE',  ( 22.71562500061451573, -6.054752690667223547, -1.112240025338166033E-15 ) ) ;
#9943 = CARTESIAN_POINT ( 'NONE',  ( 18.08437500061451431, 4.541064518000418104, 2.621784821874999949 ) ) ;
#9944 = CARTESIAN_POINT ( 'NONE',  ( 11.24062500061451608, 6.054752690667223547, 3.707466751127219781E-16 ) ) ;
#9945 = CARTESIAN_POINT ( 'NONE',  ( 9.001249775931846008E-16, 13.67187500061451999, 34.90005215228797653 ) ) ;
#9946 = CARTESIAN_POINT ( 'NONE',  ( 16.60312500061451857, 4.541064518000418104, -2.621784821874998173 ) ) ;
#9947 = ORIENTED_EDGE ( 'NONE', *, *, #64920, .F. ) ;
#9948 = ORIENTED_EDGE ( 'NONE', *, *, #1146, .F. ) ;
#9949 = CARTESIAN_POINT ( 'NONE',  ( 22.05000000000000071, -4.330127018922190985, -2.500000000000001332 ) ) ;
#9950 = CARTESIAN_POINT ( 'NONE',  ( -3.000416591977282496E-16, 19.29687500061451644, -34.90005215228797653 ) ) ;
#9951 = CARTESIAN_POINT ( 'NONE',  ( 12.52500000000000213, -4.330127018922194537, 2.499999999999995559 ) ) ;
#9952 = B_SPLINE_CURVE_WITH_KNOTS ( 'NONE', 3,
 ( #5623, #5978, #1170, #17050, #17412, #62843, #40321, #51046, #33685, #23317 ),
 .UNSPECIFIED., .F., .F.,
 ( 4, 3, 3, 4 ),
 ( 1.952816364424374816E-16, 2.904775715151696798E-05, 7.262233730042978481E-05, 0.0001161998171129827076 ),
 .UNSPECIFIED. ) ;
#9953 = CARTESIAN_POINT ( 'NONE',  ( 23.57812500061451289, -4.541064518000419881, 2.621784821874995952 ) ) ;
#9954 = CARTESIAN_POINT ( 'NONE',  ( 6.365625000614518747, 3.027376345333611329, 5.243569643749999010 ) ) ;
#9955 = CARTESIAN_POINT ( 'NONE',  ( 18.22500000122903430, 2.886751345948129099, -4.999999999999998224 ) ) ;
#9956 = CARTESIAN_POINT ( 'NONE',  ( 23.31562500061451715, 3.027376345333613106, -5.243569643749998122 ) ) ;
#9957 = CARTESIAN_POINT ( 'NONE',  ( 22.31250000000000000, 2.886751345948126879, 4.999999999999999112 ) ) ;
#9958 = CARTESIAN_POINT ( 'NONE',  ( 26.50312500061451360, 4.541064518000418104, -2.621784821874998173 ) ) ;
#9959 = CARTESIAN_POINT ( 'NONE',  ( 8.653125000614515727, 0.000000000000000000, 5.243569643749999010 ) ) ;
#9960 = ORIENTED_EDGE ( 'NONE', *, *, #16624, .T. ) ;
#9961 = CARTESIAN_POINT ( 'NONE',  ( 22.49062500061451431, 6.054752690667223547, 3.707466751127219781E-16 ) ) ;
#9962 = CARTESIAN_POINT ( 'NONE',  ( 3.140625000614516882, 6.054752690667223547, 3.707466751127219781E-16 ) ) ;
#9963 = CARTESIAN_POINT ( 'NONE',  ( 10.95937500061451964, 0.000000000000000000, 4.756430356249998326 ) ) ;
#9964 = CARTESIAN_POINT ( 'NONE',  ( -3.999999999999999112, 11.07500000122903394, 27.69059892324149885 ) ) ;
#9965 = CARTESIAN_POINT ( 'NONE',  ( 4.000000000000000000, 14.90000000122903323, -27.69059892324149530 ) ) ;
#9966 = CARTESIAN_POINT ( 'NONE',  ( 2.000000000000000444, 12.96874999877096712, 26.53589838486224650 ) ) ;
#9967 = EDGE_CURVE ( 'NONE', #18378, #5961, #21389, .T. ) ;
#9968 = CARTESIAN_POINT ( 'NONE',  ( 10.68750000000000000, -2.886751345948129988, 4.999999999999997335 ) ) ;
#9969 = CARTESIAN_POINT ( 'NONE',  ( 11.59687500061451892, -3.027376345333610441, -5.243569643749999898 ) ) ;
#9970 = CARTESIAN_POINT ( 'NONE',  ( 7.012500001229035718, 4.330127018922192761, -2.499999999999997780 ) ) ;
#9971 = CARTESIAN_POINT ( 'NONE',  ( 15.79687500061451821, 6.054752690667223547, 3.707466751127219781E-16 ) ) ;
#9972 = CARTESIAN_POINT ( 'NONE',  ( 6.421875000614519102, 3.027376345333611329, 5.243569643749999010 ) ) ;
#9973 = CARTESIAN_POINT ( 'NONE',  ( -2.121784821874999949, 9.828125000614516438, -33.67503911421598417 ) ) ;
#9974 = CARTESIAN_POINT ( 'NONE',  ( -1.071796769724491005, 10.57009619066136707, 26.00000000000000355 ) ) ;
#9975 = CARTESIAN_POINT ( 'NONE',  ( 13.47187500061451537, 3.027376345333613106, -5.243569643749998122 ) ) ;
#9976 = CARTESIAN_POINT ( 'NONE',  ( 0.000000000000000000, 27.50000000000000000, 26.00000000000000000 ) ) ;
#9977 = CARTESIAN_POINT ( 'NONE',  ( 21.55312500061451431, 4.541064518000418104, -2.621784821874998173 ) ) ;
#9978 = DIRECTION ( 'NONE',  ( -1.000000000000000000, -0.000000000000000000, -0.000000000000000000 ) ) ;
#9979 = CARTESIAN_POINT ( 'NONE',  ( 2.121784821874999061, 19.20312500061459460, 26.32496088578401583 ) ) ;
#9980 = CARTESIAN_POINT ( 'NONE',  ( 23.22187500061451715, -6.054752690667223547, -1.112240025338166033E-15 ) ) ;
#9981 = CARTESIAN_POINT ( 'NONE',  ( -3.999999999999997335, 13.85000000122903607, -27.69059892324149530 ) ) ;
#9982 = CARTESIAN_POINT ( 'NONE',  ( 28.98750000122903359, 6.123233995736764310E-16, -4.999999999999998224 ) ) ;
#9983 = AXIS2_PLACEMENT_3D ( 'NONE', #71711, #4116, #72428 ) ;
#9984 = CARTESIAN_POINT ( 'NONE',  ( 19.47187500061451360, -4.119189519843968306, 2.378215178124996054 ) ) ;
#9985 = VECTOR ( 'NONE', #49874, 1000.000000000000000 ) ;
#9986 = CARTESIAN_POINT ( 'NONE',  ( 25.41562500061451146, -6.054752690667223547, -1.112240025338166033E-15 ) ) ;
#9987 = CARTESIAN_POINT ( 'NONE',  ( 18.66562500061451146, -6.054752690667223547, -1.112240025338166033E-15 ) ) ;
#9988 = CARTESIAN_POINT ( 'NONE',  ( 15.01875000122903181, 2.886751345948129099, -4.999999999999998224 ) ) ;
#9989 = CARTESIAN_POINT ( 'NONE',  ( 14.82187500061451679, 3.027376345333613106, -5.243569643749998122 ) ) ;
#9990 = CARTESIAN_POINT ( 'NONE',  ( 7.284375000614518036, -2.746126346562646425, 4.756430356249996549 ) ) ;
#9991 = CARTESIAN_POINT ( 'NONE',  ( 26.92500000122903359, 2.886751345948126879, 4.999999999999999112 ) ) ;
#9992 = CARTESIAN_POINT ( 'NONE',  ( 4.846875000614519813, -3.027376345333610441, -5.243569643749999898 ) ) ;
#9993 = VECTOR ( 'NONE', #3625, 1000.000000000000000 ) ;
#9994 = CARTESIAN_POINT ( 'NONE',  ( 16.65937500061452070, 4.541064518000418104, -2.621784821874998173 ) ) ;
#9995 = CARTESIAN_POINT ( 'NONE',  ( 16.16250000000000142, -5.773502691896255534, -1.060575238724906372E-15 ) ) ;
#9996 = CARTESIAN_POINT ( 'NONE',  ( 3.975000001229033852, 2.886751345948126879, 4.999999999999999112 ) ) ;
#9997 = CARTESIAN_POINT ( 'NONE',  ( 24.57187500061451502, -6.054752690667223547, -1.112240025338166033E-15 ) ) ;
#9998 = CARTESIAN_POINT ( 'NONE',  ( 17.78437500061451715, -4.541064518000419881, 2.621784821874995952 ) ) ;
#9999 = CARTESIAN_POINT ( 'NONE',  ( -3.756430356249999214, 13.84062499938548463, 27.83122392262697531 ) ) ;
#10000 = CARTESIAN_POINT ( 'NONE',  ( 29.21249999999999858, -5.773502691896255534, -1.060575238724906372E-15 ) ) ;
#10001 = CARTESIAN_POINT ( 'NONE',  ( 4.724999999999999645, 4.330127018922191873, 2.499999999999999556 ) ) ;
#10002 = CARTESIAN_POINT ( 'NONE',  ( 8.109375000614516438, 2.746126346562643317, 4.756430356249998326 ) ) ;
#10003 = CARTESIAN_POINT ( 'NONE',  ( 19.64062500061451644, -3.027376345333610441, -5.243569643749999898 ) ) ;
#10004 = CARTESIAN_POINT ( 'NONE',  ( 8.775000000000002132, 4.330127018922191873, 2.499999999999999556 ) ) ;
#10005 = CARTESIAN_POINT ( 'NONE',  ( 5.315625000614516260, 3.027376345333613106, -5.243569643749998122 ) ) ;
#10006 = CARTESIAN_POINT ( 'NONE',  ( 20.47500000000000142, 4.330127018922191873, 2.499999999999999556 ) ) ;
#10007 = CARTESIAN_POINT ( 'NONE',  ( -1.071796769724483234, 17.20759618943233704, 25.99999999999999645 ) ) ;
#10008 = CARTESIAN_POINT ( 'NONE',  ( 22.20000000122903216, -2.886751345948125991, -5.000000000000000000 ) ) ;
#10009 = CARTESIAN_POINT ( 'NONE',  ( 4.765820465973550135, 8.794739343793304798, 33.66511406871330081 ) ) ;
#10010 = CARTESIAN_POINT ( 'NONE',  ( 3.337499999999999911, 5.773502691896255534, 3.535250795749688894E-16 ) ) ;
#10011 = VERTEX_POINT ( 'NONE', #32850 ) ;
#10012 = CARTESIAN_POINT ( 'NONE',  ( 17.69062500061451715, -3.027376345333614438, 5.243569643749998122 ) ) ;
#10013 = CARTESIAN_POINT ( 'NONE',  ( 23.31562500061451715, 3.027376345333613106, -5.243569643749998122 ) ) ;
#10014 = CARTESIAN_POINT ( 'NONE',  ( 25.17187500061451644, 3.027376345333613106, -5.243569643749998122 ) ) ;
#10015 = CARTESIAN_POINT ( 'NONE',  ( 6.825000000000001066, 6.123233995736764310E-16, -4.999999999999998224 ) ) ;
#10016 = CARTESIAN_POINT ( 'NONE',  ( 11.50312500061451892, -4.541064518000417216, -2.621784821875001281 ) ) ;
#10017 = CARTESIAN_POINT ( 'NONE',  ( 26.09062500061451573, 6.054752690667223547, 3.707466751127219781E-16 ) ) ;
#10018 = CARTESIAN_POINT ( 'NONE',  ( 13.50937500061451679, 4.541064518000418104, -2.621784821874998173 ) ) ;
#10019 = CARTESIAN_POINT ( 'NONE',  ( 19.43437500061451928, 4.541064518000418104, 2.621784821874999949 ) ) ;
#10020 = CARTESIAN_POINT ( 'NONE',  ( 19.23749999999999716, -2.886751345948197045, 4.999999999999880096 ) ) ;
#10021 = CARTESIAN_POINT ( 'NONE',  ( -4.243569643749999898, 19.80312500061451786, 30.00000000000000000 ) ) ;
#10022 = CARTESIAN_POINT ( 'NONE',  ( 24.15000000122903145, 5.773502691896255534, 3.535250795749688894E-16 ) ) ;
#10023 = CARTESIAN_POINT ( 'NONE',  ( 17.78437500061451715, -4.119189519843968306, 2.378215178124996054 ) ) ;
#10024 = CARTESIAN_POINT ( 'NONE',  ( 13.67812500061451786, -4.541064518000419881, 2.621784821874995952 ) ) ;
#10025 = CARTESIAN_POINT ( 'NONE',  ( 6.909375000614518036, 0.000000000000000000, 5.243569643749999010 ) ) ;
#10026 = CARTESIAN_POINT ( 'NONE',  ( 7.809375000614519280, 0.000000000000000000, 5.243569643749999010 ) ) ;
#10027 = ORIENTED_EDGE ( 'NONE', *, *, #10344, .T. ) ;
#10028 = EDGE_CURVE ( 'NONE', #26188, #12976, #3361, .T. ) ;
#10029 = CARTESIAN_POINT ( 'NONE',  ( 28.32187500061451502, 3.027376345333613106, -5.243569643749998122 ) ) ;
#10030 = CARTESIAN_POINT ( 'NONE',  ( 19.15312500061451573, -4.541064518000417216, -2.621784821875001281 ) ) ;
#10031 = CARTESIAN_POINT ( 'NONE',  ( 3.215625000614518836, 3.027376345333611329, 5.243569643749999010 ) ) ;
#10032 = CARTESIAN_POINT ( 'NONE',  ( 29.50312500061451360, -4.541064518000417216, -2.621784821875001281 ) ) ;
#10033 = CARTESIAN_POINT ( 'NONE',  ( 24.00937500061451502, 0.000000000000000000, 5.243569643749999010 ) ) ;
#10034 = CARTESIAN_POINT ( 'NONE',  ( 20.65312500061451573, 4.541064518000418104, -2.621784821874998173 ) ) ;
#10035 = CARTESIAN_POINT ( 'NONE',  ( -2.828200636599751609E-16, 11.78749999999999964, 25.38119784648299770 ) ) ;
#10036 = VECTOR ( 'NONE', #39102, 1000.000000000000000 ) ;
#10037 = CARTESIAN_POINT ( 'NONE',  ( 24.47812500061451502, -4.541064518000419881, 2.621784821874995952 ) ) ;
#10038 = CARTESIAN_POINT ( 'NONE',  ( 5.550000001229032698, -2.886751345948125991, -5.000000000000000000 ) ) ;
#10039 = EDGE_LOOP ( 'NONE', ( #52253, #19611, #5090, #49545 ) ) ;
#10040 = CARTESIAN_POINT ( 'NONE',  ( 29.09999999999999787, 0.000000000000000000, 4.999999999999998224 ) ) ;
#10041 = CARTESIAN_POINT ( 'NONE',  ( -2.000000000000000000, 16.32499999999999929, -33.46410161513775705 ) ) ;
#10042 = CARTESIAN_POINT ( 'NONE',  ( 22.87500000122903288, 2.886751345948126879, 4.999999999999999112 ) ) ;
#10043 = CARTESIAN_POINT ( 'NONE',  ( 1.878215178124997609, 14.47812499938548214, 33.25316411605952993 ) ) ;
#10044 = CARTESIAN_POINT ( 'NONE',  ( 3.571875000614517237, 3.027376345333613106, -5.243569643749998122 ) ) ;
#10045 = CARTESIAN_POINT ( 'NONE',  ( 28.82812500061451644, 4.541064518000418104, 2.621784821874999949 ) ) ;
#10046 = CARTESIAN_POINT ( 'NONE',  ( 11.87812500061451537, -4.541064518000419881, 2.621784821874995952 ) ) ;
#10047 = CARTESIAN_POINT ( 'NONE',  ( 6.121875000614517504, -6.054752690667223547, -1.112240025338166033E-15 ) ) ;
#10048 = CARTESIAN_POINT ( 'NONE',  ( 24.71250000122903145, 0.000000000000000000, 4.999999999999998224 ) ) ;
#10049 = AXIS2_PLACEMENT_3D ( 'NONE', #57208, #5532, #50243 ) ;
#10050 = CARTESIAN_POINT ( 'NONE',  ( 16.09687500061451715, -3.027376345333610441, -5.243569643749999898 ) ) ;
#10051 = CARTESIAN_POINT ( 'NONE',  ( 3.234375000614516438, 4.541064518000418104, 2.621784821874999949 ) ) ;
#10052 = CARTESIAN_POINT ( 'NONE',  ( 29.17500000000000071, -4.330127018922194537, 2.499999999999995559 ) ) ;
#10053 = CARTESIAN_POINT ( 'NONE',  ( 3.928125000614516527, 6.421520780324663323E-16, -5.243569643749999010 ) ) ;
#10054 = CARTESIAN_POINT ( 'NONE',  ( 14.65312500061451573, -4.541064518000417216, -2.621784821875001281 ) ) ;
#10055 =( BOUNDED_CURVE ( )  B_SPLINE_CURVE ( 3, ( #53842, #26493, #59356, #9136 ),
 .UNSPECIFIED., .F., .F. ) 
 B_SPLINE_CURVE_WITH_KNOTS ( ( 4, 4 ),
 ( 0.3414135753472636314, 0.4010135564025098520 ),
 .UNSPECIFIED. ) 
 CURVE ( )  GEOMETRIC_REPRESENTATION_ITEM ( )  RATIONAL_B_SPLINE_CURVE ( ( 1.000000000000000000, 0.9997040087601481995, 0.9997040087601481995, 1.000000000000000000 ) ) 
 REPRESENTATION_ITEM ( '' )  );
#10056 = ORIENTED_EDGE ( 'NONE', *, *, #56020, .F. ) ;
#10057 = CIRCLE ( 'NONE', #23005, 4.000000000000003553 ) ;
#10058 = CARTESIAN_POINT ( 'NONE',  ( 9.178125000614517859, -4.541064518000419881, 2.621784821874995952 ) ) ;
#10059 = CARTESIAN_POINT ( 'NONE',  ( 8.990625000614516082, 6.054752690667223547, 3.707466751127219781E-16 ) ) ;
#10060 = CARTESIAN_POINT ( 'NONE',  ( 18.27187500061451431, -5.492252693125287522, -1.008910452111647106E-15 ) ) ;
#10061 = CARTESIAN_POINT ( 'NONE',  ( 9.225000000000001421, 4.330127018922191873, 2.499999999999999556 ) ) ;
#10062 = CARTESIAN_POINT ( 'NONE',  ( 3.562500001229033764, 0.000000000000000000, 4.999999999999998224 ) ) ;
#10063 = CARTESIAN_POINT ( 'NONE',  ( 17.69999999999999929, 4.330127018922192761, -2.499999999999997780 ) ) ;
#10064 = EDGE_CURVE ( 'NONE', #71866, #51638, #12496, .T. ) ;
#10065 = CARTESIAN_POINT ( 'NONE',  ( 18.34687500061451715, -3.027376345333610441, -5.243569643749999898 ) ) ;
#10066 = CARTESIAN_POINT ( 'NONE',  ( 12.63750000122903394, -4.330127018922194537, 2.499999999999995559 ) ) ;
#10067 = CARTESIAN_POINT ( 'NONE',  ( 18.82500000000000284, -4.330127018922194537, 2.499999999999995559 ) ) ;
#10068 = CARTESIAN_POINT ( 'NONE',  ( -4.243569643749997233, 16.69062500061451360, -27.54997392385601174 ) ) ;
#10069 = DIRECTION ( 'NONE',  ( 1.000000000000000000, 0.000000000000000000, -0.000000000000000000 ) ) ;
#10070 = CARTESIAN_POINT ( 'NONE',  ( 45.00000000000000000, 0.000000000000000000, 0.000000000000000000 ) ) ;
#10071 = CARTESIAN_POINT ( 'NONE',  ( -5.810221930991193690E-16, 12.35000000122903430, -34.00000000000000000 ) ) ;
#10072 = SURFACE_SIDE_STYLE ('',( #14872 ) ) ;
#10073 = CARTESIAN_POINT ( 'NONE',  ( 17.43750000000000000, -2.886751345948130876, 4.999999999999996447 ) ) ;
#10074 = CARTESIAN_POINT ( 'NONE',  ( 13.58437500061451786, 4.541064518000418104, 2.621784821874999949 ) ) ;
#10075 = CARTESIAN_POINT ( 'NONE',  ( 26.43750000000000000, -2.886751345948129988, 4.999999999999997335 ) ) ;
#10076 = CARTESIAN_POINT ( 'NONE',  ( 10.11562500061451608, -6.054752690667223547, -1.112240025338166033E-15 ) ) ;
#10077 = CARTESIAN_POINT ( 'NONE',  ( 27.42187500061451289, 4.119189519843966529, 2.378215178124999607 ) ) ;
#10078 = CARTESIAN_POINT ( 'NONE',  ( 22.05937500061451573, 4.541064518000418104, -2.621784821874998173 ) ) ;
#10079 = CARTESIAN_POINT ( 'NONE',  ( 12.98437500061451289, 5.492252693125287522, 3.363034840372157021E-16 ) ) ;
#10080 = VECTOR ( 'NONE', #1408, 1000.000000000000000 ) ;
#10081 = CARTESIAN_POINT ( 'NONE',  ( 7.678125000614516082, 4.541064518000418104, 2.621784821874999949 ) ) ;
#10082 = CARTESIAN_POINT ( 'NONE',  ( 13.24687500061451750, -3.027376345333614438, 5.243569643749998122 ) ) ;
#10083 = ORIENTED_EDGE ( 'NONE', *, *, #2879, .F. ) ;
#10084 = CARTESIAN_POINT ( 'NONE',  ( 22.73437500061451644, -4.541064518000419881, 2.621784821874995952 ) ) ;
#10085 = CARTESIAN_POINT ( 'NONE',  ( 0.5511252142286452438, 4.971455555459576736, -26.03572899521184425 ) ) ;
#10086 = CARTESIAN_POINT ( 'NONE',  ( 45.00000000000000000, 0.000000000000000000, 0.000000000000000000 ) ) ;
#10087 = CARTESIAN_POINT ( 'NONE',  ( 5.475000000000000533, 6.123233995736764310E-16, -4.999999999999998224 ) ) ;
#10088 = CARTESIAN_POINT ( 'NONE',  ( 16.53750000122903430, 4.330127018922191873, 2.499999999999999556 ) ) ;
#10089 = DIRECTION ( 'NONE',  ( 1.000000000000000000, 0.000000000000000000, 0.000000000000000000 ) ) ;
#10090 = CARTESIAN_POINT ( 'NONE',  ( 14.55000000122903359, -2.886751345948126435, -5.000000000000000000 ) ) ;
#10091 = ORIENTED_EDGE ( 'NONE', *, *, #58291, .T. ) ;
#10092 = CARTESIAN_POINT ( 'NONE',  ( 12.90000000000000213, 0.000000000000000000, 4.999999999999998224 ) ) ;
#10093 = CARTESIAN_POINT ( 'NONE',  ( 17.02499999999999858, -4.330127018922194537, 2.499999999999995559 ) ) ;
#10094 = CARTESIAN_POINT ( 'NONE',  ( 12.78750000122903430, 6.123233995736764310E-16, -4.999999999999998224 ) ) ;
#10095 = CARTESIAN_POINT ( 'NONE',  ( 10.90312500061451928, 0.000000000000000000, 5.243569643749999010 ) ) ;
#10097 = ORIENTED_EDGE ( 'NONE', *, *, #16399, .F. ) ;
#10096 = VECTOR ( 'NONE', #22341, 1000.000000000000000 ) ;
#10098 = DIRECTION ( 'NONE',  ( -0.000000000000000000, -1.000000000000000000, -0.000000000000000000 ) ) ;
#10099 = CARTESIAN_POINT ( 'NONE',  ( -4.243569643749997233, 18.09687500061452070, -27.54997392385601174 ) ) ;
#10100 = CARTESIAN_POINT ( 'NONE',  ( 3.740625000614516527, -3.027376345333614438, 5.243569643749998122 ) ) ;
#10101 = CARTESIAN_POINT ( 'NONE',  ( -1.878215178124999163, 14.59062499938548463, 26.74683588394047007 ) ) ;
#10102 = CARTESIAN_POINT ( 'NONE',  ( 9.975000000000001421, 6.123233995736764310E-16, -4.999999999999998224 ) ) ;
#10103 = EDGE_LOOP ( 'NONE', ( #48887, #2429, #41244, #1421, #3545 ) ) ;
#10104 = CARTESIAN_POINT ( 'NONE',  ( 23.16562500061451502, -6.054752690667223547, -1.112240025338166033E-15 ) ) ;
#10105 = CARTESIAN_POINT ( 'NONE',  ( 29.39999999999999858, 4.330127018922192761, -2.499999999999997780 ) ) ;
#10106 = CARTESIAN_POINT ( 'NONE',  ( -7.967954043666661671E-16, 19.72812499938548214, 34.33755215474603517 ) ) ;
#10107 = CARTESIAN_POINT ( 'NONE',  ( 21.68437500061451573, 4.541064518000418104, 2.621784821874999949 ) ) ;
#10108 = CARTESIAN_POINT ( 'NONE',  ( 18.89062500061451644, 6.054752690667223547, 3.707466751127219781E-16 ) ) ;
#10109 = CARTESIAN_POINT ( 'NONE',  ( -4.243569643749998122, 14.89062500061459282, -27.54997392385601174 ) ) ;
#10110 = CARTESIAN_POINT ( 'NONE',  ( 6.928125000614516082, -4.541064518000419881, 2.621784821874995952 ) ) ;
#10111 = CARTESIAN_POINT ( 'NONE',  ( 4.303125000614516971, -4.541064518000417216, -2.621784821875001281 ) ) ;
#10112 = CARTESIAN_POINT ( 'NONE',  ( 24.68437500061451573, 5.824947211148865298E-16, -4.756430356249998326 ) ) ;
#10113 = CARTESIAN_POINT ( 'NONE',  ( 20.65312500061451573, 4.541064518000418104, -2.621784821874998173 ) ) ;
#10114 = DIRECTION ( 'NONE',  ( -0.000000000000000000, -1.000000000000000000, -0.000000000000000000 ) ) ;
#10115 = CARTESIAN_POINT ( 'NONE',  ( -1.878215178125001827, 17.44062499938548072, 33.25316411605952283 ) ) ;
#10116 = CARTESIAN_POINT ( 'NONE',  ( 14.29687500061451821, -3.027376345333610441, -5.243569643749999898 ) ) ;
#10117 = CARTESIAN_POINT ( 'NONE',  ( 15.49687500061451750, -3.027376345333614438, 5.243569643749998122 ) ) ;
#10118 = CARTESIAN_POINT ( 'NONE',  ( 23.07187500061451857, 3.027376345333611329, 5.243569643749999010 ) ) ;
#10119 = ORIENTED_EDGE ( 'NONE', *, *, #50679, .T. ) ;
#10120 = CARTESIAN_POINT ( 'NONE',  ( 4.243569643749999898, 12.43437500061451750, 30.00000000000000000 ) ) ;
#10121 = CARTESIAN_POINT ( 'NONE',  ( -3.999999999999999112, 14.67500000122903536, -32.30940107675850470 ) ) ;
#10122 = CARTESIAN_POINT ( 'NONE',  ( 26.84062500061451573, -3.027376345333610441, -5.243569643749999898 ) ) ;
#10123 = CARTESIAN_POINT ( 'NONE',  ( 25.97812500061451502, 6.421520780324663323E-16, -5.243569643749999010 ) ) ;
#10124 = CARTESIAN_POINT ( 'NONE',  ( 1.071796769724497445, 16.37990381179669797, -33.99999999999998579 ) ) ;
#10125 = CARTESIAN_POINT ( 'NONE',  ( 4.898587196589412829E-16, 27.50000000000000000, 34.00000000000000000 ) ) ;
#10126 = CARTESIAN_POINT ( 'NONE',  ( 3.834375000614519635, -4.541064518000419881, 2.621784821874995952 ) ) ;
#10127 = CARTESIAN_POINT ( 'NONE',  ( 13.38750000122903394, 4.330127018922191873, 2.499999999999999556 ) ) ;
#10128 = CARTESIAN_POINT ( 'NONE',  ( 10.38750000122903572, -4.330127018922194537, 2.499999999999995559 ) ) ;
#10129 = CARTESIAN_POINT ( 'NONE',  ( 28.95000000122903572, -2.886751345948125991, -5.000000000000000000 ) ) ;
#10130 = CARTESIAN_POINT ( 'NONE',  ( -4.000000000000000000, 16.26874999877096784, 30.00000000000000000 ) ) ;
#10131 = CARTESIAN_POINT ( 'NONE',  ( 18.95625000122903003, -4.330127018922190985, -2.500000000000001332 ) ) ;
#10132 = CARTESIAN_POINT ( 'NONE',  ( 12.72187500061451537, 3.027376345333611329, 5.243569643749999010 ) ) ;
#10133 = CARTESIAN_POINT ( 'NONE',  ( 4.683223236373093457, -1.751405183929441556, 4.942428804804532838 ) ) ;
#10134 = ORIENTED_EDGE ( 'NONE', *, *, #48422, .F. ) ;
#10135 = CARTESIAN_POINT ( 'NONE',  ( 19.56562500061451715, -6.054752690667223547, -1.112240025338166033E-15 ) ) ;
#10136 = CARTESIAN_POINT ( 'NONE',  ( 14.85937500061451644, 4.541064518000418104, -2.621784821874998173 ) ) ;
#10137 = CARTESIAN_POINT ( 'NONE',  ( 5.878125000614517148, 4.541064518000418104, 2.621784821874999949 ) ) ;
#10138 = CARTESIAN_POINT ( 'NONE',  ( 23.29687500061451644, -3.027376345333610441, -5.243569643749999898 ) ) ;
#10139 = CARTESIAN_POINT ( 'NONE',  ( 4.415625000614518569, 3.027376345333613106, -5.243569643749998122 ) ) ;
#10140 = CARTESIAN_POINT ( 'NONE',  ( 6.675000001229034474, 2.886751345948126879, 4.999999999999998224 ) ) ;
#10141 = CARTESIAN_POINT ( 'NONE',  ( 9.225000001229034297, 2.886751345948129099, -4.999999999999998224 ) ) ;
#10142 = CARTESIAN_POINT ( 'NONE',  ( 22.04062500061451502, 6.054752690667223547, 3.707466751127219781E-16 ) ) ;
#10143 = CARTESIAN_POINT ( 'NONE',  ( 1.999999999999998668, 19.06250000122903288, -33.46410161513775705 ) ) ;
#10144 = CARTESIAN_POINT ( 'NONE',  ( 8.362500001229031810, 4.330127018922192761, -2.499999999999997780 ) ) ;
#10145 = CARTESIAN_POINT ( 'NONE',  ( 20.61562500061451431, 3.027376345333613106, -5.243569643749998122 ) ) ;
#10146 = AXIS2_PLACEMENT_3D ( 'NONE', #52939, #71400, #20774 ) ;
#10147 = CARTESIAN_POINT ( 'NONE',  ( 14.50312500061451537, 0.000000000000000000, 5.243569643749999010 ) ) ;
#10148 = CARTESIAN_POINT ( 'NONE',  ( 26.89687500061451431, -2.746126346562642428, -4.756430356249999214 ) ) ;
#10149 = CARTESIAN_POINT ( 'NONE',  ( 15.03749999999999964, 5.773502691896255534, 3.535250795749688894E-16 ) ) ;
#10150 = CARTESIAN_POINT ( 'NONE',  ( 11.17500000122903536, 2.886751345948126879, 4.999999999999999112 ) ) ;
#10151 = CARTESIAN_POINT ( 'NONE',  ( 7.040625000614517681, -3.027376345333610441, -5.243569643749999898 ) ) ;
#10152 = CARTESIAN_POINT ( 'NONE',  ( 11.01562500061451821, -6.054752690667223547, -1.112240025338166033E-15 ) ) ;
#10153 = EDGE_CURVE ( 'NONE', #22971, #25850, #22764, .T. ) ;
#10154 = CARTESIAN_POINT ( 'NONE',  ( 21.15000000122903145, -2.886751345948129988, 4.999999999999997335 ) ) ;
#10155 = CARTESIAN_POINT ( 'NONE',  ( 2.121784821875001281, 13.70937500061451786, -26.32496088578401938 ) ) ;
#10156 = CARTESIAN_POINT ( 'NONE',  ( 19.20937500061451786, -4.541064518000417216, -2.621784821875001281 ) ) ;
#10157 = CARTESIAN_POINT ( 'NONE',  ( -3.999999999999999112, 14.43124999877096570, 27.69059892324149530 ) ) ;
#10158 = CARTESIAN_POINT ( 'NONE',  ( 5.962500001229033231, -4.330127018922190985, -2.500000000000001332 ) ) ;
#10159 = CARTESIAN_POINT ( 'NONE',  ( 3.496875000614518836, -3.027376345333610441, -5.243569643749999898 ) ) ;
#10160 = CARTESIAN_POINT ( 'NONE',  ( 22.02187500061452141, 3.027376345333613106, -5.243569643749998122 ) ) ;
#10161 = DIRECTION ( 'NONE',  ( -1.000000000000000000, -0.000000000000000000, -0.000000000000000000 ) ) ;
#10162 = CARTESIAN_POINT ( 'NONE',  ( 18.10312500061451502, 0.000000000000000000, 5.243569643749999010 ) ) ;
#10163 = CARTESIAN_POINT ( 'NONE',  ( 11.94375000122903252, 5.773502691896255534, 3.535250795749688894E-16 ) ) ;
#10164 = LINE ( 'NONE', #28248, #17674 ) ;
#10165 = CARTESIAN_POINT ( 'NONE',  ( -1.071796769724483234, 15.40759618943233811, 25.99999999999999645 ) ) ;
#10166 = CARTESIAN_POINT ( 'NONE',  ( 29.44687500061451857, -3.027376345333614438, 5.243569643749998122 ) ) ;
#10167 = CARTESIAN_POINT ( 'NONE',  ( 21.94687500061451146, 4.119189519843966529, -2.378215178124998275 ) ) ;
#10168 = CARTESIAN_POINT ( 'NONE',  ( 15.81562500061451537, 3.027376345333611329, 5.243569643749999010 ) ) ;
#10169 = CARTESIAN_POINT ( 'NONE',  ( 12.90937500061451537, -4.541064518000417216, -2.621784821875001281 ) ) ;
#10170 = VERTEX_POINT ( 'NONE', #46480 ) ;
#10171 = CARTESIAN_POINT ( 'NONE',  ( 22.67812500061451431, -4.541064518000419881, 2.621784821874995952 ) ) ;
#10172 = CARTESIAN_POINT ( 'NONE',  ( -1.071796769724488563, 10.75490381179670152, -26.00000000000000000 ) ) ;
#10173 = CARTESIAN_POINT ( 'NONE',  ( -3.999999999999999112, 11.56250000122903465, -30.00000000000000000 ) ) ;
#10174 = CARTESIAN_POINT ( 'NONE',  ( 13.19999999999999929, 4.330127018922192761, -2.499999999999997780 ) ) ;
#10175 = CARTESIAN_POINT ( 'NONE',  ( 24.56250000122903288, 4.330127018922192761, -2.499999999999997780 ) ) ;
#10176 = CARTESIAN_POINT ( 'NONE',  ( 17.91562500061451502, 3.027376345333613106, -5.243569643749998122 ) ) ;
#10177 = EDGE_LOOP ( 'NONE', ( #58165, #17633, #34372, #40085 ) ) ;
#10178 = CARTESIAN_POINT ( 'NONE',  ( 23.02499999999999858, 6.123233995736764310E-16, -4.999999999999998224 ) ) ;
#10179 = CARTESIAN_POINT ( 'NONE',  ( 24.75937500061451502, 4.541064518000418104, -2.621784821874998173 ) ) ;
#10180 = ORIENTED_EDGE ( 'NONE', *, *, #61111, .F. ) ;
#10181 = CARTESIAN_POINT ( 'NONE',  ( 30.00000000000000000, 0.000000000000000000, 0.000000000000000000 ) ) ;
#10182 = CARTESIAN_POINT ( 'NONE',  ( 9.778125000614517504, 6.421520780324663323E-16, -5.243569643749999010 ) ) ;
#10183 = CARTESIAN_POINT ( 'NONE',  ( 11.02500000000000036, 4.330127018922191873, 2.499999999999999556 ) ) ;
#10184 = CARTESIAN_POINT ( 'NONE',  ( 15.12187500061451573, 5.824947211148865298E-16, -4.756430356249998326 ) ) ;
#10185 = CARTESIAN_POINT ( 'NONE',  ( 16.05000000000000071, 0.000000000000000000, 4.999999999999998224 ) ) ;
#10186 = CARTESIAN_POINT ( 'NONE',  ( 23.69999999999999929, 0.000000000000000000, 4.999999999999998224 ) ) ;
#10187 = CARTESIAN_POINT ( 'NONE',  ( 7.612500001229035362, 0.000000000000000000, 4.999999999999998224 ) ) ;
#10188 = CARTESIAN_POINT ( 'NONE',  ( 3.534375000614518036, 6.421520780324663323E-16, -5.243569643749999010 ) ) ;
#10189 = CARTESIAN_POINT ( 'NONE',  ( 27.64687500061452141, -3.027376345333614438, 5.243569643749998122 ) ) ;
#10190 = VERTEX_POINT ( 'NONE', #23206 ) ;
#10191 = CARTESIAN_POINT ( 'NONE',  ( 26.09062500061451573, 6.054752690667223547, 3.707466751127219781E-16 ) ) ;
#10192 = CARTESIAN_POINT ( 'NONE',  ( 27.42187500061451644, 3.027376345333613106, -5.243569643749998122 ) ) ;
#10193 = CARTESIAN_POINT ( 'NONE',  ( 1.138803498474273873E-14, 16.38124999877096499, 34.00000000000000000 ) ) ;
#10194 = CARTESIAN_POINT ( 'NONE',  ( 14.13750000000000107, 5.773502691896255534, 3.535250795749688894E-16 ) ) ;
#10195 = CARTESIAN_POINT ( 'NONE',  ( 11.76562500061451644, 3.027376345333611329, 5.243569643749999010 ) ) ;
#10196 = CARTESIAN_POINT ( 'NONE',  ( 6.000000000000001776, 4.330127018922192761, -2.499999999999997780 ) ) ;
#10197 = CARTESIAN_POINT ( 'NONE',  ( 3.999999999999998668, 19.36249999999999716, -32.30940107675850470 ) ) ;
#10198 = CARTESIAN_POINT ( 'NONE',  ( 28.67812500061451431, 6.421520780324663323E-16, -5.243569643749999010 ) ) ;
#10199 = CARTESIAN_POINT ( 'NONE',  ( 16.46250000122903501, 4.330127018922192761, -2.499999999999997780 ) ) ;
#10200 = CARTESIAN_POINT ( 'NONE',  ( 16.35937500061451644, 0.000000000000000000, 4.756430356249998326 ) ) ;
#10201 = CARTESIAN_POINT ( 'NONE',  ( 5.128125000614516260, -4.541064518000419881, 2.621784821874995952 ) ) ;
#10202 = CARTESIAN_POINT ( 'NONE',  ( 22.39687500061451075, -3.027376345333610441, -5.243569643749999898 ) ) ;
#10204 = CARTESIAN_POINT ( 'NONE',  ( 2.121784821875001281, 15.05937500061451928, 33.67503911421598417 ) ) ;
#10203 =( BOUNDED_CURVE ( )  B_SPLINE_CURVE ( 2, ( #717, #67947, #12513, #72759, #63114, #56490, #22145 ),
 .UNSPECIFIED., .F., .F. ) 
 B_SPLINE_CURVE_WITH_KNOTS ( ( 3, 2, 2, 3 ),
 ( 0.1833333333333333204, 0.1861111111111111160, 0.1888888888888888562, 0.1916666666666666519 ),
 .UNSPECIFIED. ) 
 CURVE ( )  GEOMETRIC_REPRESENTATION_ITEM ( )  RATIONAL_B_SPLINE_CURVE ( ( 1.000000000000000000, 0.8660254037844387076, 1.000000000000000000, 0.8660254037844387076, 1.000000000000000000, 0.8660254037844400399, 0.9999999999999986677 ) ) 
 REPRESENTATION_ITEM ( '' )  );
#10205 = CARTESIAN_POINT ( 'NONE',  ( 22.20937500061451431, 0.000000000000000000, 5.243569643749999010 ) ) ;
#10206 = CARTESIAN_POINT ( 'NONE',  ( 29.52187500061451431, -6.054752690667223547, -1.112240025338166033E-15 ) ) ;
#10207 = CARTESIAN_POINT ( 'NONE',  ( -4.243569643749999898, 19.40937500061451715, 30.00000000000000000 ) ) ;
#10208 = CARTESIAN_POINT ( 'NONE',  ( 9.590625000614517504, -3.027376345333614438, 5.243569643749998122 ) ) ;
#10209 = CARTESIAN_POINT ( 'NONE',  ( 21.67500000000000071, 6.123233995736764310E-16, -4.999999999999998224 ) ) ;
#10210 = EDGE_CURVE ( 'NONE', #69178, #66787, #61219, .T. ) ;
#10211 = CARTESIAN_POINT ( 'NONE',  ( 7.696875000614516793, 6.054752690667223547, 3.707466751127219781E-16 ) ) ;
#10212 = CARTESIAN_POINT ( 'NONE',  ( 3.852725565712457723, 3.187011840027719423, -3.887821400885792311 ) ) ;
#10213 = EDGE_CURVE ( 'NONE', #29842, #67424, #30314, .T. ) ;
#10214 = CARTESIAN_POINT ( 'NONE',  ( 10.30312500061451431, 4.541064518000418104, -2.621784821874998173 ) ) ;
#10215 = CARTESIAN_POINT ( 'NONE',  ( 15.60937500061451644, -4.541064518000417216, -2.621784821875001281 ) ) ;
#10216 = CARTESIAN_POINT ( 'NONE',  ( 3.472008138778309494, -3.597954294344049675, -3.814426947577870930 ) ) ;
#10217 = CARTESIAN_POINT ( 'NONE',  ( 21.41250000122903074, 4.330127018922192761, -2.499999999999997780 ) ) ;
#10218 = CARTESIAN_POINT ( 'NONE',  ( 8.184375000614515727, 4.541064518000418104, 2.621784821874999949 ) ) ;
#10219 = CARTESIAN_POINT ( 'NONE',  ( 10.30312500061451431, 4.541064518000418104, -2.621784821874998173 ) ) ;
#10220 = CARTESIAN_POINT ( 'NONE',  ( 26.83125000122903003, 4.330127018922191873, 2.499999999999999556 ) ) ;
#10221 = CARTESIAN_POINT ( 'NONE',  ( 18.53437500061451715, 4.541064518000418104, 2.621784821874999949 ) ) ;
#10222 = CARTESIAN_POINT ( 'NONE',  ( 14.13750000000000107, 5.773502691896255534, 3.535250795749688401E-16 ) ) ;
#10223 = CARTESIAN_POINT ( 'NONE',  ( -3.578127771932954726, 3.495591672637166525, 31.80636524853745684 ) ) ;
#10224 = CARTESIAN_POINT ( 'NONE',  ( 2.121784821875001281, 11.00937500061451857, -26.32496088578401938 ) ) ;
#10225 = EDGE_CURVE ( 'NONE', #29715, #8942, #37861, .T. ) ;
#10226 = CARTESIAN_POINT ( 'NONE',  ( 15.37500000122903465, -5.773502691896255534, -1.060575238724906372E-15 ) ) ;
#10227 = CARTESIAN_POINT ( 'NONE',  ( -4.243569643749999898, 14.40312500061451750, -30.00000000000000000 ) ) ;
#10228 = CARTESIAN_POINT ( 'NONE',  ( 15.33750000122903323, -4.330127018922194537, 2.499999999999995559 ) ) ;
#10229 = CARTESIAN_POINT ( 'NONE',  ( 10.04062500061451502, -3.027376345333614438, 5.243569643749998122 ) ) ;
#10230 = ORIENTED_EDGE ( 'NONE', *, *, #44518, .T. ) ;
#10231 = CARTESIAN_POINT ( 'NONE',  ( 13.42499999999999893, -4.330127018922194537, 2.499999999999995559 ) ) ;
#10232 = DIRECTION ( 'NONE',  ( 0.000000000000000000, 0.000000000000000000, 1.000000000000000000 ) ) ;
#10233 = CARTESIAN_POINT ( 'NONE',  ( 22.11562500061451786, 3.027376345333611329, 5.243569643749999010 ) ) ;
#10234 = CARTESIAN_POINT ( 'NONE',  ( 9.946875000614516793, 6.054752690667223547, 3.707466751127219781E-16 ) ) ;
#10235 = ADVANCED_FACE ( 'NONE', ( #18381 ), #52741, .F. ) ;
#10236 = CARTESIAN_POINT ( 'NONE',  ( 4.400918202330496243, -2.373166445152071535, -4.675799785326651303 ) ) ;
#10237 = CARTESIAN_POINT ( 'NONE',  ( 10.12500000122903465, 2.886751345948129099, -4.999999999999998224 ) ) ;
#10238 = CARTESIAN_POINT ( 'NONE',  ( 19.53750000122903430, 6.123233995736764310E-16, -4.999999999999998224 ) ) ;
#10239 = CARTESIAN_POINT ( 'NONE',  ( 15.77812500061451573, 4.541064518000418104, 2.621784821874999949 ) ) ;
#10240 = CARTESIAN_POINT ( 'NONE',  ( 18.14062500061451644, -3.027376345333614438, 5.243569643749998122 ) ) ;
#10241 = CARTESIAN_POINT ( 'NONE',  ( 24.78750000122903074, -4.330127018922194537, 2.499999999999995559 ) ) ;
#10242 = CARTESIAN_POINT ( 'NONE',  ( 28.61250000122903359, 4.330127018922192761, -2.499999999999997780 ) ) ;
#10243 = CARTESIAN_POINT ( 'NONE',  ( 22.83749999999999858, -2.886751345948129988, 4.999999999999997335 ) ) ;
#10244 = CARTESIAN_POINT ( 'NONE',  ( -3.756430356250001434, 14.70312499938548179, 32.16877607737301048 ) ) ;
#10245 = VECTOR ( 'NONE', #43048, 1000.000000000000000 ) ;
#10246 = CARTESIAN_POINT ( 'NONE',  ( 26.29687500061451644, -3.027376345333614438, 5.243569643749998122 ) ) ;
#10247 = CARTESIAN_POINT ( 'NONE',  ( 11.66250000122903430, 0.000000000000000000, 4.999999999999998224 ) ) ;
#10248 = CARTESIAN_POINT ( 'NONE',  ( 4.012500000000001954, -5.773502691896255534, -1.060575238724906372E-15 ) ) ;
#10249 = EDGE_CURVE ( 'NONE', #16314, #4423, #52964, .T. ) ;
#10250 =( BOUNDED_CURVE ( )  B_SPLINE_CURVE ( 2, ( #26628, #9264, #27356, #4822, #59860, #44360, #43986, #31799, #21794 ),
 .UNSPECIFIED., .F., .F. ) 
 B_SPLINE_CURVE_WITH_KNOTS ( ( 3, 2, 2, 2, 3 ),
 ( 0.5972222222222222099, 0.6018518518518518601, 0.6111111111111111605, 0.6203703703703703498, 0.6250000000000000000 ),
 .UNSPECIFIED. ) 
 CURVE ( )  GEOMETRIC_REPRESENTATION_ITEM ( )  RATIONAL_B_SPLINE_CURVE ( ( 0.9330127018922194093, 0.9330127018922194093, 1.000000000000000000, 0.8660254037844387076, 1.000000000000000000, 0.8660254037844387076, 1.000000000000000000, 0.9330127018922194093, 0.9330127018922194093 ) ) 
 REPRESENTATION_ITEM ( '' )  );
#10251 = CARTESIAN_POINT ( 'NONE',  ( 14.24999999999999822, 0.000000000000000000, 4.999999999999998224 ) ) ;
#10252 = CARTESIAN_POINT ( 'NONE',  ( 4.471875000614518925, 3.027376345333613106, -5.243569643749998122 ) ) ;
#10253 = CARTESIAN_POINT ( 'NONE',  ( 27.17812500061451786, -4.541064518000419881, 2.621784821874995952 ) ) ;
#10254 = CARTESIAN_POINT ( 'NONE',  ( 3.756430356250000546, 13.24062499938548321, 27.83122392262697886 ) ) ;
#10255 = CARTESIAN_POINT ( 'NONE',  ( 2.000000000000001332, 19.69999999999999929, -26.53589838486224650 ) ) ;
#10256 = CARTESIAN_POINT ( 'NONE',  ( 10.02187500061451964, 3.027376345333611329, 5.243569643749999010 ) ) ;
#10257 = CARTESIAN_POINT ( 'NONE',  ( 4.134375000614517681, 4.541064518000418104, 2.621784821874999949 ) ) ;
#10258 = CARTESIAN_POINT ( 'NONE',  ( 8.146875000614516082, 6.054752690667223547, 3.707466751127219781E-16 ) ) ;
#10259 = CARTESIAN_POINT ( 'NONE',  ( 28.77187500061451431, 3.027376345333613106, -5.243569643749998122 ) ) ;
#10260 = CARTESIAN_POINT ( 'NONE',  ( -2.121784821874996840, 13.12812500061459353, 33.67503911421598417 ) ) ;
#10261 = CARTESIAN_POINT ( 'NONE',  ( 20.58750000000000213, -2.886751345948129988, 4.999999999999997335 ) ) ;
#10262 = ORIENTED_EDGE ( 'NONE', *, *, #27962, .T. ) ;
#10263 = CARTESIAN_POINT ( 'NONE',  ( 29.28749999999999787, -2.886751345948125991, -5.000000000000000000 ) ) ;
#10264 = CARTESIAN_POINT ( 'NONE',  ( 4.275000000000001243, 4.330127018922191873, 2.499999999999999556 ) ) ;
#10265 = VERTEX_POINT ( 'NONE', #1787 ) ;
#10266 = CARTESIAN_POINT ( 'NONE',  ( 17.46562500061451217, 3.027376345333613106, -5.243569643749998122 ) ) ;
#10267 = CARTESIAN_POINT ( 'NONE',  ( 8.653125000614515727, 0.000000000000000000, 5.243569643749999010 ) ) ;
#10268 = CARTESIAN_POINT ( 'NONE',  ( 22.35937500061451644, 2.746126346562645981, -4.756430356249997438 ) ) ;
#10269 = CARTESIAN_POINT ( 'NONE',  ( 7.959375000614516971, -4.541064518000417216, -2.621784821875001281 ) ) ;
#10270 = CARTESIAN_POINT ( 'NONE',  ( 16.95000000122903216, 5.773502691896255534, 3.535250795749688894E-16 ) ) ;
#10271 = CARTESIAN_POINT ( 'NONE',  ( 5.810221930991193690E-16, 19.81250000000000000, 26.00000000000000000 ) ) ;
#10272 = CARTESIAN_POINT ( 'NONE',  ( 7.659375000614518036, 4.541064518000418104, -2.621784821874998173 ) ) ;
#10273 = CARTESIAN_POINT ( 'NONE',  ( 11.63437500061451857, 6.421520780324663323E-16, -5.243569643749999010 ) ) ;
#10274 = CARTESIAN_POINT ( 'NONE',  ( 24.64687500061451431, -3.027376345333610441, -5.243569643749999898 ) ) ;
#10275 = CARTESIAN_POINT ( 'NONE',  ( 26.77499999999999858, 4.330127018922191873, 2.499999999999999556 ) ) ;
#10276 = ORIENTED_EDGE ( 'NONE', *, *, #60328, .F. ) ;
#10277 = CARTESIAN_POINT ( 'NONE',  ( 12.03749999999999964, -2.886751345948129988, 4.999999999999997335 ) ) ;
#10278 = CIRCLE ( 'NONE', #49214, 5.000000000000000000 ) ;
#10279 = CARTESIAN_POINT ( 'NONE',  ( 18.23437500061451999, -4.541064518000419881, 2.621784821874995952 ) ) ;
#10280 = CARTESIAN_POINT ( 'NONE',  ( 9.009375000614518569, 4.541064518000418104, -2.621784821874998173 ) ) ;
#10281 = CIRCLE ( 'NONE', #68133, 9.000000000000000000 ) ;
#10282 = CARTESIAN_POINT ( 'NONE',  ( 3.756430356250000546, 15.37812499938548427, 27.83122392262697886 ) ) ;
#10283 = CARTESIAN_POINT ( 'NONE',  ( 21.48750000000000071, -2.886751345948129988, 4.999999999999997335 ) ) ;
#10284 = CARTESIAN_POINT ( 'NONE',  ( 4.000000000000000000, 17.48750000000000071, 27.69059892324149530 ) ) ;
#10285 = CARTESIAN_POINT ( 'NONE',  ( 29.92500000000000071, 4.330127018922191873, 2.499999999999999556 ) ) ;
#10286 = CARTESIAN_POINT ( 'NONE',  ( 21.57187500061451502, 2.746126346562645981, -4.756430356249997438 ) ) ;
#10287 = CARTESIAN_POINT ( 'NONE',  ( 13.34062500061451750, -3.027376345333610441, -5.243569643749999898 ) ) ;
#10288 = CARTESIAN_POINT ( 'NONE',  ( 28.32187500061451502, 3.027376345333613106, -5.243569643749998122 ) ) ;
#10289 = DIRECTION ( 'NONE',  ( -0.000000000000000000, -1.000000000000000000, -0.000000000000000000 ) ) ;
#10290 = CARTESIAN_POINT ( 'NONE',  ( 29.52187500061451431, -6.054752690667223547, -1.112240025338166033E-15 ) ) ;
#10291 = CARTESIAN_POINT ( 'NONE',  ( 10.31250000000000355, -5.773502691896255534, -1.060575238724906372E-15 ) ) ;
#10292 = CARTESIAN_POINT ( 'NONE',  ( -3.999999999999997335, 16.55000000122903003, 32.30940107675850470 ) ) ;
#10293 = CARTESIAN_POINT ( 'NONE',  ( 8.137500001229033941, -4.330127018922194537, 2.499999999999995559 ) ) ;
#10294 = CARTESIAN_POINT ( 'NONE',  ( 22.35937500061451644, -4.541064518000417216, -2.621784821875001281 ) ) ;
#10295 = CARTESIAN_POINT ( 'NONE',  ( 14.03437500061451715, 4.541064518000418104, 2.621784821874999949 ) ) ;
#10296 = CARTESIAN_POINT ( 'NONE',  ( -1.487416814333745711E-14, 15.16250000000000142, 34.00000000000000000 ) ) ;
#10297 = ORIENTED_EDGE ( 'NONE', *, *, #46318, .T. ) ;
#10298 = CARTESIAN_POINT ( 'NONE',  ( 16.04062500061451857, -3.027376345333610441, -5.243569643749999898 ) ) ;
#10299 = CARTESIAN_POINT ( 'NONE',  ( 28.72500000122903074, 2.886751345948126879, 4.999999999999999112 ) ) ;
#10300 = CARTESIAN_POINT ( 'NONE',  ( 16.35937500061451644, 0.000000000000000000, 5.243569643749999010 ) ) ;
#10301 = CARTESIAN_POINT ( 'NONE',  ( 16.52812500061451573, 6.421520780324663323E-16, -5.243569643749999010 ) ) ;
#10302 = CARTESIAN_POINT ( 'NONE',  ( 27.53437500061451360, 4.541064518000418104, 2.621784821874999949 ) ) ;
#10303 = CARTESIAN_POINT ( 'NONE',  ( -4.243569643749997233, 12.64062500061451999, 32.45002607614398471 ) ) ;
#10304 = CARTESIAN_POINT ( 'NONE',  ( 16.99687500061451573, -3.027376345333610441, -5.243569643749999898 ) ) ;
#10305 = CARTESIAN_POINT ( 'NONE',  ( 13.46250000122903323, 0.000000000000000000, 4.999999999999998224 ) ) ;
#10306 = CARTESIAN_POINT ( 'NONE',  ( 10.13437500061451679, -4.119189519843968306, 2.378215178124996054 ) ) ;
#10307 = CARTESIAN_POINT ( 'NONE',  ( -3.000416591977282496E-16, 19.29687500061451644, -34.90005215228797653 ) ) ;
#10308 = EDGE_CURVE ( 'NONE', #58357, #21163, #56222, .T. ) ;
#10309 = CARTESIAN_POINT ( 'NONE',  ( 20.93437500061451573, -4.541064518000419881, 2.621784821874995952 ) ) ;
#10310 = CARTESIAN_POINT ( 'NONE',  ( 21.45000000122903216, 5.773502691896255534, 3.535250795749688894E-16 ) ) ;
#10311 = CARTESIAN_POINT ( 'NONE',  ( 17.97187500061451715, 3.027376345333613106, -5.243569643749998122 ) ) ;
#10312 = CARTESIAN_POINT ( 'NONE',  ( 13.52812500061451750, 4.541064518000418104, 2.621784821874999949 ) ) ;
#10313 = CARTESIAN_POINT ( 'NONE',  ( 4.243569643749999010, 13.37187500061451750, 27.54997392385601174 ) ) ;
#10314 = CARTESIAN_POINT ( 'NONE',  ( 16.90312500061451573, -4.541064518000417216, -2.621784821875001281 ) ) ;
#10315 = ORIENTED_EDGE ( 'NONE', *, *, #59108, .T. ) ;
#10316 = VERTEX_POINT ( 'NONE', #12129 ) ;
#10317 = CARTESIAN_POINT ( 'NONE',  ( 20.24999999999999645, -4.330127018922190985, -2.500000000000001332 ) ) ;
#10318 = CARTESIAN_POINT ( 'NONE',  ( -3.999999999999997335, 17.90000000122903501, 32.30940107675850470 ) ) ;
#10319 = CARTESIAN_POINT ( 'NONE',  ( 25.60312500061451502, 4.541064518000418104, -2.621784821874998173 ) ) ;
#10320 = CARTESIAN_POINT ( 'NONE',  ( 5.503125000614516260, 0.000000000000000000, 5.243569643749999010 ) ) ;
#10321 = CARTESIAN_POINT ( 'NONE',  ( 18.41250000122903430, 0.000000000000000000, 4.999999999999998224 ) ) ;
#10322 = CARTESIAN_POINT ( 'NONE',  ( 23.35312500061451857, 4.541064518000418104, -2.621784821874998173 ) ) ;
#10323 = CARTESIAN_POINT ( 'NONE',  ( 22.53750000000000142, -2.886751345948125991, -5.000000000000000000 ) ) ;
#10324 = CARTESIAN_POINT ( 'NONE',  ( 25.90312500061451573, -4.541064518000417216, -2.621784821875001281 ) ) ;
#10325 = CARTESIAN_POINT ( 'NONE',  ( 6.140625000614516438, -3.027376345333610441, -5.243569643749999898 ) ) ;
#10326 = ORIENTED_EDGE ( 'NONE', *, *, #55566, .T. ) ;
#10327 = CARTESIAN_POINT ( 'NONE',  ( 30.00000000000000000, 0.000000000000000000, 4.999999999999998224 ) ) ;
#10328 = CARTESIAN_POINT ( 'NONE',  ( 3.740625000614516527, -3.027376345333614438, 5.243569643749998122 ) ) ;
#10329 = CARTESIAN_POINT ( 'NONE',  ( 12.27187500061451786, 2.746126346562643317, 4.756430356249998326 ) ) ;
#10330 = CARTESIAN_POINT ( 'NONE',  ( 3.999999999999999112, 13.02500000000000213, 30.00000000000000000 ) ) ;
#10331 = CARTESIAN_POINT ( 'NONE',  ( -3.999999999999997335, 14.30000000122903359, -27.69059892324149175 ) ) ;
#10332 = CARTESIAN_POINT ( 'NONE',  ( -2.121784821874999949, 17.98437500061451999, -33.67503911421598417 ) ) ;
#10333 = ADVANCED_FACE ( 'NONE', ( #34656 ), #57185, .T. ) ;
#10334 = VECTOR ( 'NONE', #62725, 1000.000000000000000 ) ;
#10335 = CARTESIAN_POINT ( 'NONE',  ( 10.31250000000000355, -5.773502691896255534, -1.060575238724906372E-15 ) ) ;
#10336 = CARTESIAN_POINT ( 'NONE',  ( 12.19687500061451679, 6.054752690667223547, 3.707466751127219781E-16 ) ) ;
#10337 = CARTESIAN_POINT ( 'NONE',  ( 6.187500001229032875, 4.330127018922191873, 2.499999999999999556 ) ) ;
#10338 = CARTESIAN_POINT ( 'NONE',  ( 12.87187500061451750, -6.054752690667223547, -1.112240025338166033E-15 ) ) ;
#10339 = CARTESIAN_POINT ( 'NONE',  ( 4.959375000614516971, 4.541064518000418104, -2.621784821874998173 ) ) ;
#10340 = CYLINDRICAL_SURFACE ( 'NONE', #3120, 4.999999999999998224 ) ;
#10341 = CARTESIAN_POINT ( 'NONE',  ( 3.390184931900214860, 3.675138926287994767, 3.390184931900133147 ) ) ;
#10342 = CARTESIAN_POINT ( 'NONE',  ( 9.796875000614519990, -3.027376345333610441, -5.243569643749999898 ) ) ;
#10343 = CARTESIAN_POINT ( 'NONE',  ( 21.93750000122903288, 4.330127018922191873, 2.499999999999999556 ) ) ;
#10344 = EDGE_CURVE ( 'NONE', #4424, #33565, #68096, .T. ) ;
#10345 = CARTESIAN_POINT ( 'NONE',  ( 19.71562500061451928, 3.027376345333613106, -5.243569643749998122 ) ) ;
#10346 = CARTESIAN_POINT ( 'NONE',  ( -1.999999999999997113, 12.53750000122903430, -26.53589838486224295 ) ) ;
#10347 = CARTESIAN_POINT ( 'NONE',  ( -3.000416591977282496E-16, 19.24062500061459247, 25.09994784771203058 ) ) ;
#10348 = CARTESIAN_POINT ( 'NONE',  ( 24.49687500061451573, -3.027376345333614438, 5.243569643749998122 ) ) ;
#10349 = DIRECTION ( 'NONE',  ( -1.000000000000000000, -0.000000000000000000, -0.000000000000000000 ) ) ;
#10350 = CARTESIAN_POINT ( 'NONE',  ( 28.72500000122903074, 2.886751345948126879, 4.999999999999999112 ) ) ;
#10351 = CARTESIAN_POINT ( 'NONE',  ( 20.89687500061451786, -4.119189519843965641, -2.378215178125001383 ) ) ;
#10352 = CARTESIAN_POINT ( 'NONE',  ( 24.10312500061451502, -4.541064518000417216, -2.621784821875001281 ) ) ;
#10353 = CARTESIAN_POINT ( 'NONE',  ( 16.97812500061451502, 6.421520780324663323E-16, -5.243569643749999010 ) ) ;
#10354 = CARTESIAN_POINT ( 'NONE',  ( 13.74375000122903323, 5.773502691896255534, 3.535250795749688894E-16 ) ) ;
#10355 = CARTESIAN_POINT ( 'NONE',  ( 13.65937500061451715, 0.000000000000000000, 5.243569643749999010 ) ) ;
#10356 = CARTESIAN_POINT ( 'NONE',  ( 26.10000000122903785, -2.886751345948146863, 4.999999999999968026 ) ) ;
#10357 = CARTESIAN_POINT ( 'NONE',  ( 27.93750000122903288, -4.330127018922194537, 2.499999999999995559 ) ) ;
#10358 = CARTESIAN_POINT ( 'NONE',  ( 3.009375000614516793, -4.541064518000417216, -2.621784821875001281 ) ) ;
#10359 = CARTESIAN_POINT ( 'NONE',  ( 15.04687500061451644, -3.027376345333614438, 5.243569643749998122 ) ) ;
#10360 = CARTESIAN_POINT ( 'NONE',  ( 5.000000000000000000, 39.99999999999999289, 30.00000000000000000 ) ) ;
#10361 = CARTESIAN_POINT ( 'NONE',  ( 3.412500001229032964, 4.330127018922192761, -2.499999999999997780 ) ) ;
#10362 = CARTESIAN_POINT ( 'NONE',  ( 23.93437500061451573, 4.541064518000418104, 2.621784821874999949 ) ) ;
#10363 = CARTESIAN_POINT ( 'NONE',  ( 16.95937500061451786, -4.541064518000417216, -2.621784821875001281 ) ) ;
#10364 = CARTESIAN_POINT ( 'NONE',  ( 1.878215178125000495, 15.07812499938548179, 26.74683588394047007 ) ) ;
#10365 = CARTESIAN_POINT ( 'NONE',  ( 28.31250000000000000, -5.773502691896255534, -1.060575238724906372E-15 ) ) ;
#10366 = ADVANCED_FACE ( 'NONE', ( #47563 ), #64548, .T. ) ;
#10367 = CARTESIAN_POINT ( 'NONE',  ( 3.712500001229034563, -4.330127018922190985, -2.500000000000001332 ) ) ;
#10368 = CARTESIAN_POINT ( 'NONE',  ( 4.612500000000002487, 2.886751345948129099, -4.999999999999998224 ) ) ;
#10369 = CARTESIAN_POINT ( 'NONE',  ( 28.69687500061451502, -2.746126346562642428, -4.756430356249999214 ) ) ;
#10370 = CARTESIAN_POINT ( 'NONE',  ( 19.75312500061451360, 4.541064518000418104, -2.621784821874998173 ) ) ;
#10371 = CARTESIAN_POINT ( 'NONE',  ( 9.487500000000000711, -2.886751345948125991, -5.000000000000000000 ) ) ;
#10372 = CARTESIAN_POINT ( 'NONE',  ( 5.203125000614518214, -4.541064518000417216, -2.621784821875001281 ) ) ;
#10373 = CARTESIAN_POINT ( 'NONE',  ( 19.38749999999999929, -2.886751345948125991, -5.000000000000000000 ) ) ;
#10374 = DIRECTION ( 'NONE',  ( 0.000000000000000000, 0.000000000000000000, 1.000000000000000000 ) ) ;
#10375 = CARTESIAN_POINT ( 'NONE',  ( 20.28750000122903074, -4.330127018922194537, 2.499999999999995559 ) ) ;
#10376 = CARTESIAN_POINT ( 'NONE',  ( -1.999999999999997113, 10.17500000000000249, -26.53589838486224295 ) ) ;
#10377 = CARTESIAN_POINT ( 'NONE',  ( 3.075000000000001510, -4.330127018922194537, 2.499999999999995559 ) ) ;
#10378 = EDGE_LOOP ( 'NONE', ( #72738, #63812, #49845, #54740 ) ) ;
#10379 = CARTESIAN_POINT ( 'NONE',  ( 16.41562500061451857, -6.054752690667223547, -1.112240025338166033E-15 ) ) ;
#10380 = CARTESIAN_POINT ( 'NONE',  ( 24.96562500061451573, -6.054752690667223547, -1.112240025338166033E-15 ) ) ;
#10381 = CARTESIAN_POINT ( 'NONE',  ( 21.90937500061451715, -4.541064518000417216, -2.621784821875001281 ) ) ;
#10382 = CARTESIAN_POINT ( 'NONE',  ( 7.612500000000000711, -5.773502691896255534, -1.060575238724906372E-15 ) ) ;
#10383 = CARTESIAN_POINT ( 'NONE',  ( 10.22812500061451679, 6.421520780324663323E-16, -5.243569643749999010 ) ) ;
#10384 = CARTESIAN_POINT ( 'NONE',  ( 27.77812500061451573, 6.421520780324663323E-16, -5.243569643749999010 ) ) ;
#10385 = CARTESIAN_POINT ( 'NONE',  ( 14.63437500061451679, -4.541064518000419881, 2.621784821874995952 ) ) ;
#10386 = CARTESIAN_POINT ( 'NONE',  ( 18.53437500061451715, 4.541064518000418104, 2.621784821874999949 ) ) ;
#10387 = CARTESIAN_POINT ( 'NONE',  ( -5.810221930991193690E-16, 11.90000000122903501, -34.00000000000000000 ) ) ;
#10388 = CARTESIAN_POINT ( 'NONE',  ( 4.243569643749999010, 10.22187500061451892, 27.54997392385601174 ) ) ;
#10389 = CARTESIAN_POINT ( 'NONE',  ( 21.00000000122903288, 5.773502691896255534, 3.535250795749688894E-16 ) ) ;
#10390 = CARTESIAN_POINT ( 'NONE',  ( 16.99687500061451573, -2.746126346562641984, -4.756430356249999214 ) ) ;
#10391 = CARTESIAN_POINT ( 'NONE',  ( 10.90312500061451928, 0.000000000000000000, 5.243569643749999010 ) ) ;
#10392 = CARTESIAN_POINT ( 'NONE',  ( 9.009375000614518569, 4.541064518000418104, -2.621784821874998173 ) ) ;
#10393 = CARTESIAN_POINT ( 'NONE',  ( 7.621875000614519280, 3.027376345333613106, -5.243569643749998122 ) ) ;
#10394 = ORIENTED_EDGE ( 'NONE', *, *, #18647, .F. ) ;
#10395 = CARTESIAN_POINT ( 'NONE',  ( 28.50937500061451502, 0.000000000000000000, 5.243569643749999010 ) ) ;
#10396 = CARTESIAN_POINT ( 'NONE',  ( 18.55312500061451431, 0.000000000000000000, 5.243569643749999010 ) ) ;
#10397 = CARTESIAN_POINT ( 'NONE',  ( 28.57500000122903572, 2.886751345948129099, -4.999999999999998224 ) ) ;
#10398 = CARTESIAN_POINT ( 'NONE',  ( 3.796875000614517326, -3.027376345333614438, 5.243569643749998122 ) ) ;
#10399 = CARTESIAN_POINT ( 'NONE',  ( 24.57187500061451502, -6.054752690667223547, -1.112240025338166033E-15 ) ) ;
#10400 = CARTESIAN_POINT ( 'NONE',  ( 18.70312500061451644, -4.541064518000417216, -2.621784821875001281 ) ) ;
#10401 = CARTESIAN_POINT ( 'NONE',  ( 4.243569643749999898, 19.14687500061451431, 32.45002607614398471 ) ) ;
#10402 = CARTESIAN_POINT ( 'NONE',  ( 23.57812500061451289, -4.541064518000419881, 2.621784821874995952 ) ) ;
#10403 = CARTESIAN_POINT ( 'NONE',  ( 3.900000001229034563, 5.773502691896255534, 3.535250795749688894E-16 ) ) ;
#10404 = ORIENTED_EDGE ( 'NONE', *, *, #2674, .T. ) ;
#10405 = CARTESIAN_POINT ( 'NONE',  ( 29.96250000000000213, 2.886751345948126879, 4.999999999999999112 ) ) ;
#10406 = CARTESIAN_POINT ( 'NONE',  ( 8.484601909799253346E-16, 15.61250000000000249, -25.38119784648299770 ) ) ;
#10407 = CARTESIAN_POINT ( 'NONE',  ( 3.756430356250000546, 17.29062499938548214, 27.83122392262697886 ) ) ;
#10408 = CARTESIAN_POINT ( 'NONE',  ( 5.409375000614516260, 4.541064518000418104, -2.621784821874998173 ) ) ;
#10409 = CARTESIAN_POINT ( 'NONE',  ( 11.80312500061451608, 0.000000000000000000, 5.243569643749999010 ) ) ;
#10410 = CARTESIAN_POINT ( 'NONE',  ( 5.709375000614517859, -4.541064518000417216, -2.621784821875001281 ) ) ;
#10411 = CARTESIAN_POINT ( 'NONE',  ( 24.90000000122903145, -2.886751345948125991, -5.000000000000000000 ) ) ;
#10412 = CARTESIAN_POINT ( 'NONE',  ( 14.89687500061451786, 6.054752690667223547, 3.707466751127219781E-16 ) ) ;
#10413 = CARTESIAN_POINT ( 'NONE',  ( 3.759375000614517681, 0.000000000000000000, 5.243569643749999010 ) ) ;
#10414 = CARTESIAN_POINT ( 'NONE',  ( 2.000000000000001332, 17.44999999999999929, -26.53589838486224650 ) ) ;
#10415 =( BOUNDED_CURVE ( )  B_SPLINE_CURVE ( 2, ( #56332, #191, #50432, #40073, #58114, #7165, #40795, #13787, #47414 ),
 .UNSPECIFIED., .F., .F. ) 
 B_SPLINE_CURVE_WITH_KNOTS ( ( 3, 2, 2, 2, 3 ),
 ( 0.6195652173913043237, 0.6231884057971014412, 0.6304347826086956763, 0.6376811594202898004, 0.6413043478260869179 ),
 .UNSPECIFIED. ) 
 CURVE ( )  GEOMETRIC_REPRESENTATION_ITEM ( )  RATIONAL_B_SPLINE_CURVE ( ( 0.9330127018922194093, 0.9330127018922194093, 1.000000000000000000, 0.8660254037844387076, 1.000000000000000000, 0.8660254037844387076, 1.000000000000000000, 0.9330127018922194093, 0.9330127018922194093 ) ) 
 REPRESENTATION_ITEM ( '' )  );
#10416 = CARTESIAN_POINT ( 'NONE',  ( 26.85937500061451644, -4.541064518000417216, -2.621784821875001281 ) ) ;
#10417 = CARTESIAN_POINT ( 'NONE',  ( 14.36249999999999893, -5.773502691896255534, -1.060575238724906372E-15 ) ) ;
#10418 = CARTESIAN_POINT ( 'NONE',  ( 13.30312500061451786, -4.541064518000417216, -2.621784821875001281 ) ) ;
#10419 = ORIENTED_EDGE ( 'NONE', *, *, #10486, .T. ) ;
#10420 = CARTESIAN_POINT ( 'NONE',  ( 10.86562500061451431, 3.027376345333611329, 5.243569643749999010 ) ) ;
#10421 = CARTESIAN_POINT ( 'NONE',  ( 8.015625000614518214, 3.027376345333613106, -5.243569643749998122 ) ) ;
#10422 = CARTESIAN_POINT ( 'NONE',  ( 17.93437500061451928, 5.824947211148865298E-16, -4.756430356249998326 ) ) ;
#10423 = CARTESIAN_POINT ( 'NONE',  ( 9.674999999999998934, 4.330127018922191873, 2.499999999999999556 ) ) ;
#10424 = CARTESIAN_POINT ( 'NONE',  ( 4.462500001229035007, 0.000000000000000000, 4.999999999999998224 ) ) ;
#10425 = VECTOR ( 'NONE', #31873, 1000.000000000000000 ) ;
#10426 = CARTESIAN_POINT ( 'NONE',  ( 17.36249999999999716, 2.886751345948126879, 4.999999999999999112 ) ) ;
#10427 = CARTESIAN_POINT ( 'NONE',  ( 18.15937500061451715, 0.000000000000000000, 5.243569643749999010 ) ) ;
#10428 = CARTESIAN_POINT ( 'NONE',  ( 13.12500000122903288, -5.773502691896255534, -1.060575238724906372E-15 ) ) ;
#10429 = CARTESIAN_POINT ( 'NONE',  ( 21.03750000000000142, -2.886751345948129988, 4.999999999999997335 ) ) ;
#10430 = CARTESIAN_POINT ( 'NONE',  ( -4.243569643749999898, 17.10312500061451502, -30.00000000000000000 ) ) ;
#10431 = CARTESIAN_POINT ( 'NONE',  ( 21.93750000000000000, -2.886751345948130876, 4.999999999999996447 ) ) ;
#10432 = CARTESIAN_POINT ( 'NONE',  ( 24.09375000122903288, 5.773502691896255534, 3.535250795749688401E-16 ) ) ;
#10433 = CARTESIAN_POINT ( 'NONE',  ( 29.50312500061451360, -4.541064518000417216, -2.621784821875001281 ) ) ;
#10434 = CARTESIAN_POINT ( 'NONE',  ( 1.071796769724490783, 19.68259618943233491, 34.00000000000000000 ) ) ;
#10435 = CARTESIAN_POINT ( 'NONE',  ( 24.29999999999999716, -4.330127018922190985, -2.500000000000001332 ) ) ;
#10436 = CARTESIAN_POINT ( 'NONE',  ( 13.24687500061451750, -3.027376345333614438, 5.243569643749998122 ) ) ;
#10437 = CARTESIAN_POINT ( 'NONE',  ( 26.36249999999999716, 2.886751345948126879, 4.999999999999999112 ) ) ;
#10438 = CARTESIAN_POINT ( 'NONE',  ( 9.290625000614515017, -3.027376345333610441, -5.243569643749999898 ) ) ;
#10439 = CARTESIAN_POINT ( 'NONE',  ( 28.13437500061451502, -2.746126346562642428, -4.756430356249999214 ) ) ;
#10440 = CARTESIAN_POINT ( 'NONE',  ( 21.00937500061451857, -4.541064518000417216, -2.621784821875001281 ) ) ;
#10441 = CARTESIAN_POINT ( 'NONE',  ( 14.59687500061451537, -4.119189519843965641, -2.378215178125001383 ) ) ;
#10442 = CARTESIAN_POINT ( 'NONE',  ( 7.453125000614516438, -4.541064518000417216, -2.621784821875001281 ) ) ;
#10443 = CARTESIAN_POINT ( 'NONE',  ( 10.99687500061451750, -3.027376345333614438, 5.243569643749998122 ) ) ;
#10444 = ORIENTED_EDGE ( 'NONE', *, *, #15050, .T. ) ;
#10445 = CARTESIAN_POINT ( 'NONE',  ( 21.00937500061451857, -4.541064518000417216, -2.621784821875001281 ) ) ;
#10446 = CARTESIAN_POINT ( 'NONE',  ( 28.98750000000000071, 5.773502691896255534, 3.535250795749688401E-16 ) ) ;
#10447 = FACE_OUTER_BOUND ( 'NONE', #63927, .T. ) ;
#10448 =( BOUNDED_CURVE ( )  B_SPLINE_CURVE ( 2, ( #29610, #2268, #69507, #52146, #68782, #8167, #40337, #24783, #6721 ),
 .UNSPECIFIED., .F., .T. ) 
 B_SPLINE_CURVE_WITH_KNOTS ( ( 3, 2, 2, 2, 3 ),
 ( 0.9239130434782608647, 0.9275362318840579823, 0.9347826086956522174, 0.9420289855072463414, 0.9456521739130434590 ),
 .UNSPECIFIED. ) 
 CURVE ( )  GEOMETRIC_REPRESENTATION_ITEM ( )  RATIONAL_B_SPLINE_CURVE ( ( 0.9330127018922194093, 0.9330127018922194093, 1.000000000000000000, 0.8660254037844387076, 1.000000000000000000, 0.8660254037844387076, 1.000000000000000000, 0.9330127018922194093, 0.9330127018922194093 ) ) 
 REPRESENTATION_ITEM ( '' )  );
#10449 = CARTESIAN_POINT ( 'NONE',  ( 4.875000000000000888, -4.330127018922194537, 2.499999999999995559 ) ) ;
#10450 = CARTESIAN_POINT ( 'NONE',  ( 14.70000000122903394, 5.773502691896255534, 3.535250795749688894E-16 ) ) ;
#10451 = CARTESIAN_POINT ( 'NONE',  ( 17.98125000122903572, -4.330127018922194537, 2.499999999999995559 ) ) ;
#10452 = CARTESIAN_POINT ( 'NONE',  ( 18.71249999999999503, 2.886751345948182834, 4.999999999999902300 ) ) ;
#10453 = VERTEX_POINT ( 'NONE', #31302 ) ;
#10454 = CARTESIAN_POINT ( 'NONE',  ( 12.18750000000000000, -2.886751345948125991, -5.000000000000000000 ) ) ;
#10455 = CARTESIAN_POINT ( 'NONE',  ( 15.48749999999999893, 5.773502691896255534, 3.535250795749688894E-16 ) ) ;
#10456 = CARTESIAN_POINT ( 'NONE',  ( 12.63750000122903394, -4.330127018922194537, 2.499999999999995559 ) ) ;
#10457 = CARTESIAN_POINT ( 'NONE',  ( 11.31562500061451892, 3.027376345333611329, 5.243569643749999010 ) ) ;
#10458 = VERTEX_POINT ( 'NONE', #53101 ) ;
#10459 = CARTESIAN_POINT ( 'NONE',  ( 8.250000000000000000, 4.330127018922192761, -2.499999999999997780 ) ) ;
#10460 = CARTESIAN_POINT ( 'NONE',  ( -3.000416591977282496E-16, 13.44687500061451857, -34.90005215228797653 ) ) ;
#10461 = CARTESIAN_POINT ( 'NONE',  ( 29.62500000122903288, 2.886751345948126879, 4.999999999999999112 ) ) ;
#10462 = CARTESIAN_POINT ( 'NONE',  ( 3.756430356250000102, 15.79062499938548392, 30.00000000000000000 ) ) ;
#10463 = CARTESIAN_POINT ( 'NONE',  ( 9.262499999999999289, 2.886751345948126879, 4.999999999999999112 ) ) ;
#10464 = CARTESIAN_POINT ( 'NONE',  ( 3.965171583692859603, 3.045884815923804556, 3.965171583692790325 ) ) ;
#10465 = ORIENTED_EDGE ( 'NONE', *, *, #10153, .T. ) ;
#10466 = CARTESIAN_POINT ( 'NONE',  ( 24.14062500061451289, -3.027376345333610441, -5.243569643749999898 ) ) ;
#10467 = DIRECTION ( 'NONE',  ( -1.000000000000000000, -0.000000000000000000, -0.000000000000000000 ) ) ;
#10468 = CARTESIAN_POINT ( 'NONE',  ( 3.756430356249998770, 20.25312499938547717, 32.16877607737302469 ) ) ;
#10469 = CARTESIAN_POINT ( 'NONE',  ( 22.02187500061452141, 3.027376345333613106, -5.243569643749998122 ) ) ;
#10470 = CARTESIAN_POINT ( 'NONE',  ( 16.94062500061451715, -3.027376345333610441, -5.243569643749999898 ) ) ;
#10471 = EDGE_CURVE ( 'NONE', #2226, #12747, #2489, .T. ) ;
#10472 = CARTESIAN_POINT ( 'NONE',  ( 2.121784821874999061, 10.65312500061459389, -33.67503911421598417 ) ) ;
#10473 = CARTESIAN_POINT ( 'NONE',  ( 6.028125000614517504, -4.541064518000419881, 2.621784821874995952 ) ) ;
#10474 = CARTESIAN_POINT ( 'NONE',  ( 29.62500000122903288, 2.886751345948126879, 4.999999999999999112 ) ) ;
#10475 = CARTESIAN_POINT ( 'NONE',  ( 25.47187500061451715, -5.492252693125287522, -1.008910452111647106E-15 ) ) ;
#10476 = CARTESIAN_POINT ( 'NONE',  ( 18.81562500061451715, 3.027376345333612662, -5.243569643749998122 ) ) ;
#10477 = CARTESIAN_POINT ( 'NONE',  ( 8.034375000614518925, 5.824947211148865298E-16, -4.756430356249998326 ) ) ;
#10478 = CARTESIAN_POINT ( 'NONE',  ( 3.756430356250000546, 18.52812499938548285, 27.83122392262697886 ) ) ;
#10479 = CARTESIAN_POINT ( 'NONE',  ( 14.44687500061451679, 6.054752690667223547, 3.707466751127219781E-16 ) ) ;
#10480 = CARTESIAN_POINT ( 'NONE',  ( 14.03437500061451715, 4.541064518000418104, 2.621784821874999949 ) ) ;
#10481 = CARTESIAN_POINT ( 'NONE',  ( 21.87187500061451573, -6.054752690667223547, -1.112240025338166033E-15 ) ) ;
#10482 = ORIENTED_EDGE ( 'NONE', *, *, #458, .T. ) ;
#10483 = CARTESIAN_POINT ( 'NONE',  ( 4.243569643749999010, 12.47187500061451715, 27.54997392385601174 ) ) ;
#10484 = CARTESIAN_POINT ( 'NONE',  ( 3.890625000614517326, -3.027376345333610441, -5.243569643749999898 ) ) ;
#10485 = CARTESIAN_POINT ( 'NONE',  ( 26.42812500061451431, 6.421520780324663323E-16, -5.243569643749999010 ) ) ;
#10486 = EDGE_CURVE ( 'NONE', #47796, #55334, #10055, .T. ) ;
#10487 =( BOUNDED_CURVE ( )  B_SPLINE_CURVE ( 2, ( #4058, #60180, #26216, #70551, #3327, #64637, #14023 ),
 .UNSPECIFIED., .F., .F. ) 
 B_SPLINE_CURVE_WITH_KNOTS ( ( 3, 2, 2, 3 ),
 ( 0.6100000000000002087, 0.6133333333333333970, 0.6166666666666668073, 0.6199999999999999956 ),
 .UNSPECIFIED. ) 
 CURVE ( )  GEOMETRIC_REPRESENTATION_ITEM ( )  RATIONAL_B_SPLINE_CURVE ( ( 0.9999999999999911182, 0.8660254037844475894, 1.000000000000000000, 0.8660254037844387076, 1.000000000000000000, 0.8660254037844387076, 1.000000000000000000 ) ) 
 REPRESENTATION_ITEM ( '' )  );
#10488 = CARTESIAN_POINT ( 'NONE',  ( 27.14062500061451644, -3.027376345333614438, 5.243569643749998122 ) ) ;
#10489 = DIRECTION ( 'NONE',  ( 0.000000000000000000, 6.195440985631455317E-17, 1.000000000000000000 ) ) ;
#10490 = CARTESIAN_POINT ( 'NONE',  ( 8.484601909799253346E-16, 18.76250000000000284, 34.61880215351700230 ) ) ;
#10491 = CARTESIAN_POINT ( 'NONE',  ( 4.846875000614519813, -3.027376345333610441, -5.243569643749999898 ) ) ;
#10492 = CARTESIAN_POINT ( 'NONE',  ( 12.86250000122903359, 4.330127018922192761, -2.499999999999997780 ) ) ;
#10493 = CARTESIAN_POINT ( 'NONE',  ( 8.212500001229035007, -4.330127018922190985, -2.500000000000001332 ) ) ;
#10494 = CARTESIAN_POINT ( 'NONE',  ( 28.91250000122903074, -4.330127018922190985, -2.500000000000001332 ) ) ;
#10495 = CARTESIAN_POINT ( 'NONE',  ( -8.484601909799255319E-16, 15.48124999877096641, 34.61880215351700940 ) ) ;
#10496 = CARTESIAN_POINT ( 'NONE',  ( 19.59375000122903288, 5.773502691896255534, 3.535250795749688894E-16 ) ) ;
#10497 = CARTESIAN_POINT ( 'NONE',  ( 11.59687500061451892, -3.027376345333610441, -5.243569643749999898 ) ) ;
#10498 = CARTESIAN_POINT ( 'NONE',  ( -1.999999999999999112, 17.54374999877096641, 26.53589838486224650 ) ) ;
#10499 = ORIENTED_EDGE ( 'NONE', *, *, #68490, .T. ) ;
#10500 = CARTESIAN_POINT ( 'NONE',  ( 19.94062500061451715, -3.027376345333614438, 5.243569643749998122 ) ) ;
#10501 = CARTESIAN_POINT ( 'NONE',  ( 12.34687500061452070, -3.027376345333614438, 5.243569643749998122 ) ) ;
#10502 = CARTESIAN_POINT ( 'NONE',  ( 5.953125000614519102, 0.000000000000000000, 5.243569643749999010 ) ) ;
#10503 = CARTESIAN_POINT ( 'NONE',  ( 21.79687500061451644, -3.027376345333614438, 5.243569643749998122 ) ) ;
#10504 = CARTESIAN_POINT ( 'NONE',  ( 5.915625000614515905, 3.027376345333611329, 5.243569643749999010 ) ) ;
#10505 = DIRECTION ( 'NONE',  ( 0.000000000000000000, 0.000000000000000000, -1.000000000000000000 ) ) ;
#10506 = CARTESIAN_POINT ( 'NONE',  ( 6.187500001229032875, 4.330127018922191873, 2.499999999999999556 ) ) ;
#10507 = CARTESIAN_POINT ( 'NONE',  ( 21.81562500061451004, -6.054752690667223547, -1.112240025338166033E-15 ) ) ;
#10508 = CARTESIAN_POINT ( 'NONE',  ( -2.828200636599751609E-16, 18.65000000122903501, -34.61880215351700230 ) ) ;
#10509 = CARTESIAN_POINT ( 'NONE',  ( 9.037500001229034297, -4.330127018922194537, 2.499999999999995559 ) ) ;
#10510 =( BOUNDED_CURVE ( )  B_SPLINE_CURVE ( 2, ( #41321, #36131, #19486, #24673, #29861, #47220, #41674 ),
 .UNSPECIFIED., .F., .F. ) 
 B_SPLINE_CURVE_WITH_KNOTS ( ( 3, 2, 2, 3 ),
 ( 0.02999999999999993991, 0.03333333333333331899, 0.03666666666666669461, 0.04000000000000007022 ),
 .UNSPECIFIED. ) 
 CURVE ( )  GEOMETRIC_REPRESENTATION_ITEM ( )  RATIONAL_B_SPLINE_CURVE ( ( 1.000000000000002442, 0.8660254037844364872, 1.000000000000000000, 0.8660254037844387076, 1.000000000000000000, 0.8660254037844359321, 1.000000000000002887 ) ) 
 REPRESENTATION_ITEM ( '' )  );
#10511 = CARTESIAN_POINT ( 'NONE',  ( 16.64062500061451289, 6.054752690667223547, 3.707466751127219781E-16 ) ) ;
#10512 = CARTESIAN_POINT ( 'NONE',  ( 16.00312500061451715, -4.541064518000417216, -2.621784821875001281 ) ) ;
#10513 = CARTESIAN_POINT ( 'NONE',  ( 26.59687500061451360, 5.492252693125287522, 3.363034840372157021E-16 ) ) ;
#10514 = CARTESIAN_POINT ( 'NONE',  ( 15.90000000000000036, 4.330127018922192761, -2.499999999999997780 ) ) ;
#10515 = CARTESIAN_POINT ( 'NONE',  ( 10.91250000122903252, -4.330127018922190985, -2.500000000000001332 ) ) ;
#10516 = CARTESIAN_POINT ( 'NONE',  ( 8.615625000614517859, 3.027376345333611329, 5.243569643749999010 ) ) ;
#10517 = CARTESIAN_POINT ( 'NONE',  ( 11.35312500061451679, 0.000000000000000000, 5.243569643749999010 ) ) ;
#10518 = CARTESIAN_POINT ( 'NONE',  ( 20.96250000122903145, 4.330127018922192761, -2.499999999999997780 ) ) ;
#10519 = CARTESIAN_POINT ( 'NONE',  ( 9.001249775931846008E-16, 12.77187500061451786, -25.09994784771203058 ) ) ;
#10520 = FACE_OUTER_BOUND ( 'NONE', #48532, .T. ) ;
#10521 = CARTESIAN_POINT ( 'NONE',  ( 4.575000001229033941, -5.773502691896255534, -1.060575238724906372E-15 ) ) ;
#10522 = CARTESIAN_POINT ( 'NONE',  ( 3.909375000614518481, -4.541064518000417216, -2.621784821875001281 ) ) ;
#10523 = CARTESIAN_POINT ( 'NONE',  ( 20.33437500061451786, 4.541064518000418104, 2.621784821874999949 ) ) ;
#10524 = CARTESIAN_POINT ( 'NONE',  ( 5.025000000000002132, 6.123233995736764310E-16, -4.999999999999998224 ) ) ;
#10525 = CARTESIAN_POINT ( 'NONE',  ( 16.49062500061451786, -3.027376345333610441, -5.243569643749999898 ) ) ;
#10526 = CARTESIAN_POINT ( 'NONE',  ( 11.23125000122903216, -4.330127018922194537, 2.499999999999995559 ) ) ;
#10527 = CARTESIAN_POINT ( 'NONE',  ( -2.000000000000000000, 14.63750000122903394, 26.53589838486224650 ) ) ;
#10528 = CARTESIAN_POINT ( 'NONE',  ( 1.626862140677534273E-15, 15.61250000000000071, 34.00000000000000000 ) ) ;
#10529 = CARTESIAN_POINT ( 'NONE',  ( 29.63437500061451502, 6.421520780324663323E-16, -5.243569643749999010 ) ) ;
#10530 = CARTESIAN_POINT ( 'NONE',  ( 19.84687500061451360, 0.000000000000000000, 4.756430356249998326 ) ) ;
#10531 = CARTESIAN_POINT ( 'NONE',  ( 15.29062500061451679, 6.054752690667223547, 3.707466751127219781E-16 ) ) ;
#10532 = CARTESIAN_POINT ( 'NONE',  ( 12.00937500061451857, -4.541064518000417216, -2.621784821875001281 ) ) ;
#10533 = ORIENTED_EDGE ( 'NONE', *, *, #14215, .F. ) ;
#10534 = CARTESIAN_POINT ( 'NONE',  ( 22.34062500061451573, -3.027376345333610441, -5.243569643749999898 ) ) ;
#10535 = FACE_OUTER_BOUND ( 'NONE', #69101, .T. ) ;
#10536 = CARTESIAN_POINT ( 'NONE',  ( -3.999999999999997335, 18.35000000122903074, 32.30940107675850470 ) ) ;
#10537 = CARTESIAN_POINT ( 'NONE',  ( 12.41249999999999964, 2.886751345948126879, 4.999999999999999112 ) ) ;
#10538 = CARTESIAN_POINT ( 'NONE',  ( 21.45000000122903216, 5.773502691896255534, 3.535250795749688894E-16 ) ) ;
#10539 = CARTESIAN_POINT ( 'NONE',  ( 16.56562500061451715, 3.027376345333613106, -5.243569643749998122 ) ) ;
#10540 = CARTESIAN_POINT ( 'NONE',  ( 11.97187500061451537, 5.824947211148865298E-16, -4.756430356249998326 ) ) ;
#10541 = ORIENTED_EDGE ( 'NONE', *, *, #64554, .F. ) ;
#10542 = CARTESIAN_POINT ( 'NONE',  ( 19.31250000000000000, -5.773502691896255534, -1.060575238724906372E-15 ) ) ;
#10543 = CARTESIAN_POINT ( 'NONE',  ( 21.75937500061451502, 0.000000000000000000, 5.243569643749999010 ) ) ;
#10544 = CARTESIAN_POINT ( 'NONE',  ( 27.47812500061451502, 4.541064518000418104, 2.621784821874999949 ) ) ;
#10545 = ORIENTED_EDGE ( 'NONE', *, *, #2122, .T. ) ;
#10546 = CARTESIAN_POINT ( 'NONE',  ( 1.071796769724491893, 17.88259618943233065, -26.00000000000000355 ) ) ;
#10547 = CARTESIAN_POINT ( 'NONE',  ( 11.24062500061451608, 6.054752690667223547, 3.707466751127219781E-16 ) ) ;
#10548 = CARTESIAN_POINT ( 'NONE',  ( 17.28750000122903430, 6.123233995736764310E-16, -4.999999999999998224 ) ) ;
#10549 = CARTESIAN_POINT ( 'NONE',  ( 13.99687500061451395, 0.000000000000000000, 4.756430356249998326 ) ) ;
#10550 = CARTESIAN_POINT ( 'NONE',  ( 17.21249999999999858, 2.886751345948129099, -4.999999999999998224 ) ) ;
#10551 = CARTESIAN_POINT ( 'NONE',  ( 23.92499999999999716, 6.123233995736764310E-16, -4.999999999999998224 ) ) ;
#10552 = CARTESIAN_POINT ( 'NONE',  ( 3.492642502296683382, -3.577956359659812513, -3.802396965202827772 ) ) ;
#10553 = CARTESIAN_POINT ( 'NONE',  ( 3.721875000614518036, 3.027376345333611329, 5.243569643749999010 ) ) ;
#10554 = CARTESIAN_POINT ( 'NONE',  ( 28.77187500061451431, 3.027376345333613106, -5.243569643749998122 ) ) ;
#10555 = VERTEX_POINT ( 'NONE', #31673 ) ;
#10556 = CARTESIAN_POINT ( 'NONE',  ( 26.57812500061451644, 4.541064518000418104, 2.621784821874999949 ) ) ;
#10557 = CARTESIAN_POINT ( 'NONE',  ( 24.68437500061451573, 6.421520780324663323E-16, -5.243569643749999010 ) ) ;
#10558 = CARTESIAN_POINT ( 'NONE',  ( -2.121784821874996840, 17.62812500061459176, -26.32496088578401583 ) ) ;
#10559 = CARTESIAN_POINT ( 'NONE',  ( 14.81250000000000000, -5.773502691896255534, -1.060575238724906372E-15 ) ) ;
#10560 = CARTESIAN_POINT ( 'NONE',  ( 10.94062500061451537, -3.027376345333614438, 5.243569643749998122 ) ) ;
#10561 = CARTESIAN_POINT ( 'NONE',  ( 3.774699069111469019, 3.279031861275984561, 3.945388500768145956 ) ) ;
#10562 = CARTESIAN_POINT ( 'NONE',  ( 17.13749999999999574, -2.886751345948181946, -4.999999999999904077 ) ) ;
#10563 = CARTESIAN_POINT ( 'NONE',  ( 29.69062500061451715, 6.054752690667223547, 3.707466751127219781E-16 ) ) ;
#10564 = CARTESIAN_POINT ( 'NONE',  ( 15.82500000122903216, -5.773502691896255534, -1.060575238724906372E-15 ) ) ;
#10565 = CARTESIAN_POINT ( 'NONE',  ( -6.275039685470489619E-15, 18.31250000000000000, 33.99999999999999289 ) ) ;
#10566 = CARTESIAN_POINT ( 'NONE',  ( 14.03437500061451715, 4.119189519843966529, 2.378215178124999607 ) ) ;
#10567 = CARTESIAN_POINT ( 'NONE',  ( 4.190625000614518925, -3.027376345333614438, 5.243569643749998122 ) ) ;
#10568 = CARTESIAN_POINT ( 'NONE',  ( 22.62187500061451573, 3.027376345333611329, 5.243569643749999010 ) ) ;
#10569 = CARTESIAN_POINT ( 'NONE',  ( -4.243569643749999898, 15.32187500061451679, 27.54997392385601529 ) ) ;
#10570 = CARTESIAN_POINT ( 'NONE',  ( 22.28437500061451715, -4.541064518000419881, 2.621784821874995952 ) ) ;
#10571 = CARTESIAN_POINT ( 'NONE',  ( 29.22187500061451715, 3.027376345333613106, -5.243569643749998122 ) ) ;
#10572 = CARTESIAN_POINT ( 'NONE',  ( 4.243569643749999010, 18.32187500061451502, 27.54997392385601174 ) ) ;
#10573 = CARTESIAN_POINT ( 'NONE',  ( 8.878125000614515372, 6.421520780324663323E-16, -5.243569643749999010 ) ) ;
#10574 = CARTESIAN_POINT ( 'NONE',  ( 8.025000000000000355, -4.330127018922194537, 2.499999999999995559 ) ) ;
#10575 = EDGE_CURVE ( 'NONE', #39103, #13160, #46297, .T. ) ;
#10576 = CARTESIAN_POINT ( 'NONE',  ( 6.909375000614518036, 0.000000000000000000, 5.243569643749999010 ) ) ;
#10577 = CARTESIAN_POINT ( 'NONE',  ( 13.14375000122903536, -2.886751345948126435, -5.000000000000000000 ) ) ;
#10578 = CARTESIAN_POINT ( 'NONE',  ( 7.303125000614516082, 0.000000000000000000, 5.243569643749999010 ) ) ;
#10579 = CARTESIAN_POINT ( 'NONE',  ( 10.84687500061451892, 6.054752690667223547, 3.707466751127219781E-16 ) ) ;
#10580 = CARTESIAN_POINT ( 'NONE',  ( 1.592000809091587073E-14, 16.85000000122903785, 26.00000000000000000 ) ) ;
#10581 = CARTESIAN_POINT ( 'NONE',  ( 17.92500000122903359, 2.886751345948126879, 4.999999999999999112 ) ) ;
#10582 = CARTESIAN_POINT ( 'NONE',  ( 7.809375000614519280, 0.000000000000000000, 5.243569643749999010 ) ) ;
#10583 = CARTESIAN_POINT ( 'NONE',  ( 10.75312500061451715, 4.541064518000418104, -2.621784821874998173 ) ) ;
#10584 = CARTESIAN_POINT ( 'NONE',  ( 7.228125000614517681, 4.541064518000418104, 2.621784821874999949 ) ) ;
#10585 = CARTESIAN_POINT ( 'NONE',  ( 26.56875000122903074, -5.773502691896255534, -1.060575238724906372E-15 ) ) ;
#10586 = CARTESIAN_POINT ( 'NONE',  ( 19.24687500061452283, -3.027376345333610441, -5.243569643749999898 ) ) ;
#10587 = CARTESIAN_POINT ( 'NONE',  ( 18.30000000000000071, 0.000000000000000000, 4.999999999999998224 ) ) ;
#10588 = CARTESIAN_POINT ( 'NONE',  ( 11.42812500061451608, -4.541064518000419881, 2.621784821874995952 ) ) ;
#10589 = CARTESIAN_POINT ( 'NONE',  ( 29.18437500061451573, 6.421520780324663323E-16, -5.243569643749999010 ) ) ;
#10590 = CARTESIAN_POINT ( 'NONE',  ( -4.243569643749999898, 12.20937500061451608, -30.00000000000000000 ) ) ;
#10591 = CARTESIAN_POINT ( 'NONE',  ( 13.42500000122903536, 2.886751345948126879, 4.999999999999999112 ) ) ;
#10592 = CARTESIAN_POINT ( 'NONE',  ( 2.121784821874999061, 14.25312500061451715, -33.67503911421598417 ) ) ;
#10593 = CARTESIAN_POINT ( 'NONE',  ( 14.62500000122903288, 2.886751345948129099, -4.999999999999998224 ) ) ;
#10594 = CARTESIAN_POINT ( 'NONE',  ( 10.75312500061451715, 4.541064518000418104, -2.621784821874998173 ) ) ;
#10595 = EDGE_LOOP ( 'NONE', ( #6169, #26713, #24601, #3412 ) ) ;
#10596 = CARTESIAN_POINT ( 'NONE',  ( 12.63749999999999929, -2.886751345948125991, -5.000000000000000000 ) ) ;
#10597 = CARTESIAN_POINT ( 'NONE',  ( 23.90625000122903288, -4.330127018922190985, -2.500000000000001332 ) ) ;
#10598 = CARTESIAN_POINT ( 'NONE',  ( 22.71562500061451573, -6.054752690667223547, -1.112240025338166033E-15 ) ) ;
#10599 = CARTESIAN_POINT ( 'NONE',  ( 8.484375000614518214, 6.421520780324663323E-16, -5.243569643749999010 ) ) ;
#10600 = CARTESIAN_POINT ( 'NONE',  ( 10.80000000122903536, -2.886751345948129988, 4.999999999999997335 ) ) ;
#10601 = CARTESIAN_POINT ( 'NONE',  ( 17.58750000122903145, -4.330127018922194537, 2.499999999999995559 ) ) ;
#10602 = CARTESIAN_POINT ( 'NONE',  ( 15.29062500061451679, 6.054752690667223547, 3.707466751127219781E-16 ) ) ;
#10603 = CARTESIAN_POINT ( 'NONE',  ( 18.55312500061451431, 0.000000000000000000, 5.243569643749999010 ) ) ;
#10604 = CARTESIAN_POINT ( 'NONE',  ( 25.80000000122903714, -2.886751345948125991, -5.000000000000000000 ) ) ;
#10605 = CARTESIAN_POINT ( 'NONE',  ( 27.00000000122903288, -2.886751345948129988, 4.999999999999997335 ) ) ;
#10606 = CARTESIAN_POINT ( 'NONE',  ( 21.86250000000000071, 2.886751345948126879, 4.999999999999999112 ) ) ;
#10607 = CARTESIAN_POINT ( 'NONE',  ( 3.756430356250000546, 14.47812499938548747, 27.83122392262697886 ) ) ;
#10608 = CARTESIAN_POINT ( 'NONE',  ( 25.50937500061451502, -4.541064518000417216, -2.621784821875001281 ) ) ;
#10609 = DIRECTION ( 'NONE',  ( -1.000000000000000000, -0.000000000000000000, -0.000000000000000000 ) ) ;
#10610 = CARTESIAN_POINT ( 'NONE',  ( 12.15000000122903501, -2.886751345948129988, 4.999999999999997335 ) ) ;
#10611 = CARTESIAN_POINT ( 'NONE',  ( 28.39687500061452141, 6.054752690667223547, 3.707466751127219781E-16 ) ) ;
#10612 = CARTESIAN_POINT ( 'NONE',  ( 20.78732959644809952, 2.500000000000000444, 3.499999999999999112 ) ) ;
#10613 = CARTESIAN_POINT ( 'NONE',  ( 4.209375000614516971, 0.000000000000000000, 5.243569643749999010 ) ) ;
#10614 = CARTESIAN_POINT ( 'NONE',  ( 22.64062500061451644, -3.027376345333614438, 5.243569643749998122 ) ) ;
#10615 = CARTESIAN_POINT ( 'NONE',  ( 3.756430356250000102, 14.55312499938548321, 30.00000000000000000 ) ) ;
#10616 = CARTESIAN_POINT ( 'NONE',  ( -1.394453263437886604E-15, 19.66249999999999787, -26.00000000000000000 ) ) ;
#10617 = CARTESIAN_POINT ( 'NONE',  ( 9.871875000614517504, 3.027376345333613106, -5.243569643749998122 ) ) ;
#10618 = CARTESIAN_POINT ( 'NONE',  ( 4.282566015150520933, -2.580625568709436379, 4.493093119413346770 ) ) ;
#10619 = CARTESIAN_POINT ( 'NONE',  ( 3.721875000614518036, 3.027376345333611329, 5.243569643749999010 ) ) ;
#10620 = CARTESIAN_POINT ( 'NONE',  ( 6.459375000614518747, 0.000000000000000000, 5.243569643749999010 ) ) ;
#10621 = CARTESIAN_POINT ( 'NONE',  ( 27.60937500061451644, 0.000000000000000000, 5.243569643749999010 ) ) ;
#10622 = CARTESIAN_POINT ( 'NONE',  ( 9.001249775931846008E-16, 10.46562500061459389, 34.90005215228797653 ) ) ;
#10623 = CARTESIAN_POINT ( 'NONE',  ( 20.51249999999999929, 2.886751345948126879, 4.999999999999999112 ) ) ;
#10624 = ORIENTED_EDGE ( 'NONE', *, *, #44946, .T. ) ;
#10625 = CARTESIAN_POINT ( 'NONE',  ( 27.29999999999999716, 0.000000000000000000, 4.999999999999998224 ) ) ;
#10626 =( BOUNDED_CURVE ( )  B_SPLINE_CURVE ( 2, ( #27613, #28329, #27251, #61222, #33146, #632, #10255, #55683, #10616 ),
 .UNSPECIFIED., .F., .F. ) 
 B_SPLINE_CURVE_WITH_KNOTS ( ( 3, 2, 2, 2, 3 ),
 ( 0.01086956521739130578, 0.01449275362318840597, 0.02173913043478260809, 0.02898550724637680848, 0.03260869565217391908 ),
 .UNSPECIFIED. ) 
 CURVE ( )  GEOMETRIC_REPRESENTATION_ITEM ( )  RATIONAL_B_SPLINE_CURVE ( ( 0.9330127018922194093, 0.9330127018922194093, 1.000000000000000000, 0.8660254037844387076, 1.000000000000000000, 0.8660254037844387076, 1.000000000000000000, 0.9330127018922191873, 0.9330127018922192983 ) ) 
 REPRESENTATION_ITEM ( '' )  );
#10627 = CARTESIAN_POINT ( 'NONE',  ( 28.43437500061451573, 4.541064518000418104, 2.621784821874999949 ) ) ;
#10628 = EDGE_LOOP ( 'NONE', ( #57607, #53697, #42839, #35952 ) ) ;
#10629 = CARTESIAN_POINT ( 'NONE',  ( 16.71562500061451573, 3.027376345333611329, 5.243569643749999010 ) ) ;
#10630 = CARTESIAN_POINT ( 'NONE',  ( 8.878125000614515372, 6.421520780324663323E-16, -5.243569643749999010 ) ) ;
#10631 = CARTESIAN_POINT ( 'NONE',  ( 20.52187500061451786, 5.824947211148865298E-16, -4.756430356249998326 ) ) ;
#10632 = CARTESIAN_POINT ( 'NONE',  ( 8.184375000614515727, 4.541064518000418104, 2.621784821874999949 ) ) ;
#10633 = CARTESIAN_POINT ( 'NONE',  ( 17.40000000122903145, 5.773502691896255534, 3.535250795749688894E-16 ) ) ;
#10634 = CARTESIAN_POINT ( 'NONE',  ( 7.059375000614518392, -4.541064518000417216, -2.621784821875001281 ) ) ;
#10635 = CARTESIAN_POINT ( 'NONE',  ( 11.25937500061451679, 4.541064518000418104, -2.621784821874998173 ) ) ;
#10636 = CARTESIAN_POINT ( 'NONE',  ( 23.10937500061451644, 0.000000000000000000, 5.243569643749999010 ) ) ;
#10637 = EDGE_CURVE ( 'NONE', #42547, #39133, #61392, .T. ) ;
#10638 = DIRECTION ( 'NONE',  ( -0.4999999999999975575, -0.000000000000000000, -0.8660254037844400399 ) ) ;
#10639 = VERTEX_POINT ( 'NONE', #53471 ) ;
#10640 = CARTESIAN_POINT ( 'NONE',  ( 9.600000000000001421, 4.330127018922192761, -2.499999999999997780 ) ) ;
#10641 = CARTESIAN_POINT ( 'NONE',  ( 17.59687500061451715, 6.054752690667223547, 3.707466751127219781E-16 ) ) ;
#10642 = CARTESIAN_POINT ( 'NONE',  ( 9.421875000614519990, 3.027376345333613106, -5.243569643749998122 ) ) ;
#10643 = CARTESIAN_POINT ( 'NONE',  ( 3.756430356250000546, 14.02812499938548463, 27.83122392262697886 ) ) ;
#10644 = CARTESIAN_POINT ( 'NONE',  ( 19.91250000000000142, 2.886751345948129099, -4.999999999999998224 ) ) ;
#10645 = CARTESIAN_POINT ( 'NONE',  ( -4.000000000000000000, 16.32499999999999929, 30.00000000000000000 ) ) ;
#10646 = CARTESIAN_POINT ( 'NONE',  ( 9.001249775931846008E-16, 10.52187500061451964, -25.09994784771203058 ) ) ;
#10647 = CARTESIAN_POINT ( 'NONE',  ( 21.64687500061451786, 5.492252693125287522, 3.363034840372157021E-16 ) ) ;
#10648 = CARTESIAN_POINT ( 'NONE',  ( 11.61562500061451608, 3.027376345333613106, -5.243569643749998122 ) ) ;
#10649 = CARTESIAN_POINT ( 'NONE',  ( 3.075000000000001510, -4.330127018922194537, 2.499999999999995559 ) ) ;
#10650 = CARTESIAN_POINT ( 'NONE',  ( 3.486133158594716510E-16, 19.55000000122903359, 26.00000000000000355 ) ) ;
#10651 = CARTESIAN_POINT ( 'NONE',  ( 4.204793154262189248, 2.706354874286773349, -4.204793154262189248 ) ) ;
#10652 = CARTESIAN_POINT ( 'NONE',  ( 10.95000000000000107, 4.330127018922192761, -2.499999999999997780 ) ) ;
#10653 = CARTESIAN_POINT ( 'NONE',  ( -3.999999999999999556, 15.12500000122903288, 27.69059892324149530 ) ) ;
#10654 = CARTESIAN_POINT ( 'NONE',  ( 9.262500001229033941, 4.330127018922192761, -2.499999999999997780 ) ) ;
#10655 = CARTESIAN_POINT ( 'NONE',  ( 20.97187500061451715, -6.054752690667223547, -1.112240025338166033E-15 ) ) ;
#10656 = CARTESIAN_POINT ( 'NONE',  ( 15.27187500061451786, 3.027376345333613106, -5.243569643749998122 ) ) ;
#10657 = DIRECTION ( 'NONE',  ( 0.000000000000000000, 0.000000000000000000, -1.000000000000000000 ) ) ;
#10658 = ORIENTED_EDGE ( 'NONE', *, *, #40061, .T. ) ;
#10659 = CARTESIAN_POINT ( 'NONE',  ( 15.32812500061451644, 4.541064518000418104, 2.621784821874999949 ) ) ;
#10660 = CARTESIAN_POINT ( 'NONE',  ( 29.25000000122903288, -2.886751345948129988, 4.999999999999997335 ) ) ;
#10661 = CARTESIAN_POINT ( 'NONE',  ( 15.87187500061451573, 3.027376345333611329, 5.243569643749999010 ) ) ;
#10662 = CARTESIAN_POINT ( 'NONE',  ( 27.31875000122903430, 2.886751345948098901, 5.000000000000047073 ) ) ;
#10663 = CARTESIAN_POINT ( 'NONE',  ( 17.91562500061451502, 3.027376345333613106, -5.243569643749998122 ) ) ;
#10664 = CARTESIAN_POINT ( 'NONE',  ( 18.18750000122903288, 6.123233995736764310E-16, -4.999999999999998224 ) ) ;
#10665 = CARTESIAN_POINT ( 'NONE',  ( 27.38437500061451857, 6.421520780324663323E-16, -5.243569643749999010 ) ) ;
#10666 = CARTESIAN_POINT ( 'NONE',  ( -3.000416591977282496E-16, 13.39062500061451644, 25.09994784771203058 ) ) ;
#10667 = CARTESIAN_POINT ( 'NONE',  ( 16.35937500061451644, 0.000000000000000000, 5.243569643749999010 ) ) ;
#10668 = CARTESIAN_POINT ( 'NONE',  ( 13.42500000122903536, 2.886751345948126879, 4.999999999999999112 ) ) ;
#10669 = CARTESIAN_POINT ( 'NONE',  ( 9.196875000614518569, -2.746126346562646425, 4.756430356249996549 ) ) ;
#10670 = CARTESIAN_POINT ( 'NONE',  ( 4.243569643749999010, 19.67187500061451644, -32.45002607614398471 ) ) ;
#10671 = CARTESIAN_POINT ( 'NONE',  ( 21.08437500061451786, 6.421520780324663323E-16, -5.243569643749999010 ) ) ;
#10672 = CARTESIAN_POINT ( 'NONE',  ( 22.80000000122903359, 5.773502691896255534, 3.535250795749688894E-16 ) ) ;
#10673 = CARTESIAN_POINT ( 'NONE',  ( 15.90937500061451892, 0.000000000000000000, 5.243569643749999010 ) ) ;
#10674 = CARTESIAN_POINT ( 'NONE',  ( 4.243569643749999898, 11.94687500061451857, 32.45002607614398471 ) ) ;
#10675 = CARTESIAN_POINT ( 'NONE',  ( 18.10312500061451502, 0.000000000000000000, 5.243569643749999010 ) ) ;
#10676 = ORIENTED_EDGE ( 'NONE', *, *, #35455, .T. ) ;
#10677 = ORIENTED_EDGE ( 'NONE', *, *, #7510, .T. ) ;
#10678 = CARTESIAN_POINT ( 'NONE',  ( 21.71249999999999858, 2.886751345948129099, -4.999999999999998224 ) ) ;
#10679 = CARTESIAN_POINT ( 'NONE',  ( 28.20000000122903216, 5.773502691896255534, 3.535250795749688401E-16 ) ) ;
#10680 = CARTESIAN_POINT ( 'NONE',  ( 25.19062500061451715, 6.054752690667223547, 3.707466751127219781E-16 ) ) ;
#10681 = CARTESIAN_POINT ( 'NONE',  ( 4.603125000614518569, 0.000000000000000000, 5.243569643749999010 ) ) ;
#10682 = CARTESIAN_POINT ( 'NONE',  ( 17.58750000122903145, -4.330127018922194537, 2.499999999999995559 ) ) ;
#10683 = CARTESIAN_POINT ( 'NONE',  ( 21.77812500061451928, -4.541064518000419881, 2.621784821874995952 ) ) ;
#10684 = CARTESIAN_POINT ( 'NONE',  ( 19.72499999999999787, -4.330127018922194537, 2.499999999999995559 ) ) ;
#10685 = CARTESIAN_POINT ( 'NONE',  ( 25.37812500061451715, -4.541064518000419881, 2.621784821874995952 ) ) ;
#10686 = CARTESIAN_POINT ( 'NONE',  ( 4.753125000614515372, -4.541064518000417216, -2.621784821875001281 ) ) ;
#10687 =( BOUNDED_CURVE ( )  B_SPLINE_CURVE ( 2, ( #27432, #49963, #15593, #38135, #21506, #26330, #60657 ),
 .UNSPECIFIED., .F., .F. ) 
 B_SPLINE_CURVE_WITH_KNOTS ( ( 3, 2, 2, 3 ),
 ( 0.3500000000000000333, 0.3527777777777778567, 0.3555555555555556246, 0.3583333333333333925 ),
 .UNSPECIFIED. ) 
 CURVE ( )  GEOMETRIC_REPRESENTATION_ITEM ( )  RATIONAL_B_SPLINE_CURVE ( ( 0.9999999999999973355, 0.8660254037844413721, 1.000000000000000000, 0.8660254037844387076, 1.000000000000000000, 0.8660254037844360431, 1.000000000000002665 ) ) 
 REPRESENTATION_ITEM ( '' )  );
#10688 = ORIENTED_EDGE ( 'NONE', *, *, #16624, .F. ) ;
#10689 = CARTESIAN_POINT ( 'NONE',  ( 29.84999999999999787, 4.330127018922192761, -2.499999999999997780 ) ) ;
#10690 = CARTESIAN_POINT ( 'NONE',  ( 3.553125000614516082, 4.541064518000418104, -2.621784821874998173 ) ) ;
#10691 = CARTESIAN_POINT ( 'NONE',  ( 10.84687500061451892, 5.492252693125287522, 3.363034840372157021E-16 ) ) ;
#10692 = CARTESIAN_POINT ( 'NONE',  ( -5.810221930991193690E-16, 18.98750000000000071, 26.00000000000000355 ) ) ;
#10693 = CARTESIAN_POINT ( 'NONE',  ( -2.000000000000000000, 11.48750000122903359, -33.46410161513775705 ) ) ;
#10694 = CARTESIAN_POINT ( 'NONE',  ( 2.121784821874999061, 19.25937500061451857, -33.67503911421598417 ) ) ;
#10695 = CARTESIAN_POINT ( 'NONE',  ( 8.925000000000002487, -4.330127018922194537, 2.499999999999995559 ) ) ;
#10696 = ADVANCED_FACE ( 'NONE', ( #54206 ), #60094, .F. ) ;
#10697 = CARTESIAN_POINT ( 'NONE',  ( 8.034375000614518925, 6.421520780324663323E-16, -5.243569643749999010 ) ) ;
#10698 = CARTESIAN_POINT ( 'NONE',  ( 7.500000001229034652, 5.773502691896255534, 3.535250795749688894E-16 ) ) ;
#10699 = CARTESIAN_POINT ( 'NONE',  ( 13.24687500061451750, -3.027376345333614438, 5.243569643749998122 ) ) ;
#10700 = CARTESIAN_POINT ( 'NONE',  ( 4.621875000614516615, 3.027376345333611329, 5.243569643749999010 ) ) ;
#10701 = CARTESIAN_POINT ( 'NONE',  ( -2.556497649636125342E-15, 18.87500000122903288, 34.00000000000000000 ) ) ;
#10702 = CARTESIAN_POINT ( 'NONE',  ( 19.83750000000000213, -2.886751345948126435, -5.000000000000000000 ) ) ;
#10704 = EDGE_CURVE ( 'NONE', #13105, #6716, #53851, .T. ) ;
#10703 = CARTESIAN_POINT ( 'NONE',  ( 9.309375000614517504, -4.541064518000417216, -2.621784821875001281 ) ) ;
#10705 = CARTESIAN_POINT ( 'NONE',  ( 3.999999999999999112, 17.18750000122903288, -30.00000000000000000 ) ) ;
#10706 = CARTESIAN_POINT ( 'NONE',  ( 19.15312500061451573, -4.541064518000417216, -2.621784821875001281 ) ) ;
#10707 = CARTESIAN_POINT ( 'NONE',  ( 16.72500000000000142, 6.123233995736764310E-16, -4.999999999999998224 ) ) ;
#10708 = CARTESIAN_POINT ( 'NONE',  ( -2.121784821874996840, 18.97812500061459673, 33.67503911421598417 ) ) ;
#10709 = CARTESIAN_POINT ( 'NONE',  ( 23.18437500061451573, -4.541064518000419881, 2.621784821874995952 ) ) ;
#10710 = EDGE_CURVE ( 'NONE', #38182, #50028, #68943, .T. ) ;
#10711 = CARTESIAN_POINT ( 'NONE',  ( 2.000000000000001332, 19.25000000000000000, 33.46410161513774995 ) ) ;
#10712 = CARTESIAN_POINT ( 'NONE',  ( 29.43750000122903288, 6.123233995736764310E-16, -4.999999999999998224 ) ) ;
#10713 = CARTESIAN_POINT ( 'NONE',  ( 20.70937500061451786, 2.746126346562643317, 4.756430356249998326 ) ) ;
#10714 = CARTESIAN_POINT ( 'NONE',  ( 25.07812500061451644, 6.421520780324663323E-16, -5.243569643749999010 ) ) ;
#10715 = CARTESIAN_POINT ( 'NONE',  ( 14.35312500061451679, 4.541064518000418104, -2.621784821874998173 ) ) ;
#10716 = CARTESIAN_POINT ( 'NONE',  ( 13.78125000122903288, 4.330127018922191873, 2.499999999999999556 ) ) ;
#10717 = CARTESIAN_POINT ( 'NONE',  ( 13.32187500061451502, -6.054752690667223547, -1.112240025338166033E-15 ) ) ;
#10718 = CARTESIAN_POINT ( 'NONE',  ( 16.83749999999999858, 5.773502691896255534, 3.535250795749688401E-16 ) ) ;
#10719 = CARTESIAN_POINT ( 'NONE',  ( 25.20000000122903216, -2.886751345948129988, 4.999999999999997335 ) ) ;
#10720 = CARTESIAN_POINT ( 'NONE',  ( 2.859375000614519546, 0.000000000000000000, 5.243569643749999010 ) ) ;
#10721 = CARTESIAN_POINT ( 'NONE',  ( 13.43437500061451750, 6.421520780324663323E-16, -5.243569643749999010 ) ) ;
#10722 = FACE_OUTER_BOUND ( 'NONE', #48151, .T. ) ;
#10723 = CARTESIAN_POINT ( 'NONE',  ( 30.00000000000000000, 0.000000000000000000, 0.000000000000000000 ) ) ;
#10724 = CARTESIAN_POINT ( 'NONE',  ( 30.00000000000000000, 6.123233995736764310E-16, -4.999999999999998224 ) ) ;
#10725 = CARTESIAN_POINT ( 'NONE',  ( 25.50937500061451502, -4.541064518000417216, -2.621784821875001281 ) ) ;
#10726 = CARTESIAN_POINT ( 'NONE',  ( 17.10937500061451999, 4.541064518000418104, -2.621784821874998173 ) ) ;
#10727 = CARTESIAN_POINT ( 'NONE',  ( -7.967954043666661671E-16, 14.89062499938548179, 34.33755215474603517 ) ) ;
#10728 = CARTESIAN_POINT ( 'NONE',  ( 28.04999999999999716, 4.330127018922192761, -2.499999999999997780 ) ) ;
#10729 = CARTESIAN_POINT ( 'NONE',  ( 4.725000001229034297, 2.886751345948129099, -4.999999999999998224 ) ) ;
#10730 = CARTESIAN_POINT ( 'NONE',  ( 4.687500000000000000, 5.773502691896255534, 3.535250795749688894E-16 ) ) ;
#10731 = CARTESIAN_POINT ( 'NONE',  ( 7.434375000614515727, -2.746126346562642428, -4.756430356249999214 ) ) ;
#10732 = CARTESIAN_POINT ( 'NONE',  ( 18.85312500061451502, 4.541064518000418104, -2.621784821874998173 ) ) ;
#10733 = CARTESIAN_POINT ( 'NONE',  ( 9.000000000000001776, -4.330127018922190985, -2.500000000000001332 ) ) ;
#10734 = CARTESIAN_POINT ( 'NONE',  ( 17.47499999999999787, -4.330127018922194537, 2.499999999999995559 ) ) ;
#10735 = DIRECTION ( 'NONE',  ( -0.000000000000000000, -1.000000000000000000, -0.000000000000000000 ) ) ;
#10736 = CARTESIAN_POINT ( 'NONE',  ( 20.10000000122903074, 5.773502691896255534, 3.535250795749688894E-16 ) ) ;
#10737 = CARTESIAN_POINT ( 'NONE',  ( 0.4052273161492640496, 10.00000000000000000, 36.00000000000000711 ) ) ;
#10738 = CARTESIAN_POINT ( 'NONE',  ( 27.45937500061451786, 4.541064518000418104, -2.621784821874998173 ) ) ;
#10739 = ORIENTED_EDGE ( 'NONE', *, *, #58225, .F. ) ;
#10740 = CARTESIAN_POINT ( 'NONE',  ( 16.07812500061451289, 6.421520780324663323E-16, -5.243569643749999010 ) ) ;
#10741 = CARTESIAN_POINT ( 'NONE',  ( 23.57812500061451289, -4.541064518000419881, 2.621784821874995952 ) ) ;
#10742 = CARTESIAN_POINT ( 'NONE',  ( 22.50937500061451857, 4.541064518000418104, -2.621784821874998173 ) ) ;
#10743 = CARTESIAN_POINT ( 'NONE',  ( 5.737499999999998934, -2.886751345948129988, 4.999999999999997335 ) ) ;
#10744 = CARTESIAN_POINT ( 'NONE',  ( 9.703125000614514661, -4.541064518000417216, -2.621784821875001281 ) ) ;
#10745 = CARTESIAN_POINT ( 'NONE',  ( 24.92812500061451431, -4.541064518000419881, 2.621784821874995952 ) ) ;
#10746 = CARTESIAN_POINT ( 'NONE',  ( 14.89687500061451786, 6.054752690667223547, 3.707466751127219781E-16 ) ) ;
#10747 = CARTESIAN_POINT ( 'NONE',  ( 20.14687500061451786, -3.027376345333610441, -5.243569643749999898 ) ) ;
#10748 = CARTESIAN_POINT ( 'NONE',  ( 19.87500000000000000, 6.123233995736764310E-16, -4.999999999999998224 ) ) ;
#10749 = CARTESIAN_POINT ( 'NONE',  ( -4.243569643749999898, 19.35312500061451857, 30.00000000000000000 ) ) ;
#10750 = EDGE_CURVE ( 'NONE', #67289, #3601, #4697, .T. ) ;
#10751 = CARTESIAN_POINT ( 'NONE',  ( 20.77500000122903145, -5.773502691896255534, -1.060575238724906372E-15 ) ) ;
#10752 = CARTESIAN_POINT ( 'NONE',  ( 16.43437500061451573, -4.119189519843968306, 2.378215178124996054 ) ) ;
#10753 = CARTESIAN_POINT ( 'NONE',  ( 12.59062500061451573, 6.054752690667223547, 3.707466751127219781E-16 ) ) ;
#10754 = CARTESIAN_POINT ( 'NONE',  ( 8.784375000614518925, -4.541064518000419881, 2.621784821874995952 ) ) ;
#10755 = CARTESIAN_POINT ( 'NONE',  ( 6.496875000614517504, -3.027376345333614438, 5.243569643749998122 ) ) ;
#10756 = ORIENTED_EDGE ( 'NONE', *, *, #27024, .T. ) ;
#10757 = CARTESIAN_POINT ( 'NONE',  ( 28.20937500061451786, -4.541064518000417216, -2.621784821875001281 ) ) ;
#10758 = CARTESIAN_POINT ( 'NONE',  ( 19.97812500061451502, -4.541064518000419881, 2.621784821874995952 ) ) ;
#10759 = CARTESIAN_POINT ( 'NONE',  ( 2.990625000614519191, -3.027376345333610441, -5.243569643749999898 ) ) ;
#10760 = CARTESIAN_POINT ( 'NONE',  ( 27.62812500061451360, -4.541064518000419881, 2.621784821874995952 ) ) ;
#10761 = CARTESIAN_POINT ( 'NONE',  ( 24.94687500061451502, -3.027376345333614438, 5.243569643749998122 ) ) ;
#10762 = CARTESIAN_POINT ( 'NONE',  ( 19.90312500061451573, 0.000000000000000000, 5.243569643749999010 ) ) ;
#10763 = CARTESIAN_POINT ( 'NONE',  ( -2.121784821874999949, 18.43437500061451928, 26.32496088578401938 ) ) ;
#10764 = CARTESIAN_POINT ( 'NONE',  ( 25.07812500061451644, 6.421520780324663323E-16, -5.243569643749999010 ) ) ;
#10765 = CARTESIAN_POINT ( 'NONE',  ( 5.812500001229035540, 0.000000000000000000, 4.999999999999998224 ) ) ;
#10766 = ORIENTED_EDGE ( 'NONE', *, *, #10575, .T. ) ;
#10767 = CARTESIAN_POINT ( 'NONE',  ( 28.83749999999999858, -2.886751345948125991, -5.000000000000000000 ) ) ;
#10768 = CARTESIAN_POINT ( 'NONE',  ( 2.000000000000001332, 16.10000000000000142, -26.53589838486224650 ) ) ;
#10769 = CARTESIAN_POINT ( 'NONE',  ( -1.878215178124999163, 16.50312499938548427, 26.74683588394047007 ) ) ;
#10770 = CARTESIAN_POINT ( 'NONE',  ( 3.759375000614517681, 0.000000000000000000, 5.243569643749999010 ) ) ;
#10771 = CARTESIAN_POINT ( 'NONE',  ( 13.04062500061451502, 6.054752690667223547, 3.707466751127219781E-16 ) ) ;
#10772 = CARTESIAN_POINT ( 'NONE',  ( 6.834375000614518747, 4.541064518000418104, 2.621784821874999949 ) ) ;
#10773 = CARTESIAN_POINT ( 'NONE',  ( 24.07500000122903216, 2.886751345948129099, -4.999999999999998224 ) ) ;
#10774 = CARTESIAN_POINT ( 'NONE',  ( 14.22187500061451892, -6.054752690667223547, -1.112240025338166033E-15 ) ) ;
#10775 = CARTESIAN_POINT ( 'NONE',  ( 3.534375000614518036, 6.421520780324663323E-16, -5.243569643749999010 ) ) ;
#10776 = CARTESIAN_POINT ( 'NONE',  ( 7.987500001229032698, 4.330127018922191873, 2.499999999999999556 ) ) ;
#10777 = CARTESIAN_POINT ( 'NONE',  ( 26.29687500061451644, -3.027376345333614438, 5.243569643749998122 ) ) ;
#10778 = CARTESIAN_POINT ( 'NONE',  ( 3.890625000614517326, -3.027376345333610441, -5.243569643749999898 ) ) ;
#10779 = CARTESIAN_POINT ( 'NONE',  ( 13.37812500061451715, 6.421520780324663323E-16, -5.243569643749999010 ) ) ;
#10780 = ORIENTED_EDGE ( 'NONE', *, *, #14213, .F. ) ;
#10781 = CARTESIAN_POINT ( 'NONE',  ( 11.05312500061451608, -4.541064518000417216, -2.621784821875001281 ) ) ;
#10782 = CARTESIAN_POINT ( 'NONE',  ( 7.265625000614516438, 3.027376345333611329, 5.243569643749999010 ) ) ;
#10783 = CARTESIAN_POINT ( 'NONE',  ( 18.87187500061451573, 2.746126346562645981, -4.756430356249997438 ) ) ;
#10784 = CARTESIAN_POINT ( 'NONE',  ( 30.00000000000000000, 0.000000000000000000, 0.000000000000000000 ) ) ;
#10785 = CARTESIAN_POINT ( 'NONE',  ( 16.38749999999999929, 5.773502691896255534, 3.535250795749688894E-16 ) ) ;
#10786 = CARTESIAN_POINT ( 'NONE',  ( 17.03437500061451715, 6.421520780324663323E-16, -5.243569643749999010 ) ) ;
#10787 = CARTESIAN_POINT ( 'NONE',  ( 14.81250000122903288, 0.000000000000000000, 4.999999999999998224 ) ) ;
#10788 = CARTESIAN_POINT ( 'NONE',  ( 19.38749999999999929, -2.886751345948125991, -5.000000000000000000 ) ) ;
#10789 = CARTESIAN_POINT ( 'NONE',  ( 4.243569643749999010, 14.66562500061451857, -32.45002607614398471 ) ) ;
#10790 = CARTESIAN_POINT ( 'NONE',  ( -1.071796769724490339, 19.83259618943233704, 26.00000000000000000 ) ) ;
#10791 = CARTESIAN_POINT ( 'NONE',  ( 25.13437500061451502, 5.492252693125287522, 3.363034840372157021E-16 ) ) ;
#10792 = CARTESIAN_POINT ( 'NONE',  ( 23.98125000122903216, 6.123233995736764310E-16, -4.999999999999998224 ) ) ;
#10793 = CARTESIAN_POINT ( 'NONE',  ( 26.46562500061451573, 3.027376345333613106, -5.243569643749998122 ) ) ;
#10794 = CARTESIAN_POINT ( 'NONE',  ( 3.999999999999998668, 19.81250000000000000, 27.69059892324149530 ) ) ;
#10795 = CARTESIAN_POINT ( 'NONE',  ( 24.37500000000000000, 6.123233995736764310E-16, -4.999999999999998224 ) ) ;
#10796 = EDGE_CURVE ( 'NONE', #17653, #48156, #18435, .T. ) ;
#10797 = CARTESIAN_POINT ( 'NONE',  ( 26.73749999999999716, 5.773502691896255534, 3.535250795749688894E-16 ) ) ;
#10798 = CARTESIAN_POINT ( 'NONE',  ( 8.390625000614518214, -3.027376345333610441, -5.243569643749999898 ) ) ;
#10799 = CARTESIAN_POINT ( 'NONE',  ( 26.22187500061451360, -4.119189519843968306, 2.378215178124996054 ) ) ;
#10800 = CARTESIAN_POINT ( 'NONE',  ( 22.50937500061451857, 4.541064518000418104, -2.621784821874998173 ) ) ;
#10801 = CARTESIAN_POINT ( 'NONE',  ( 12.94687500061451502, 4.119189519843966529, -2.378215178124998275 ) ) ;
#10802 = CARTESIAN_POINT ( 'NONE',  ( 4.415625000614518569, 3.027376345333613106, -5.243569643749998122 ) ) ;
#10803 = CARTESIAN_POINT ( 'NONE',  ( 10.80937500061451928, 4.541064518000418104, -2.621784821874998173 ) ) ;
#10804 = VERTEX_POINT ( 'NONE', #67128 ) ;
#10805 = CARTESIAN_POINT ( 'NONE',  ( 20.74687500061451573, 6.054752690667223547, 3.707466751127219781E-16 ) ) ;
#10806 = CARTESIAN_POINT ( 'NONE',  ( 3.963750086740945200, 3.047826611959361109, -30.55459297196504309 ) ) ;
#10807 = CARTESIAN_POINT ( 'NONE',  ( 28.61249999999999716, 2.886751345948126879, 4.999999999999999112 ) ) ;
#10808 = CARTESIAN_POINT ( 'NONE',  ( 5.437500000000001776, -2.886751345948125991, -5.000000000000000000 ) ) ;
#10809 = CARTESIAN_POINT ( 'NONE',  ( 13.83750000122903323, 4.330127018922191873, 2.499999999999999556 ) ) ;
#10810 = CARTESIAN_POINT ( 'NONE',  ( 3.999999999999998668, 15.31250000000000000, -32.30940107675850470 ) ) ;
#10811 = CARTESIAN_POINT ( 'NONE',  ( 18.59999999999999787, 4.330127018922192761, -2.499999999999997780 ) ) ;
#10812 = PRESENTATION_LAYER_ASSIGNMENT (  '', '', ( #3706 ) ) ;
#10813 = ORIENTED_EDGE ( 'NONE', *, *, #69202, .F. ) ;
#10814 = CARTESIAN_POINT ( 'NONE',  ( 11.77500000000000036, 6.123233995736764310E-16, -4.999999999999998224 ) ) ;
#10815 = CARTESIAN_POINT ( 'NONE',  ( 17.58749999999999858, -2.886751345948125991, -5.000000000000000000 ) ) ;
#10816 = CARTESIAN_POINT ( 'NONE',  ( 12.18750000122903465, -4.330127018922194537, 2.499999999999995559 ) ) ;
#10817 = CARTESIAN_POINT ( 'NONE',  ( 12.21562500061451573, 3.027376345333611329, 5.243569643749999010 ) ) ;
#10818 = CARTESIAN_POINT ( 'NONE',  ( 8.099999999999999645, -4.330127018922190985, -2.500000000000001332 ) ) ;
#10819 = CARTESIAN_POINT ( 'NONE',  ( -4.243569643749999898, 14.87187500061451928, -32.45002607614398471 ) ) ;
#10820 = CARTESIAN_POINT ( 'NONE',  ( 28.80000000122903003, -2.886751345948129988, 4.999999999999997335 ) ) ;
#10821 = CARTESIAN_POINT ( 'NONE',  ( -3.756430356249999214, 14.17812499938548498, 27.83122392262697176 ) ) ;
#10822 = CARTESIAN_POINT ( 'NONE',  ( 11.06250000000000000, 2.886751345948126879, 4.999999999999999112 ) ) ;
#10823 = CARTESIAN_POINT ( 'NONE',  ( 0.000000000000000000, 20.00000000000000000, -30.00000000000000000 ) ) ;
#10824 = VERTEX_POINT ( 'NONE', #39042 ) ;
#10825 = CARTESIAN_POINT ( 'NONE',  ( 25.34062500061451217, -3.027376345333614438, 5.243569643749998122 ) ) ;
#10826 = CARTESIAN_POINT ( 'NONE',  ( 29.32500000122903216, -5.773502691896255534, -1.060575238724906372E-15 ) ) ;
#10827 = CARTESIAN_POINT ( 'NONE',  ( 29.14687500061451075, -3.027376345333610441, -5.243569643749999898 ) ) ;
#10828 = CARTESIAN_POINT ( 'NONE',  ( 22.13437500061451502, 4.541064518000418104, 2.621784821874999949 ) ) ;
#10829 = CARTESIAN_POINT ( 'NONE',  ( 15.85312500061451857, 0.000000000000000000, 5.243569643749999010 ) ) ;
#10830 = CARTESIAN_POINT ( 'NONE',  ( -4.243569643749999898, 12.56562500061459176, -32.45002607614398471 ) ) ;
#10831 = CARTESIAN_POINT ( 'NONE',  ( 7.265625000614516438, 3.027376345333611329, 5.243569643749999010 ) ) ;
#10832 = CARTESIAN_POINT ( 'NONE',  ( 28.57500000122903572, 2.886751345948129099, -4.999999999999998224 ) ) ;
#10833 = CARTESIAN_POINT ( 'NONE',  ( 23.67187500061451644, -5.492252693125287522, -1.008910452111647106E-15 ) ) ;
#10834 = CARTESIAN_POINT ( 'NONE',  ( 17.95312500061451644, 4.541064518000418104, -2.621784821874998173 ) ) ;
#10835 = CARTESIAN_POINT ( 'NONE',  ( 7.884375000614517681, -4.119189519843968306, 2.378215178124996054 ) ) ;
#10836 = CARTESIAN_POINT ( 'NONE',  ( -7.967954043666661671E-16, 19.27812499938548640, 34.33755215474603517 ) ) ;
#10837 =( BOUNDED_CURVE ( )  B_SPLINE_CURVE ( 2, ( #67427, #11984, #49703, #6080, #27530, #72594, #16789 ),
 .UNSPECIFIED., .F., .F. ) 
 B_SPLINE_CURVE_WITH_KNOTS ( ( 3, 2, 2, 3 ),
 ( 0.4416666666666666519, 0.4444444444444444753, 0.4472222222222222987, 0.4500000000000001221 ),
 .UNSPECIFIED. ) 
 CURVE ( )  GEOMETRIC_REPRESENTATION_ITEM ( )  RATIONAL_B_SPLINE_CURVE ( ( 1.000000000000000000, 0.8660254037844387076, 1.000000000000000000, 0.8660254037844387076, 1.000000000000000000, 0.8660254037844333785, 1.000000000000005329 ) ) 
 REPRESENTATION_ITEM ( '' )  );
#10838 = CARTESIAN_POINT ( 'NONE',  ( 15.42187500061451821, 3.027376345333611329, 5.243569643749999010 ) ) ;
#10839 = CARTESIAN_POINT ( 'NONE',  ( 14.29687500061451821, -3.027376345333610441, -5.243569643749999898 ) ) ;
#10840 = CARTESIAN_POINT ( 'NONE',  ( 22.77187500061451786, -6.054752690667223547, -1.112240025338166033E-15 ) ) ;
#10841 = EDGE_LOOP ( 'NONE', ( #65731, #3473, #38399, #20427 ) ) ;
#10842 = CARTESIAN_POINT ( 'NONE',  ( 4.243569643749999898, 12.88437500061451857, 30.00000000000000000 ) ) ;
#10843 = CARTESIAN_POINT ( 'NONE',  ( 3.478125000614517237, 6.421520780324663323E-16, -5.243569643749999010 ) ) ;
#10844 = CARTESIAN_POINT ( 'NONE',  ( 27.17812500061451786, -4.541064518000419881, 2.621784821874995952 ) ) ;
#10845 = CARTESIAN_POINT ( 'NONE',  ( 26.39062500061451644, -3.027376345333610441, -5.243569643749999898 ) ) ;
#10846 = CARTESIAN_POINT ( 'NONE',  ( -2.000000000000001776, 17.24374999877096570, 33.46410161513775705 ) ) ;
#10847 = CARTESIAN_POINT ( 'NONE',  ( 4.000000000000000000, 16.58750000000000213, 32.30940107675849049 ) ) ;
#10848 = CARTESIAN_POINT ( 'NONE',  ( 5.971875000614516260, 3.027376345333611329, 5.243569643749999010 ) ) ;
#10849 = CARTESIAN_POINT ( 'NONE',  ( 11.51250000122903216, 4.330127018922192761, -2.499999999999997780 ) ) ;
#10850 = CARTESIAN_POINT ( 'NONE',  ( 6.375000001229031987, -5.773502691896255534, -1.060575238724906372E-15 ) ) ;
#10851 = CARTESIAN_POINT ( 'NONE',  ( 3.215625000614518836, 3.027376345333611329, 5.243569643749999010 ) ) ;
#10852 = CARTESIAN_POINT ( 'NONE',  ( -8.484601909799255319E-16, 18.18124999877096215, 34.61880215351700940 ) ) ;
#10853 = CARTESIAN_POINT ( 'NONE',  ( 19.70625000122903359, 0.000000000000000000, 4.999999999999998224 ) ) ;
#10854 = CARTESIAN_POINT ( 'NONE',  ( 12.12187500061451573, 3.027376345333613106, -5.243569643749998122 ) ) ;
#10855 = CARTESIAN_POINT ( 'NONE',  ( 1.071796769724489895, 14.91740381056766829, -34.00000000000000000 ) ) ;
#10856 = EDGE_LOOP ( 'NONE', ( #28024, #19160, #53321, #31491 ) ) ;
#10857 = ADVANCED_FACE ( 'NONE', ( #33125 ), #55662, .T. ) ;
#10858 = CARTESIAN_POINT ( 'NONE',  ( 19.64062500061451644, -3.027376345333610441, -5.243569643749999898 ) ) ;
#10859 = CARTESIAN_POINT ( 'NONE',  ( 13.50937500061451679, 4.541064518000418104, -2.621784821874998173 ) ) ;
#10860 = CARTESIAN_POINT ( 'NONE',  ( 4.528125000614516615, 4.541064518000418104, 2.621784821874999949 ) ) ;
#10861 = CARTESIAN_POINT ( 'NONE',  ( 21.57187500061451502, 3.027376345333612662, -5.243569643749998122 ) ) ;
#10862 = CARTESIAN_POINT ( 'NONE',  ( 9.421875000614519990, 3.027376345333613106, -5.243569643749998122 ) ) ;
#10863 = CARTESIAN_POINT ( 'NONE',  ( 4.340625000614515727, -3.027376345333610441, -5.243569643749999898 ) ) ;
#10864 = CARTESIAN_POINT ( 'NONE',  ( 10.80000000122903536, -2.886751345948130876, 4.999999999999996447 ) ) ;
#10865 = CARTESIAN_POINT ( 'NONE',  ( 6.637500001229035718, 4.330127018922191873, 2.499999999999999556 ) ) ;
#10866 = CARTESIAN_POINT ( 'NONE',  ( 20.39062500061451644, -3.027376345333614438, 5.243569643749998122 ) ) ;
#10867 = CARTESIAN_POINT ( 'NONE',  ( 7.425000001229034474, 2.886751345948129099, -4.999999999999998224 ) ) ;
#10868 = CARTESIAN_POINT ( 'NONE',  ( 16.82812500061451644, -4.541064518000419881, 2.621784821874995952 ) ) ;
#10869 = CARTESIAN_POINT ( 'NONE',  ( 16.71562500061451573, 3.027376345333611329, 5.243569643749999010 ) ) ;
#10870 = CARTESIAN_POINT ( 'NONE',  ( 25.43437500061451573, -4.119189519843968306, 2.378215178124996054 ) ) ;
#10871 = CARTESIAN_POINT ( 'NONE',  ( 16.35000000000000142, 4.330127018922192761, -2.499999999999997780 ) ) ;
#10872 = CARTESIAN_POINT ( 'NONE',  ( 8.700000001229032165, -2.886751345948125991, -5.000000000000000000 ) ) ;
#10873 = CARTESIAN_POINT ( 'NONE',  ( 6.215625000614517504, 3.027376345333613106, -5.243569643749998122 ) ) ;
#10874 = CARTESIAN_POINT ( 'NONE',  ( 20.25000000122903288, -2.886751345948129988, 4.999999999999997335 ) ) ;
#10875 = CARTESIAN_POINT ( 'NONE',  ( 26.96249999999999858, -5.773502691896255534, -1.060575238724906372E-15 ) ) ;
#10876 = CARTESIAN_POINT ( 'NONE',  ( 4.243569643749999898, 12.88437500061451857, -30.00000000000000000 ) ) ;
#10877 = CARTESIAN_POINT ( 'NONE',  ( 30.00000000000000000, 6.123233995736764310E-16, -4.999999999999998224 ) ) ;
#10878 = VECTOR ( 'NONE', #14421, 1000.000000000000000 ) ;
#10879 = CARTESIAN_POINT ( 'NONE',  ( 3.037500001229032964, 4.330127018922191873, 2.499999999999999556 ) ) ;
#10880 =( BOUNDED_CURVE ( )  B_SPLINE_CURVE ( 2, ( #43956, #72023, #21400, #5518, #27325, #33938, #4069, #66478, #15856 ),
 .UNSPECIFIED., .F., .F. ) 
 B_SPLINE_CURVE_WITH_KNOTS ( ( 3, 2, 2, 2, 3 ),
 ( 0.01388888888888888985, 0.01851851851851851749, 0.02777777777777777624, 0.03703703703703703498, 0.04166666666666667129 ),
 .UNSPECIFIED. ) 
 CURVE ( )  GEOMETRIC_REPRESENTATION_ITEM ( )  RATIONAL_B_SPLINE_CURVE ( ( 0.9330127018922194093, 0.9330127018922194093, 1.000000000000000000, 0.8660254037844387076, 1.000000000000000000, 0.8660254037844387076, 1.000000000000000000, 0.9330127018922191873, 0.9330127018922192983 ) ) 
 REPRESENTATION_ITEM ( '' )  );
#10881 = CARTESIAN_POINT ( 'NONE',  ( 5.184375000614516615, -4.541064518000419881, 2.621784821874995952 ) ) ;
#10882 = CARTESIAN_POINT ( 'NONE',  ( 19.73437500061451644, 6.421520780324663323E-16, -5.243569643749999010 ) ) ;
#10883 = EDGE_CURVE ( 'NONE', #61284, #27013, #33559, .T. ) ;
#10884 = CARTESIAN_POINT ( 'NONE',  ( 12.41249999999999609, 2.886751345948193936, 4.999999999999883649 ) ) ;
#10885 = CARTESIAN_POINT ( 'NONE',  ( 15.40312500061451573, 0.000000000000000000, 5.243569643749999010 ) ) ;
#10886 = CARTESIAN_POINT ( 'NONE',  ( 12.58125000122903359, -4.330127018922194537, 2.499999999999995559 ) ) ;
#10887 = CARTESIAN_POINT ( 'NONE',  ( 13.16250000000000142, 2.886751345948129099, -4.999999999999997335 ) ) ;
#10888 = DIRECTION ( 'NONE',  ( 0.000000000000000000, 0.000000000000000000, 1.000000000000000000 ) ) ;
#10889 = CARTESIAN_POINT ( 'NONE',  ( 29.48437500061451644, -4.541064518000419881, 2.621784821874995952 ) ) ;
#10890 = CARTESIAN_POINT ( 'NONE',  ( 21.08437500061451786, 5.492252693125287522, 3.363034840372157021E-16 ) ) ;
#10891 = CARTESIAN_POINT ( 'NONE',  ( 16.04062500061451857, -3.027376345333610441, -5.243569643749999898 ) ) ;
#10892 = CARTESIAN_POINT ( 'NONE',  ( 10.80937500061451928, 4.541064518000418104, -2.621784821874998173 ) ) ;
#10893 = ORIENTED_EDGE ( 'NONE', *, *, #38374, .F. ) ;
#10894 = CARTESIAN_POINT ( 'NONE',  ( 28.82812500061451644, 4.541064518000418104, 2.621784821874999949 ) ) ;
#10895 = CARTESIAN_POINT ( 'NONE',  ( 22.86562500061451431, 3.027376345333613106, -5.243569643749998122 ) ) ;
#10896 = CARTESIAN_POINT ( 'NONE',  ( -1.071796769724488563, 13.00490381179669974, 34.00000000000000000 ) ) ;
#10897 = CARTESIAN_POINT ( 'NONE',  ( 12.48750000000000249, -2.886751345948129988, 4.999999999999997335 ) ) ;
#10898 = CARTESIAN_POINT ( 'NONE',  ( 22.65000000122903856, -2.886751345948125991, -5.000000000000000000 ) ) ;
#10899 = CARTESIAN_POINT ( 'NONE',  ( 16.52812500061451573, 6.421520780324663323E-16, -5.243569643749999010 ) ) ;
#10900 = CARTESIAN_POINT ( 'NONE',  ( 12.30937500061451750, -5.492252693125287522, -1.008910452111647106E-15 ) ) ;
#10901 = ORIENTED_EDGE ( 'NONE', *, *, #10796, .F. ) ;
#10902 = CARTESIAN_POINT ( 'NONE',  ( 20.96250000000000213, 2.886751345948126879, 4.999999999999999112 ) ) ;
#10903 = CARTESIAN_POINT ( 'NONE',  ( 22.05937500061451573, 4.541064518000418104, -2.621784821874998173 ) ) ;
#10904 = CARTESIAN_POINT ( 'NONE',  ( 26.69062500061451715, -3.027376345333614438, 5.243569643749998122 ) ) ;
#10905 =( BOUNDED_CURVE ( )  B_SPLINE_CURVE ( 2, ( #11939, #45925, #45572, #68823, #62542, #63623, #68457 ),
 .UNSPECIFIED., .F., .F. ) 
 B_SPLINE_CURVE_WITH_KNOTS ( ( 3, 2, 2, 3 ),
 ( 0.02499999999999994935, 0.02777777777777776236, 0.03055555555555557884, 0.03333333333333339532 ),
 .UNSPECIFIED. ) 
 CURVE ( )  GEOMETRIC_REPRESENTATION_ITEM ( )  RATIONAL_B_SPLINE_CURVE ( ( 1.000000000000002442, 0.8660254037844360431, 1.000000000000000000, 0.8660254037844387076, 1.000000000000000000, 0.8660254037844357100, 1.000000000000003109 ) ) 
 REPRESENTATION_ITEM ( '' )  );
#10906 = ORIENTED_EDGE ( 'NONE', *, *, #24383, .F. ) ;
#10907 = CARTESIAN_POINT ( 'NONE',  ( 19.87500000000000000, 6.123233995736764310E-16, -4.999999999999998224 ) ) ;
#10908 = CARTESIAN_POINT ( 'NONE',  ( 9.140625000614518214, -3.027376345333614438, 5.243569643749998122 ) ) ;
#10909 = DIRECTION ( 'NONE',  ( 0.000000000000000000, 0.000000000000000000, 1.000000000000000000 ) ) ;
#10910 = CARTESIAN_POINT ( 'NONE',  ( 17.47499999999999787, -4.330127018922194537, 2.499999999999995559 ) ) ;
#10911 = CARTESIAN_POINT ( 'NONE',  ( 24.22500000000000142, -4.330127018922194537, 2.499999999999995559 ) ) ;
#10912 = CARTESIAN_POINT ( 'NONE',  ( 7.912499999999999645, 2.886751345948126879, 4.999999999999998224 ) ) ;
#10913 = CARTESIAN_POINT ( 'NONE',  ( 5.446875000614518569, 6.054752690667223547, 3.707466751127219781E-16 ) ) ;
#10914 = CARTESIAN_POINT ( 'NONE',  ( 29.40937500061451715, 0.000000000000000000, 5.243569643749999010 ) ) ;
#10915 = ORIENTED_EDGE ( 'NONE', *, *, #55179, .F. ) ;
#10916 = CARTESIAN_POINT ( 'NONE',  ( 24.02812500061451573, -4.541064518000419881, 2.621784821874995952 ) ) ;
#10917 = CARTESIAN_POINT ( 'NONE',  ( 24.57187500061451502, -6.054752690667223547, -1.112240025338166033E-15 ) ) ;
#10918 = DIRECTION ( 'NONE',  ( 0.000000000000000000, 0.000000000000000000, -1.000000000000000000 ) ) ;
#10919 = CARTESIAN_POINT ( 'NONE',  ( 14.06250000000000000, 2.886751345948129099, -4.999999999999998224 ) ) ;
#10920 = CARTESIAN_POINT ( 'NONE',  ( 7.715625000614515727, 3.027376345333611329, 5.243569643749999010 ) ) ;
#10921 = CYLINDRICAL_SURFACE ( 'NONE', #24494, 4.999999999999998224 ) ;
#10922 = CARTESIAN_POINT ( 'NONE',  ( 17.17500000000000071, 6.123233995736764310E-16, -4.999999999999998224 ) ) ;
#10923 = CARTESIAN_POINT ( 'NONE',  ( 25.30312500061451431, 0.000000000000000000, 5.243569643749999010 ) ) ;
#10924 = CARTESIAN_POINT ( 'NONE',  ( 29.74687500061451573, 0.000000000000000000, 4.756430356249998326 ) ) ;
#10925 = CARTESIAN_POINT ( 'NONE',  ( 14.29687500061451821, -2.746126346562642428, -4.756430356249999214 ) ) ;
#10926 = CARTESIAN_POINT ( 'NONE',  ( 3.853125000614517681, -4.541064518000417216, -2.621784821875001281 ) ) ;
#10927 = CARTESIAN_POINT ( 'NONE',  ( 19.95937500061451786, 0.000000000000000000, 5.243569643749999010 ) ) ;
#10928 = CARTESIAN_POINT ( 'NONE',  ( -2.121784821874996840, 13.63437500061451857, 33.67503911421598417 ) ) ;
#10929 = CARTESIAN_POINT ( 'NONE',  ( 22.39687500061451075, -3.027376345333610441, -5.243569643749999898 ) ) ;
#10930 = CARTESIAN_POINT ( 'NONE',  ( 3.037500000000002309, -2.886751345948129988, 4.999999999999997335 ) ) ;
#10931 = CARTESIAN_POINT ( 'NONE',  ( 2.121784821874999061, 19.25937500061451857, 26.32496088578401583 ) ) ;
#10932 = CARTESIAN_POINT ( 'NONE',  ( 9.853125000614516793, 4.541064518000418104, -2.621784821874998173 ) ) ;
#10933 = CARTESIAN_POINT ( 'NONE',  ( 7.987500000000000711, -2.886751345948130876, 4.999999999999996447 ) ) ;
#10934 = ADVANCED_BREP_SHAPE_REPRESENTATION ( '', ( #45331, #23765 ), #1386 ) ;
#10935 = CIRCLE ( 'NONE', #61649, 14.99999999999999822 ) ;
#10936 = CARTESIAN_POINT ( 'NONE',  ( 6.684375000614518392, 6.421520780324663323E-16, -5.243569643749999010 ) ) ;
#10937 = LINE ( 'NONE', #43098, #24203 ) ;
#10938 =( BOUNDED_CURVE ( )  B_SPLINE_CURVE ( 2, ( #53830, #60444, #71553, #10222, #66004, #54195, #3223 ),
 .UNSPECIFIED., .F., .F. ) 
 B_SPLINE_CURVE_WITH_KNOTS ( ( 3, 2, 2, 3 ),
 ( 0.5833333333333334814, 0.5861111111111112493, 0.5888888888888890172, 0.5916666666666667851 ),
 .UNSPECIFIED. ) 
 CURVE ( )  GEOMETRIC_REPRESENTATION_ITEM ( )  RATIONAL_B_SPLINE_CURVE ( ( 0.9999999999999946709, 0.8660254037844440367, 1.000000000000000000, 0.8660254037844387076, 1.000000000000000000, 0.8660254037844333785, 1.000000000000005329 ) ) 
 REPRESENTATION_ITEM ( '' )  );
#10939 = CARTESIAN_POINT ( 'NONE',  ( 8.353125000614518569, -4.541064518000417216, -2.621784821875001281 ) ) ;
#10940 = CARTESIAN_POINT ( 'NONE',  ( 11.85937500061451644, 0.000000000000000000, 5.243569643749999010 ) ) ;
#10941 = SURFACE_SIDE_STYLE ('',( #62985 ) ) ;
#10942 = CARTESIAN_POINT ( 'NONE',  ( 18.97500000122903074, -5.773502691896255534, -1.060575238724906372E-15 ) ) ;
#10943 = CARTESIAN_POINT ( 'NONE',  ( 8.934375000614517504, 6.421520780324663323E-16, -5.243569643749999010 ) ) ;
#10944 = CARTESIAN_POINT ( 'NONE',  ( 10.90312500061451928, 0.000000000000000000, 5.243569643749999010 ) ) ;
#10945 = CARTESIAN_POINT ( 'NONE',  ( 5.615625000614517859, -6.054752690667223547, -1.112240025338166033E-15 ) ) ;
#10946 = CARTESIAN_POINT ( 'NONE',  ( 25.36875000122903501, 2.886751345948129099, -4.999999999999998224 ) ) ;
#10947 = CARTESIAN_POINT ( 'NONE',  ( 18.38437500061451857, 6.421520780324663323E-16, -5.243569643749999010 ) ) ;
#10948 = CARTESIAN_POINT ( 'NONE',  ( 9.806250001229033231, 0.000000000000000000, 4.999999999999998224 ) ) ;
#10949 = CARTESIAN_POINT ( 'NONE',  ( 26.69062500061451715, -3.027376345333614438, 5.243569643749998122 ) ) ;
#10950 = CARTESIAN_POINT ( 'NONE',  ( 12.55312500061451786, 4.541064518000418104, -2.621784821874998173 ) ) ;
#10951 = CARTESIAN_POINT ( 'NONE',  ( 28.28437500061451715, 6.421520780324663323E-16, -5.243569643749999010 ) ) ;
#10952 = CARTESIAN_POINT ( 'NONE',  ( -4.243569643749999898, 12.62187500061451750, -32.45002607614398471 ) ) ;
#10953 = CARTESIAN_POINT ( 'NONE',  ( 13.31250000122903288, 4.330127018922192761, -2.499999999999997780 ) ) ;
#10954 = CARTESIAN_POINT ( 'NONE',  ( 27.89062500061451289, 6.054752690667223547, 3.707466751127219781E-16 ) ) ;
#10955 = CARTESIAN_POINT ( 'NONE',  ( 2.121784821875001281, 15.45312500061451644, -26.32496088578401938 ) ) ;
#10956 = CARTESIAN_POINT ( 'NONE',  ( 14.77500000122903501, 2.886751345948126879, 4.999999999999999112 ) ) ;
#10957 = CARTESIAN_POINT ( 'NONE',  ( 13.12500000000000178, 6.123233995736764310E-16, -4.999999999999998224 ) ) ;
#10958 = CARTESIAN_POINT ( 'NONE',  ( 23.86875000122903501, -5.773502691896255534, -1.060575238724906372E-15 ) ) ;
#10959 = CARTESIAN_POINT ( 'NONE',  ( 23.76562500061451644, 3.027376345333613106, -5.243569643749998122 ) ) ;
#10960 = CARTESIAN_POINT ( 'NONE',  ( 6.909375000614518036, 0.000000000000000000, 5.243569643749999010 ) ) ;
#10961 = CARTESIAN_POINT ( 'NONE',  ( 11.06250000122903288, 4.330127018922192761, -2.499999999999997780 ) ) ;
#10962 = CARTESIAN_POINT ( 'NONE',  ( 19.12500000122903288, 2.886751345948129099, -4.999999999999998224 ) ) ;
#10963 = CARTESIAN_POINT ( 'NONE',  ( 14.42812500061451786, 4.541064518000418104, 2.621784821874999949 ) ) ;
#10964 = CARTESIAN_POINT ( 'NONE',  ( 18.85312500061451502, 4.541064518000418104, -2.621784821874998173 ) ) ;
#10965 = CARTESIAN_POINT ( 'NONE',  ( 25.61250000122903359, 0.000000000000000000, 4.999999999999998224 ) ) ;
#10966 = CARTESIAN_POINT ( 'NONE',  ( 28.35000000122903430, -2.886751345948129988, 4.999999999999997335 ) ) ;
#10967 = CARTESIAN_POINT ( 'NONE',  ( 23.28750000000000142, -2.886751345948129988, 4.999999999999997335 ) ) ;
#10968 = CARTESIAN_POINT ( 'NONE',  ( 26.25937500061451857, 0.000000000000000000, 5.243569643749999010 ) ) ;
#10969 = DIRECTION ( 'NONE',  ( 0.000000000000000000, 0.000000000000000000, 1.000000000000000000 ) ) ;
#10970 = CARTESIAN_POINT ( 'NONE',  ( 13.23750000122903359, 6.123233995736764310E-16, -4.999999999999998224 ) ) ;
#10971 = EDGE_CURVE ( 'NONE', #55851, #46843, #48673, .T. ) ;
#10972 = CARTESIAN_POINT ( 'NONE',  ( 27.23437500061451644, -4.541064518000419881, 2.621784821874995952 ) ) ;
#10973 = EDGE_CURVE ( 'NONE', #42476, #59817, #63740, .T. ) ;
#10974 = CARTESIAN_POINT ( 'NONE',  ( 4.584375000614516971, 4.541064518000418104, 2.621784821874999949 ) ) ;
#10975 = CARTESIAN_POINT ( 'NONE',  ( 3.909375000614518481, -4.541064518000417216, -2.621784821875001281 ) ) ;
#10976 = CARTESIAN_POINT ( 'NONE',  ( 23.09062500061451573, -3.027376345333614438, 5.243569643749998122 ) ) ;
#10977 = CARTESIAN_POINT ( 'NONE',  ( -3.756430356250000990, 14.36562499938548321, 32.16877607737301048 ) ) ;
#10978 = CARTESIAN_POINT ( 'NONE',  ( -4.000000000000000000, 14.01874999877096606, 30.00000000000000000 ) ) ;
#10979 = CARTESIAN_POINT ( 'NONE',  ( 10.43437500061451750, 4.541064518000418104, 2.621784821874999949 ) ) ;
#10980 = CARTESIAN_POINT ( 'NONE',  ( 4.000000000000000000, 12.53749999999999964, 32.30940107675849760 ) ) ;
#10981 = CARTESIAN_POINT ( 'NONE',  ( 29.27812500061451573, 4.541064518000418104, 2.621784821874999949 ) ) ;
#10982 = CARTESIAN_POINT ( 'NONE',  ( 7.209375000614519635, 4.541064518000418104, -2.621784821874998173 ) ) ;
#10983 = CARTESIAN_POINT ( 'NONE',  ( 28.28437500061451715, 6.421520780324663323E-16, -5.243569643749999010 ) ) ;
#10984 = DIRECTION ( 'NONE',  ( 1.000000000000000000, 0.000000000000000000, 0.000000000000000000 ) ) ;
#10985 = CARTESIAN_POINT ( 'NONE',  ( 19.76250000000000639, -5.773502691896255534, -1.060575238724906372E-15 ) ) ;
#10986 = ORIENTED_EDGE ( 'NONE', *, *, #5278, .F. ) ;
#10988 = EDGE_CURVE ( 'NONE', #72145, #52358, #39406, .T. ) ;
#10987 = CARTESIAN_POINT ( 'NONE',  ( 26.39999999999999858, 0.000000000000000000, 4.999999999999998224 ) ) ;
#10989 = CARTESIAN_POINT ( 'NONE',  ( 28.28437500061451715, 6.421520780324663323E-16, -5.243569643749999010 ) ) ;
#10990 = VERTEX_POINT ( 'NONE', #61924 ) ;
#10991 = CARTESIAN_POINT ( 'NONE',  ( 18.29062500061451502, -3.027376345333610441, -5.243569643749999898 ) ) ;
#10992 = CARTESIAN_POINT ( 'NONE',  ( 9.140625000614518214, -3.027376345333614438, 5.243569643749998122 ) ) ;
#10993 = CARTESIAN_POINT ( 'NONE',  ( 20.63437500061451502, 5.492252693125287522, 3.363034840372157021E-16 ) ) ;
#10994 = CARTESIAN_POINT ( 'NONE',  ( 3.834375000614519635, -4.541064518000419881, 2.621784821874995952 ) ) ;
#10995 = CARTESIAN_POINT ( 'NONE',  ( 18.37500000122903288, 2.886751345948126879, 4.999999999999999112 ) ) ;
#10996 = CARTESIAN_POINT ( 'NONE',  ( 25.16249999999999432, -5.773502691896255534, -1.060575238724906372E-15 ) ) ;
#10997 = CARTESIAN_POINT ( 'NONE',  ( -0.6945881563830144101, 20.00000000000000000, -33.93923181508938569 ) ) ;
#10998 = CARTESIAN_POINT ( 'NONE',  ( 6.646875000614518747, -3.027376345333610441, -5.243569643749999898 ) ) ;
#10999 = CARTESIAN_POINT ( 'NONE',  ( 11.48437500061451644, -4.541064518000419881, 2.621784821874995952 ) ) ;
#11000 = CARTESIAN_POINT ( 'NONE',  ( 22.50937500061451857, 4.541064518000418104, -2.621784821874998173 ) ) ;
#11001 = FACE_OUTER_BOUND ( 'NONE', #52718, .T. ) ;
#11002 = ORIENTED_EDGE ( 'NONE', *, *, #54124, .F. ) ;
#11003 = CARTESIAN_POINT ( 'NONE',  ( 4.809375000614516615, -4.541064518000417216, -2.621784821875001281 ) ) ;
#11004 = CARTESIAN_POINT ( 'NONE',  ( 11.17500000000000071, -4.330127018922194537, 2.499999999999995559 ) ) ;
#11005 = CARTESIAN_POINT ( 'NONE',  ( 6.646875000614518747, -3.027376345333610441, -5.243569643749999898 ) ) ;
#11006 = CARTESIAN_POINT ( 'NONE',  ( 1.878215178124997609, 14.81562499938548427, 33.25316411605952993 ) ) ;
#11007 = CARTESIAN_POINT ( 'NONE',  ( 21.71249999999999858, 2.886751345948129099, -4.999999999999998224 ) ) ;
#11008 = CARTESIAN_POINT ( 'NONE',  ( 15.62812500061451537, 6.421520780324663323E-16, -5.243569643749999010 ) ) ;
#11009 = CARTESIAN_POINT ( 'NONE',  ( 2.828200636599751609E-16, 17.11250000000000071, 25.38119784648299415 ) ) ;
#11010 = CARTESIAN_POINT ( 'NONE',  ( 4.218973316782503424, 2.683427332786226582, 4.406139393528273551 ) ) ;
#11011 = CARTESIAN_POINT ( 'NONE',  ( 23.40937500061451715, 4.119189519843966529, -2.378215178124998275 ) ) ;
#11012 = CARTESIAN_POINT ( 'NONE',  ( 9.215625000614515727, -6.054752690667223547, -1.112240025338166033E-15 ) ) ;
#11013 = CARTESIAN_POINT ( 'NONE',  ( 26.07187500061451857, 3.027376345333613106, -5.243569643749998122 ) ) ;
#11014 = CARTESIAN_POINT ( 'NONE',  ( 19.76250000122903216, 0.000000000000000000, 4.999999999999998224 ) ) ;
#11015 = CARTESIAN_POINT ( 'NONE',  ( 29.03437500061451715, -4.541064518000419881, 2.621784821874995952 ) ) ;
#11016 = CARTESIAN_POINT ( 'NONE',  ( 9.299999999999998934, 0.000000000000000000, 4.999999999999998224 ) ) ;
#11017 = CARTESIAN_POINT ( 'NONE',  ( -3.999999999999997335, 14.75000000122903288, 32.30940107675850470 ) ) ;
#11018 = CARTESIAN_POINT ( 'NONE',  ( 9.225000001229034297, 2.886751345948129099, -4.999999999999998224 ) ) ;
#11019 = CARTESIAN_POINT ( 'NONE',  ( 19.13437500061451857, -4.541064518000419881, 2.621784821874995952 ) ) ;
#11020 = CARTESIAN_POINT ( 'NONE',  ( 14.14687500061451786, -3.027376345333614438, 5.243569643749998122 ) ) ;
#11021 = CARTESIAN_POINT ( 'NONE',  ( 9.412500001229034297, 0.000000000000000000, 4.999999999999998224 ) ) ;
#11022 = EDGE_LOOP ( 'NONE', ( #58759, #8169, #40927, #61295 ) ) ;
#11023 = CARTESIAN_POINT ( 'NONE',  ( 14.69062500061451537, -3.027376345333610441, -5.243569643749999898 ) ) ;
#11024 = CARTESIAN_POINT ( 'NONE',  ( 25.38750000122903216, 6.123233995736764310E-16, -4.999999999999998224 ) ) ;
#11025 = CARTESIAN_POINT ( 'NONE',  ( 14.40937500061451715, 4.541064518000418104, -2.621784821874998173 ) ) ;
#11026 = CARTESIAN_POINT ( 'NONE',  ( 5.999957575222543582, 8.000031818581998522, -29.79726394907932274 ) ) ;
#11027 = CARTESIAN_POINT ( 'NONE',  ( 17.69062500061451715, -3.027376345333614438, 5.243569643749998122 ) ) ;
#11028 = CARTESIAN_POINT ( 'NONE',  ( 26.82187500061451857, -6.054752690667223547, -1.112240025338166033E-15 ) ) ;
#11029 = CARTESIAN_POINT ( 'NONE',  ( 4.243569643749999898, 10.99062500061451786, 32.45002607614398471 ) ) ;
#11030 = CARTESIAN_POINT ( 'NONE',  ( 14.82187500061451679, 3.027376345333613106, -5.243569643749998122 ) ) ;
#11031 = CARTESIAN_POINT ( 'NONE',  ( 14.73750000122903359, 4.330127018922191873, 2.499999999999999556 ) ) ;
#11032 = FACE_OUTER_BOUND ( 'NONE', #32808, .T. ) ;
#11033 = DIRECTION ( 'NONE',  ( 0.000000000000000000, 0.000000000000000000, -1.000000000000000000 ) ) ;
#11034 = CARTESIAN_POINT ( 'NONE',  ( 21.57187500061451502, 3.027376345333613106, -5.243569643749998122 ) ) ;
#11035 = CARTESIAN_POINT ( 'NONE',  ( 20.47500000122903074, 2.886751345948129099, -4.999999999999998224 ) ) ;
#11036 = CARTESIAN_POINT ( 'NONE',  ( 17.67187500061451644, 3.027376345333611329, 5.243569643749999010 ) ) ;
#11037 = CARTESIAN_POINT ( 'NONE',  ( -3.000416591977282496E-16, 12.99687500061451750, 25.09994784771203058 ) ) ;
#11038 = CARTESIAN_POINT ( 'NONE',  ( 16.52812500061451573, 6.421520780324663323E-16, -5.243569643749999010 ) ) ;
#11039 = ORIENTED_EDGE ( 'NONE', *, *, #18886, .F. ) ;
#11040 = ORIENTED_EDGE ( 'NONE', *, *, #47637, .F. ) ;
#11041 = CARTESIAN_POINT ( 'NONE',  ( 20.81250000000000000, 2.886751345948129099, -4.999999999999998224 ) ) ;
#11042 = FACE_OUTER_BOUND ( 'NONE', #71756, .T. ) ;
#11043 = CARTESIAN_POINT ( 'NONE',  ( 23.31562500061451715, 3.027376345333613106, -5.243569643749998122 ) ) ;
#11044 = CARTESIAN_POINT ( 'NONE',  ( 3.028125000614518392, 6.421520780324663323E-16, -5.243569643749999010 ) ) ;
#11045 = CARTESIAN_POINT ( 'NONE',  ( 16.91250000122903430, 4.330127018922192761, -2.499999999999997780 ) ) ;
#11046 = CARTESIAN_POINT ( 'NONE',  ( 21.70312500061451644, 0.000000000000000000, 5.243569643749999010 ) ) ;
#11047 = CARTESIAN_POINT ( 'NONE',  ( 25.52812500061451573, 6.421520780324663323E-16, -5.243569643749999010 ) ) ;
#11048 = CARTESIAN_POINT ( 'NONE',  ( 6.178125000614518747, 6.421520780324663323E-16, -5.243569643749999010 ) ) ;
#11049 = ORIENTED_EDGE ( 'NONE', *, *, #7387, .F. ) ;
#11050 = CARTESIAN_POINT ( 'NONE',  ( -1.487416814333745711E-14, 16.96250000000000213, 34.00000000000000000 ) ) ;
#11051 = CARTESIAN_POINT ( 'NONE',  ( 17.17500000000000071, 6.123233995736764310E-16, -4.999999999999998224 ) ) ;
#11052 = CARTESIAN_POINT ( 'NONE',  ( 11.63437500061451857, 5.824947211148865298E-16, -4.756430356249998326 ) ) ;
#11053 = CARTESIAN_POINT ( 'NONE',  ( 12.56250000122903465, 0.000000000000000000, 4.999999999999998224 ) ) ;
#11054 = CARTESIAN_POINT ( 'NONE',  ( -3.999999999999997335, 12.05000000122903536, -27.69059892324149175 ) ) ;
#11055 = CARTESIAN_POINT ( 'NONE',  ( 2.121784821874999061, 18.35937500061451644, -33.67503911421598417 ) ) ;
#11056 = CARTESIAN_POINT ( 'NONE',  ( 8.887499999999999289, -2.886751345948129988, 4.999999999999997335 ) ) ;
#11057 =( BOUNDED_CURVE ( )  B_SPLINE_CURVE ( 2, ( #61575, #67504, #56048, #50867, #32786, #45694, #4717 ),
 .UNSPECIFIED., .F., .F. ) 
 B_SPLINE_CURVE_WITH_KNOTS ( ( 3, 2, 2, 3 ),
 ( 0.1499999999999999944, 0.1533333333333333215, 0.1566666666666666485, 0.1599999999999999756 ),
 .UNSPECIFIED. ) 
 CURVE ( )  GEOMETRIC_REPRESENTATION_ITEM ( )  RATIONAL_B_SPLINE_CURVE ( ( 1.000000000000000000, 0.8660254037844387076, 1.000000000000000000, 0.8660254037844387076, 1.000000000000000000, 0.8660254037844398178, 0.9999999999999988898 ) ) 
 REPRESENTATION_ITEM ( '' )  );
#11058 = ADVANCED_FACE ( 'NONE', ( #11330 ), #38681, .T. ) ;
#11059 = CARTESIAN_POINT ( 'NONE',  ( 4.687500001229034652, 6.123233995736764310E-16, -4.999999999999998224 ) ) ;
#11060 = CARTESIAN_POINT ( 'NONE',  ( 13.20937500061451786, 0.000000000000000000, 5.243569643749999010 ) ) ;
#11061 = CARTESIAN_POINT ( 'NONE',  ( 1.071796769724497445, 16.82990381179670081, -33.99999999999998579 ) ) ;
#11062 = CARTESIAN_POINT ( 'NONE',  ( 4.209375000614516971, 0.000000000000000000, 5.243569643749999010 ) ) ;
#11063 = CARTESIAN_POINT ( 'NONE',  ( 12.15000000000000036, -4.330127018922190985, -2.500000000000001332 ) ) ;
#11064 = CARTESIAN_POINT ( 'NONE',  ( 19.87500000000000000, 6.123233995736764310E-16, -4.999999999999998224 ) ) ;
#11065 = CARTESIAN_POINT ( 'NONE',  ( 9.009375000614518569, 4.541064518000418104, -2.621784821874998173 ) ) ;
#11066 = CARTESIAN_POINT ( 'NONE',  ( 4.000000000000000000, 17.15000000122903145, -27.69059892324149885 ) ) ;
#11067 = CARTESIAN_POINT ( 'NONE',  ( 19.04062500061451146, -3.027376345333614438, 5.243569643749998122 ) ) ;
#11068 = CARTESIAN_POINT ( 'NONE',  ( 4.635370124282374604, -3.449855572172436879, -4.024674870222735734 ) ) ;
#11069 = CARTESIAN_POINT ( 'NONE',  ( 2.121784821875001281, 17.70312500061459104, 33.67503911421598417 ) ) ;
#11070 = CARTESIAN_POINT ( 'NONE',  ( 22.69687500061451857, -3.027376345333614438, 5.243569643749998122 ) ) ;
#11071 = DIRECTION ( 'NONE',  ( -1.000000000000000000, -0.000000000000000000, -0.000000000000000000 ) ) ;
#11072 = CARTESIAN_POINT ( 'NONE',  ( 3.178125000614515638, 4.541064518000418104, 2.621784821874999949 ) ) ;
#11073 = CARTESIAN_POINT ( 'NONE',  ( 19.88437500061451502, -2.746126346562646425, 4.756430356249996549 ) ) ;
#11074 = CARTESIAN_POINT ( 'NONE',  ( 26.24062500061451431, -3.027376345333614438, 5.243569643749998122 ) ) ;
#11075 = CARTESIAN_POINT ( 'NONE',  ( 16.26562500061451289, 3.027376345333611329, 5.243569643749999010 ) ) ;
#11076 = CARTESIAN_POINT ( 'NONE',  ( 13.55625000122903323, -4.330127018922190985, -2.500000000000001332 ) ) ;
#11077 = CARTESIAN_POINT ( 'NONE',  ( 12.27187500061451786, 3.027376345333611329, 5.243569643749999010 ) ) ;
#11078 = CARTESIAN_POINT ( 'NONE',  ( 28.42499999999999716, 6.123233995736764310E-16, -4.999999999999998224 ) ) ;
#11079 = CARTESIAN_POINT ( 'NONE',  ( 24.33750000122903145, -4.330127018922194537, 2.499999999999995559 ) ) ;
#11080 = CARTESIAN_POINT ( 'NONE',  ( 3.759375000614517681, 0.000000000000000000, 5.243569643749999010 ) ) ;
#11081 = CARTESIAN_POINT ( 'NONE',  ( 15.34687500061451537, 6.054752690667223547, 3.707466751127219781E-16 ) ) ;
#11082 = CARTESIAN_POINT ( 'NONE',  ( 29.59687500061451715, -3.027376345333610441, -5.243569643749999898 ) ) ;
#11083 = LINE ( 'NONE', #67610, #28922 ) ;
#11084 = CARTESIAN_POINT ( 'NONE',  ( 15.88125000122903074, 6.123233995736764310E-16, -4.999999999999998224 ) ) ;
#11085 = CARTESIAN_POINT ( 'NONE',  ( 24.15937500061451715, -4.541064518000417216, -2.621784821875001281 ) ) ;
#11086 = CARTESIAN_POINT ( 'NONE',  ( 13.95937500061451786, 4.541064518000418104, -2.621784821874998173 ) ) ;
#11087 = CARTESIAN_POINT ( 'NONE',  ( -3.756430356249999214, 15.19062499938548250, 27.83122392262697531 ) ) ;
#11088 = CARTESIAN_POINT ( 'NONE',  ( 28.16249999999999787, 2.886751345948126879, 4.999999999999999112 ) ) ;
#11089 = CARTESIAN_POINT ( 'NONE',  ( 4.650000001229035895, -2.886751345948125991, -5.000000000000000000 ) ) ;
#11090 = CARTESIAN_POINT ( 'NONE',  ( 5.362500000000003375, -5.773502691896255534, -1.060575238724906372E-15 ) ) ;
#11091 = CARTESIAN_POINT ( 'NONE',  ( 7.734375000614518214, -2.746126346562646425, 4.756430356249996549 ) ) ;
#11092 = CARTESIAN_POINT ( 'NONE',  ( 19.07812500061451644, -4.541064518000419881, 2.621784821874995952 ) ) ;
#11093 = CARTESIAN_POINT ( 'NONE',  ( 9.600000000000001421, 4.330127018922192761, -2.499999999999997780 ) ) ;
#11094 = FACE_OUTER_BOUND ( 'NONE', #25580, .T. ) ;
#11095 = CARTESIAN_POINT ( 'NONE',  ( 16.53750000000000142, -2.886751345948129988, 4.999999999999997335 ) ) ;
#11096 = CARTESIAN_POINT ( 'NONE',  ( 9.001249775931846008E-16, 13.16562500061451857, 34.90005215228797653 ) ) ;
#11097 = CARTESIAN_POINT ( 'NONE',  ( 4.000000000000000000, 18.34999999999999787, 30.00000000000000000 ) ) ;
#11098 = CARTESIAN_POINT ( 'NONE',  ( 19.61250000122903359, 4.330127018922192761, -2.499999999999997780 ) ) ;
#11099 = CARTESIAN_POINT ( 'NONE',  ( 1.587219675395664886, 9.875134926496691889, 35.78969804657884168 ) ) ;
#11100 = CARTESIAN_POINT ( 'NONE',  ( 27.08437500061451786, 4.541064518000418104, 2.621784821874999949 ) ) ;
#11101 = ORIENTED_EDGE ( 'NONE', *, *, #42409, .F. ) ;
#11102 = CARTESIAN_POINT ( 'NONE',  ( 16.45312500061451289, -4.541064518000417216, -2.621784821875001281 ) ) ;
#11103 = CARTESIAN_POINT ( 'NONE',  ( 22.97812500061451857, 4.541064518000418104, 2.621784821874999949 ) ) ;
#11104 = CARTESIAN_POINT ( 'NONE',  ( 23.55937500061451573, 0.000000000000000000, 5.243569643749999010 ) ) ;
#11105 = CARTESIAN_POINT ( 'NONE',  ( 6.412500000000001421, 2.886751345948129099, -4.999999999999998224 ) ) ;
#11106 = CARTESIAN_POINT ( 'NONE',  ( 9.665625000614515017, -6.054752690667223547, -1.112240025338166033E-15 ) ) ;
#11107 = CARTESIAN_POINT ( 'NONE',  ( 25.22812500061451502, 4.541064518000418104, 2.621784821874999949 ) ) ;
#11108 = CARTESIAN_POINT ( 'NONE',  ( 15.34687500061451537, 6.054752690667223547, 3.707466751127219781E-16 ) ) ;
#11109 = CARTESIAN_POINT ( 'NONE',  ( 18.19687500061451502, -3.027376345333614438, 5.243569643749998122 ) ) ;
#11110 = FACE_OUTER_BOUND ( 'NONE', #11288, .T. ) ;
#11111 = CARTESIAN_POINT ( 'NONE',  ( 4.243569643749999898, 17.29062500061451502, 32.45002607614398471 ) ) ;
#11112 = CARTESIAN_POINT ( 'NONE',  ( 22.50000000122903288, -2.886751345948129988, 4.999999999999997335 ) ) ;
#11113 = CARTESIAN_POINT ( 'NONE',  ( 14.03437500061451715, 4.119189519843966529, 2.378215178124999607 ) ) ;
#11114 = CARTESIAN_POINT ( 'NONE',  ( 11.42812500061451608, -4.541064518000419881, 2.621784821874995952 ) ) ;
#11115 = CARTESIAN_POINT ( 'NONE',  ( 6.759375000614516793, 4.541064518000418104, -2.621784821874998173 ) ) ;
#11116 = CARTESIAN_POINT ( 'NONE',  ( 5.446875000614518569, 6.054752690667223547, 3.707466751127219781E-16 ) ) ;
#11117 = VERTEX_POINT ( 'NONE', #26358 ) ;
#11118 = CARTESIAN_POINT ( 'NONE',  ( 28.13437500061451502, -4.541064518000419881, 2.621784821874995952 ) ) ;
#11119 = CARTESIAN_POINT ( 'NONE',  ( 18.17812500061451786, -4.541064518000419881, 2.621784821874995952 ) ) ;
#11120 = CARTESIAN_POINT ( 'NONE',  ( 27.18750000122903288, 6.123233995736764310E-16, -4.999999999999998224 ) ) ;
#11121 =( BOUNDED_CURVE ( )  B_SPLINE_CURVE ( 2, ( #18577, #41143, #45233, #30410, #59193, #7506, #53673 ),
 .UNSPECIFIED., .F., .F. ) 
 B_SPLINE_CURVE_WITH_KNOTS ( ( 3, 2, 2, 3 ),
 ( 0.7416666666666666963, 0.7444444444444444642, 0.7472222222222222321, 0.7500000000000000000 ),
 .UNSPECIFIED. ) 
 CURVE ( )  GEOMETRIC_REPRESENTATION_ITEM ( )  RATIONAL_B_SPLINE_CURVE ( ( 1.000000000000000000, 0.8660254037844387076, 1.000000000000000000, 0.8660254037844387076, 1.000000000000000000, 0.8660254037844387076, 1.000000000000000000 ) ) 
 REPRESENTATION_ITEM ( '' )  );
#11122 = EDGE_CURVE ( 'NONE', #32974, #64445, #71310, .T. ) ;
#11123 = CARTESIAN_POINT ( 'NONE',  ( 28.75312500061451715, 4.541064518000418104, -2.621784821874998173 ) ) ;
#11124 = CARTESIAN_POINT ( 'NONE',  ( 25.20937500061451431, 4.541064518000418104, -2.621784821874998173 ) ) ;
#11125 = CARTESIAN_POINT ( 'NONE',  ( 20.46562500061451928, -6.054752690667223547, -1.112240025338166033E-15 ) ) ;
#11126 = CARTESIAN_POINT ( 'NONE',  ( 4.243569643749999010, 18.77187500061451786, 27.54997392385601174 ) ) ;
#11127 = CARTESIAN_POINT ( 'NONE',  ( 24.70312500061451644, 4.541064518000418104, -2.621784821874998173 ) ) ;
#11128 = CARTESIAN_POINT ( 'NONE',  ( 4.312500001229034652, 4.330127018922192761, -2.499999999999997780 ) ) ;
#11129 = ORIENTED_EDGE ( 'NONE', *, *, #67636, .T. ) ;
#11130 = CARTESIAN_POINT ( 'NONE',  ( 28.91250000000000497, 2.886751345948129099, -4.999999999999998224 ) ) ;
#11131 = CARTESIAN_POINT ( 'NONE',  ( -3.999999999999997335, 14.63750000000000107, -27.69059892324149175 ) ) ;
#11132 = CARTESIAN_POINT ( 'NONE',  ( -3.756430356249999214, 16.99062499938548143, 27.83122392262697531 ) ) ;
#11133 = CARTESIAN_POINT ( 'NONE',  ( 5.184375000614516615, -4.541064518000419881, 2.621784821874995952 ) ) ;
#11134 = CARTESIAN_POINT ( 'NONE',  ( 12.77812500061451750, -4.541064518000419881, 2.621784821874995952 ) ) ;
#11135 = CARTESIAN_POINT ( 'NONE',  ( 6.946875000614517681, -3.027376345333614438, 5.243569643749998122 ) ) ;
#11136 = CARTESIAN_POINT ( 'NONE',  ( 25.23750000122903359, -4.330127018922194537, 2.499999999999995559 ) ) ;
#11137 = CARTESIAN_POINT ( 'NONE',  ( 14.14687500061451786, -3.027376345333614438, 5.243569643749998122 ) ) ;
#11138 = CARTESIAN_POINT ( 'NONE',  ( 3.196875000614516793, 6.054752690667223547, 3.707466751127219781E-16 ) ) ;
#11139 = CARTESIAN_POINT ( 'NONE',  ( 28.64999999999999858, 0.000000000000000000, 4.999999999999998224 ) ) ;
#11140 = CARTESIAN_POINT ( 'NONE',  ( 25.73437500061451644, 4.541064518000418104, 2.621784821874999949 ) ) ;
#11141 = CARTESIAN_POINT ( 'NONE',  ( 14.43749999999999645, -2.886751345948181946, -4.999999999999904077 ) ) ;
#11142 = CARTESIAN_POINT ( 'NONE',  ( 13.82812500061451466, 6.421520780324663323E-16, -5.243569643749999010 ) ) ;
#11143 = VERTEX_POINT ( 'NONE', #38911 ) ;
#11144 = CARTESIAN_POINT ( 'NONE',  ( 10.22812500061451679, 6.421520780324663323E-16, -5.243569643749999010 ) ) ;
#11145 = VECTOR ( 'NONE', #44483, 1000.000000000000000 ) ;
#11146 = CARTESIAN_POINT ( 'NONE',  ( 5.765625000614519102, 3.027376345333613106, -5.243569643749998122 ) ) ;
#11147 = CARTESIAN_POINT ( 'NONE',  ( 18.15937500061451715, 0.000000000000000000, 4.756430356249998326 ) ) ;
#11148 = ADVANCED_FACE ( 'NONE', ( #20804 ), #61430, .T. ) ;
#11149 = LINE ( 'NONE', #40310, #5503 ) ;
#11150 = VECTOR ( 'NONE', #66869, 1000.000000000000000 ) ;
#11151 = CARTESIAN_POINT ( 'NONE',  ( 16.64999999999999858, -4.330127018922190985, -2.500000000000001332 ) ) ;
#11152 = CARTESIAN_POINT ( 'NONE',  ( 14.93437500061451750, 4.541064518000418104, 2.621784821874999949 ) ) ;
#11153 = CARTESIAN_POINT ( 'NONE',  ( 13.65000000122903323, -2.886751345948125991, -5.000000000000000000 ) ) ;
#11154 = CARTESIAN_POINT ( 'NONE',  ( 20.36249999999999716, 2.886751345948129099, -4.999999999999998224 ) ) ;
#11155 = CARTESIAN_POINT ( 'NONE',  ( 21.38437500061451502, -4.541064518000419881, 2.621784821874995952 ) ) ;
#11156 = CARTESIAN_POINT ( 'NONE',  ( -4.243569643749999898, 13.05312500061451786, -30.00000000000000000 ) ) ;
#11157 = VECTOR ( 'NONE', #16685, 1000.000000000000000 ) ;
#11158 = CARTESIAN_POINT ( 'NONE',  ( 1.626862140677534470E-15, 13.68124999877096748, 34.00000000000000000 ) ) ;
#11159 = CARTESIAN_POINT ( 'NONE',  ( 25.39687500061451431, -4.119189519843965641, -2.378215178125001383 ) ) ;
#11160 = CYLINDRICAL_SURFACE ( 'NONE', #65496, 4.999999999999998224 ) ;
#11161 = CARTESIAN_POINT ( 'NONE',  ( 26.24062500061451431, -3.027376345333614438, 5.243569643749998122 ) ) ;
#11162 = CARTESIAN_POINT ( 'NONE',  ( 17.06250000122903288, 0.000000000000000000, 4.999999999999998224 ) ) ;
#11163 = CYLINDRICAL_SURFACE ( 'NONE', #66839, 4.999999999999998224 ) ;
#11164 = EDGE_CURVE ( 'NONE', #64445, #35963, #40243, .T. ) ;
#11165 = CARTESIAN_POINT ( 'NONE',  ( 25.50000000000000000, 0.000000000000000000, 4.999999999999998224 ) ) ;
#11166 = CARTESIAN_POINT ( 'NONE',  ( 8.728125000614518569, -4.541064518000419881, 2.621784821874995952 ) ) ;
#11167 = CARTESIAN_POINT ( 'NONE',  ( 26.89687500061451431, 4.119189519843966529, -2.378215178124998275 ) ) ;
#11168 = CARTESIAN_POINT ( 'NONE',  ( 18.19687500061451502, -3.027376345333614438, 5.243569643749998122 ) ) ;
#11169 = CARTESIAN_POINT ( 'NONE',  ( 12.45937500061451786, 2.746126346562645981, -4.756430356249997438 ) ) ;
#11170 = CARTESIAN_POINT ( 'NONE',  ( 5.540625000614515905, -3.027376345333614438, 5.243569643749998122 ) ) ;
#11171 = CARTESIAN_POINT ( 'NONE',  ( 10.32187500061451679, 3.027376345333613106, -5.243569643749998122 ) ) ;
#11172 = EDGE_LOOP ( 'NONE', ( #27130, #67871, #42453, #57056 ) ) ;
#11173 = CARTESIAN_POINT ( 'NONE',  ( 22.20937500061451431, 0.000000000000000000, 5.243569643749999010 ) ) ;
#11174 = DIRECTION ( 'NONE',  ( 0.000000000000000000, 0.000000000000000000, -1.000000000000000000 ) ) ;
#11175 = CARTESIAN_POINT ( 'NONE',  ( 29.06250000000000000, 2.886751345948126879, 4.999999999999999112 ) ) ;
#11176 = CARTESIAN_POINT ( 'NONE',  ( 5.850000000000001421, -4.330127018922190985, -2.500000000000001332 ) ) ;
#11177 = CARTESIAN_POINT ( 'NONE',  ( 15.48750000122903359, 6.123233995736764310E-16, -4.999999999999998224 ) ) ;
#11178 = CARTESIAN_POINT ( 'NONE',  ( 20.68125000122903145, -4.330127018922194537, 2.499999999999995559 ) ) ;
#11179 = CARTESIAN_POINT ( 'NONE',  ( 19.01249999999999929, 2.886751345948095793, -5.000000000000055067 ) ) ;
#11180 = ORIENTED_EDGE ( 'NONE', *, *, #29228, .T. ) ;
#11181 = CARTESIAN_POINT ( 'NONE',  ( 12.22499999999999964, 6.123233995736764310E-16, -4.999999999999998224 ) ) ;
#11182 = CARTESIAN_POINT ( 'NONE',  ( 25.90312500061451573, -4.541064518000417216, -2.621784821875001281 ) ) ;
#11183 = CARTESIAN_POINT ( 'NONE',  ( 17.28750000000000142, 5.773502691896255534, 3.535250795749688894E-16 ) ) ;
#11184 = CARTESIAN_POINT ( 'NONE',  ( 11.66250000122903430, 0.000000000000000000, 4.999999999999998224 ) ) ;
#11185 = CARTESIAN_POINT ( 'NONE',  ( 9.703125000614514661, -4.541064518000417216, -2.621784821875001281 ) ) ;
#11186 = CARTESIAN_POINT ( 'NONE',  ( 7.875000000000000000, 4.330127018922191873, 2.499999999999999556 ) ) ;
#11187 = CARTESIAN_POINT ( 'NONE',  ( 0.000000000000000000, 27.50000000000000000, 30.00000000000000000 ) ) ;
#11188 = CARTESIAN_POINT ( 'NONE',  ( 9.001249775931846008E-16, 15.47187500061451892, -25.09994784771203058 ) ) ;
#11189 = CARTESIAN_POINT ( 'NONE',  ( 27.11250000122903359, -4.330127018922190985, -2.500000000000001332 ) ) ;
#11190 = CARTESIAN_POINT ( 'NONE',  ( -3.756430356250000102, 14.66562499938548214, 30.00000000000000000 ) ) ;
#11191 = CARTESIAN_POINT ( 'NONE',  ( 7.200000000000001954, -4.330127018922190985, -2.500000000000001332 ) ) ;
#11192 = FACE_OUTER_BOUND ( 'NONE', #2125, .T. ) ;
#11193 = VECTOR ( 'NONE', #13770, 1000.000000000000000 ) ;
#11194 = ORIENTED_EDGE ( 'NONE', *, *, #66354, .T. ) ;
#11195 = CARTESIAN_POINT ( 'NONE',  ( 25.26562500061451289, 3.027376345333611329, 5.243569643749999010 ) ) ;
#11196 = CARTESIAN_POINT ( 'NONE',  ( 29.27812500061451573, 4.541064518000418104, 2.621784821874999949 ) ) ;
#11197 = CARTESIAN_POINT ( 'NONE',  ( 28.88437500061451502, 4.541064518000418104, 2.621784821874999949 ) ) ;
#11198 = CARTESIAN_POINT ( 'NONE',  ( 19.17187500061451999, -6.054752690667223547, -1.112240025338166033E-15 ) ) ;
#11199 = CARTESIAN_POINT ( 'NONE',  ( 16.71562500061451573, 3.027376345333611329, 5.243569643749999010 ) ) ;
#11200 = CARTESIAN_POINT ( 'NONE',  ( 4.243569643749999898, 11.89062500061459282, -27.54997392385601529 ) ) ;
#11201 = CARTESIAN_POINT ( 'NONE',  ( 6.065625000614516260, -6.054752690667223547, -1.112240025338166033E-15 ) ) ;
#11202 = CARTESIAN_POINT ( 'NONE',  ( 27.78750000122903074, 4.330127018922191873, 2.499999999999999556 ) ) ;
#11203 = CARTESIAN_POINT ( 'NONE',  ( 25.02187500061451431, -5.492252693125287522, -1.008910452111647106E-15 ) ) ;
#11204 = CARTESIAN_POINT ( 'NONE',  ( 18.89062500061451644, 6.054752690667223547, 3.707466751127219781E-16 ) ) ;
#11205 = CARTESIAN_POINT ( 'NONE',  ( -1.487416814333745711E-14, 16.06250000000000000, -26.00000000000000000 ) ) ;
#11206 = CARTESIAN_POINT ( 'NONE',  ( -3.756430356250000102, 18.26562499938548356, 30.00000000000000000 ) ) ;
#11207 = CARTESIAN_POINT ( 'NONE',  ( 12.87187500061451750, -6.054752690667223547, -1.112240025338166033E-15 ) ) ;
#11208 = CARTESIAN_POINT ( 'NONE',  ( 11.67187500061451821, 3.027376345333613106, -5.243569643749998122 ) ) ;
#11209 = CARTESIAN_POINT ( 'NONE',  ( 21.49687500061451573, -3.027376345333610441, -5.243569643749999898 ) ) ;
#11210 = ORIENTED_EDGE ( 'NONE', *, *, #55404, .F. ) ;
#11211 = CARTESIAN_POINT ( 'NONE',  ( -1.071796769724496556, 14.80490381179669690, -26.00000000000000355 ) ) ;
#11212 = CARTESIAN_POINT ( 'NONE',  ( 25.64062500061451644, 6.054752690667223547, 3.707466751127219781E-16 ) ) ;
#11213 = VECTOR ( 'NONE', #5183, 1000.000000000000000 ) ;
#11214 = CARTESIAN_POINT ( 'NONE',  ( 27.25312500061451360, -4.541064518000417216, -2.621784821875001281 ) ) ;
#11215 = CARTESIAN_POINT ( 'NONE',  ( 1.999999999999998668, 12.20000000000000107, -33.46410161513775705 ) ) ;
#11216 = CARTESIAN_POINT ( 'NONE',  ( 4.000000000000000000, 17.48750000000000071, 32.30940107675849049 ) ) ;
#11217 = CARTESIAN_POINT ( 'NONE',  ( 4.059375000614519280, 4.541064518000418104, -2.621784821874998173 ) ) ;
#11218 = ITEM_DEFINED_TRANSFORMATION ( 'NONE', 'NONE', #26153,  #23765 ) ;
#11219 = CARTESIAN_POINT ( 'NONE',  ( 12.67500000122903536, -5.773502691896255534, -1.060575238724906372E-15 ) ) ;
#11220 = AXIS2_PLACEMENT_3D ( 'NONE', #19112, #19851, #48312 ) ;
#11221 = CARTESIAN_POINT ( 'NONE',  ( 7.500000001229034652, 5.773502691896255534, 3.535250795749688894E-16 ) ) ;
#11222 = CARTESIAN_POINT ( 'NONE',  ( 29.25000000122903288, -2.886751345948129988, 4.999999999999997335 ) ) ;
#11223 = CARTESIAN_POINT ( 'NONE',  ( -2.000000000000001776, 17.69374999877096855, 33.46410161513775705 ) ) ;
#11224 = CARTESIAN_POINT ( 'NONE',  ( 17.23125000122903572, 6.123233995736764310E-16, -4.999999999999998224 ) ) ;
#11225 = CARTESIAN_POINT ( 'NONE',  ( 12.49687500061451573, -3.027376345333610441, -5.243569643749999898 ) ) ;
#11226 = CARTESIAN_POINT ( 'NONE',  ( -3.137519842735245283E-14, 14.71250000000000213, -26.00000000000000711 ) ) ;
#11227 = EDGE_LOOP ( 'NONE', ( #24614, #39277, #9167, #58690 ) ) ;
#11228 = CARTESIAN_POINT ( 'NONE',  ( 20.80312500061451431, 0.000000000000000000, 5.243569643749999010 ) ) ;
#11229 = CARTESIAN_POINT ( 'NONE',  ( 12.79687500061451821, -3.027376345333614438, 5.243569643749998122 ) ) ;
#11230 = CARTESIAN_POINT ( 'NONE',  ( 4.903125000614516615, 4.541064518000418104, -2.621784821874998173 ) ) ;
#11231 = CARTESIAN_POINT ( 'NONE',  ( 22.20937500061451431, 0.000000000000000000, 5.243569643749999010 ) ) ;
#11232 = CARTESIAN_POINT ( 'NONE',  ( 9.084375000614517859, 4.541064518000418104, 2.621784821874999949 ) ) ;
#11233 = CARTESIAN_POINT ( 'NONE',  ( 5.578125000614518214, -4.541064518000419881, 2.621784821874995952 ) ) ;
#11234 = CARTESIAN_POINT ( 'NONE',  ( 11.66250000122903430, 0.000000000000000000, 4.999999999999998224 ) ) ;
#11236 = EDGE_CURVE ( 'NONE', #63910, #24148, #30330, .T. ) ;
#11235 = CARTESIAN_POINT ( 'NONE',  ( 4.912500001229034297, 0.000000000000000000, 4.999999999999998224 ) ) ;
#11237 = CARTESIAN_POINT ( 'NONE',  ( 20.65312500061451573, 4.541064518000418104, -2.621784821874998173 ) ) ;
#11238 = CARTESIAN_POINT ( 'NONE',  ( 8.587500001229035007, -4.330127018922194537, 2.499999999999995559 ) ) ;
#11239 = CARTESIAN_POINT ( 'NONE',  ( 16.52812500061451573, 6.421520780324663323E-16, -5.243569643749999010 ) ) ;
#11240 = CARTESIAN_POINT ( 'NONE',  ( 14.69062500061451537, -3.027376345333610441, -5.243569643749999898 ) ) ;
#11241 = CARTESIAN_POINT ( 'NONE',  ( 26.14687500061451431, 5.492252693125287522, 3.363034840372157021E-16 ) ) ;
#11242 = CARTESIAN_POINT ( 'NONE',  ( 16.91250000000000142, 2.886751345948126879, 4.999999999999999112 ) ) ;
#11243 = CARTESIAN_POINT ( 'NONE',  ( 9.000000001229034652, -2.886751345948129988, 4.999999999999997335 ) ) ;
#11244 = CARTESIAN_POINT ( 'NONE',  ( 5.503125000614516260, 0.000000000000000000, 5.243569643749999010 ) ) ;
#11245 = CARTESIAN_POINT ( 'NONE',  ( 21.11250000122903359, 0.000000000000000000, 4.999999999999998224 ) ) ;
#11246 = CARTESIAN_POINT ( 'NONE',  ( 26.39999999999999858, 0.000000000000000000, 4.999999999999998224 ) ) ;
#11247 = VECTOR ( 'NONE', #64610, 1000.000000000000000 ) ;
#11248 = CARTESIAN_POINT ( 'NONE',  ( 4.243569643749999898, 10.59687500061451715, -27.54997392385601529 ) ) ;
#11249 = CARTESIAN_POINT ( 'NONE',  ( 0.000000000000000000, 20.00000000000000000, 26.00000000000000000 ) ) ;
#11250 = FACE_OUTER_BOUND ( 'NONE', #62816, .T. ) ;
#11251 = VECTOR ( 'NONE', #71053, 1000.000000000000000 ) ;
#11252 = CARTESIAN_POINT ( 'NONE',  ( 3.000000001229033320, 5.773502691896255534, 3.535250795749688401E-16 ) ) ;
#11253 = CARTESIAN_POINT ( 'NONE',  ( 21.94687500061451857, -3.027376345333610441, -5.243569643749999898 ) ) ;
#11254 = CARTESIAN_POINT ( 'NONE',  ( 5.175000000000002487, 4.330127018922191873, 2.499999999999999556 ) ) ;
#11255 = AXIS2_PLACEMENT_3D ( 'NONE', #6269, #740, #29527 ) ;
#11256 = CARTESIAN_POINT ( 'NONE',  ( 17.61562500061451786, 3.027376345333611329, 5.243569643749999010 ) ) ;
#11257 = CARTESIAN_POINT ( 'NONE',  ( 12.46875000122902932, 2.886751345948126879, 4.999999999999999112 ) ) ;
#11258 = CARTESIAN_POINT ( 'NONE',  ( -3.999999999999999112, 20.73124999877096641, 27.69059892324149530 ) ) ;
#11259 = CARTESIAN_POINT ( 'NONE',  ( 4.520699896614321034, -3.533387626757130029, -3.879993107621428905 ) ) ;
#11260 = CARTESIAN_POINT ( 'NONE',  ( 29.14687500061451075, -3.027376345333610441, -5.243569643749999898 ) ) ;
#11261 = CARTESIAN_POINT ( 'NONE',  ( 19.62187500061451573, 5.824947211148865298E-16, -4.756430356249998326 ) ) ;
#11262 = CARTESIAN_POINT ( 'NONE',  ( 12.62812500061451537, 4.541064518000418104, 2.621784821874999949 ) ) ;
#11263 = CARTESIAN_POINT ( 'NONE',  ( 10.02187500061451964, 3.027376345333611329, 5.243569643749999010 ) ) ;
#11264 = ORIENTED_EDGE ( 'NONE', *, *, #1743, .T. ) ;
#11265 = CARTESIAN_POINT ( 'NONE',  ( 21.96562500061451573, 3.027376345333613106, -5.243569643749998122 ) ) ;
#11266 = CARTESIAN_POINT ( 'NONE',  ( 1.999999999999998668, 11.30000000000000071, -33.46410161513775705 ) ) ;
#11267 = CARTESIAN_POINT ( 'NONE',  ( 1.999999999999998668, 15.46250000122903501, -33.46410161513775705 ) ) ;
#11268 = ADVANCED_FACE ( 'NONE', ( #20433 ), #21169, .F. ) ;
#11269 = CARTESIAN_POINT ( 'NONE',  ( 12.30000000000000249, 4.330127018922192761, -2.499999999999997780 ) ) ;
#11270 = EDGE_CURVE ( 'NONE', #30207, #30864, #49994, .T. ) ;
#11271 = CARTESIAN_POINT ( 'NONE',  ( 22.12500000122903288, -5.773502691896255534, -1.060575238724906372E-15 ) ) ;
#11272 = CARTESIAN_POINT ( 'NONE',  ( 16.19062500061451715, 6.054752690667223547, 3.707466751127219781E-16 ) ) ;
#11273 = CARTESIAN_POINT ( 'NONE',  ( 12.64687500061451786, 0.000000000000000000, 4.756430356249998326 ) ) ;
#11274 = ORIENTED_EDGE ( 'NONE', *, *, #9235, .F. ) ;
#11275 = CARTESIAN_POINT ( 'NONE',  ( 19.01249999999999929, 2.886751345948129099, -4.999999999999998224 ) ) ;
#11276 =( BOUNDED_CURVE ( )  B_SPLINE_CURVE ( 2, ( #71169, #24999, #47542, #64892, #26105, #64525, #14282, #13919, #36457 ),
 .UNSPECIFIED., .F., .F. ) 
 B_SPLINE_CURVE_WITH_KNOTS ( ( 3, 2, 2, 2, 3 ),
 ( 0.4456521739130435145, 0.4492753623188405765, 0.4565217391304347561, 0.4637681159420289911, 0.4673913043478261087 ),
 .UNSPECIFIED. ) 
 CURVE ( )  GEOMETRIC_REPRESENTATION_ITEM ( )  RATIONAL_B_SPLINE_CURVE ( ( 0.9330127018922194093, 0.9330127018922198534, 1.000000000000000000, 0.8660254037844387076, 1.000000000000000000, 0.8660254037844387076, 1.000000000000000000, 0.9330127018922188542, 0.9330127018922194093 ) ) 
 REPRESENTATION_ITEM ( '' )  );
#11277 = CARTESIAN_POINT ( 'NONE',  ( 24.37500000000000000, 6.123233995736764310E-16, -4.999999999999998224 ) ) ;
#11278 = CARTESIAN_POINT ( 'NONE',  ( 22.47187500061451715, 3.027376345333613106, -5.243569643749998122 ) ) ;
#11279 = CARTESIAN_POINT ( 'NONE',  ( 23.99062500061451786, -3.027376345333614438, 5.243569643749998122 ) ) ;
#11280 = ORIENTED_EDGE ( 'NONE', *, *, #72942, .F. ) ;
#11281 = CARTESIAN_POINT ( 'NONE',  ( 19.12500000000000000, 4.330127018922191873, 2.499999999999999556 ) ) ;
#11282 = CARTESIAN_POINT ( 'NONE',  ( 8.578125000614518214, 4.541064518000418104, 2.621784821874999949 ) ) ;
#11283 = DIRECTION ( 'NONE',  ( 0.000000000000000000, 6.195440985631456550E-17, 1.000000000000000000 ) ) ;
#11284 = CARTESIAN_POINT ( 'NONE',  ( 15.33750000000000036, -2.886751345948125991, -5.000000000000000000 ) ) ;
#11285 = CARTESIAN_POINT ( 'NONE',  ( 3.544399568801740674, -3.526694215397601528, -3.727027268090089329 ) ) ;
#11286 = CARTESIAN_POINT ( 'NONE',  ( 4.546875000614517326, 6.054752690667223547, 3.707466751127219781E-16 ) ) ;
#11287 = CARTESIAN_POINT ( 'NONE',  ( 28.39687500061452141, 6.054752690667223547, 3.707466751127219781E-16 ) ) ;
#11288 = EDGE_LOOP ( 'NONE', ( #69382, #49099, #26689, #56894 ) ) ;
#11289 = CARTESIAN_POINT ( 'NONE',  ( 24.62812500061451715, 6.421520780324663323E-16, -5.243569643749999010 ) ) ;
#11290 = CARTESIAN_POINT ( 'NONE',  ( 26.33437500061451431, -4.541064518000419881, 2.621784821874995952 ) ) ;
#11291 = CARTESIAN_POINT ( 'NONE',  ( -4.243569643749999898, 17.96562500061459389, -32.45002607614398471 ) ) ;
#11292 = CARTESIAN_POINT ( 'NONE',  ( 11.13750000000000284, -2.886751345948129988, 4.999999999999997335 ) ) ;
#11293 = CARTESIAN_POINT ( 'NONE',  ( 9.365625000614519635, 3.027376345333613106, -5.243569643749998122 ) ) ;
#11294 = DIRECTION ( 'NONE',  ( -1.000000000000000000, -0.000000000000000000, -0.000000000000000000 ) ) ;
#11295 = CARTESIAN_POINT ( 'NONE',  ( 3.999999999999999112, 19.32500000000000284, -30.00000000000000000 ) ) ;
#11296 = CARTESIAN_POINT ( 'NONE',  ( 25.94062500061451715, -3.027376345333610441, -5.243569643749999898 ) ) ;
#11297 = CARTESIAN_POINT ( 'NONE',  ( 29.67187500061451644, 4.119189519843966529, 2.378215178124999607 ) ) ;
#11298 = CARTESIAN_POINT ( 'NONE',  ( 11.93437500061451573, -4.119189519843968306, 2.378215178124996054 ) ) ;
#11299 = CARTESIAN_POINT ( 'NONE',  ( 3.515625000614516882, 3.027376345333613106, -5.243569643749998122 ) ) ;
#11300 = CARTESIAN_POINT ( 'NONE',  ( 20.37187500061451573, 3.027376345333611329, 5.243569643749999010 ) ) ;
#11301 = CARTESIAN_POINT ( 'NONE',  ( -2.121784821874999949, 15.28437500061451892, 26.32496088578401938 ) ) ;
#11302 = CARTESIAN_POINT ( 'NONE',  ( 20.89687500061452141, -3.027376345333614438, 5.243569643749998122 ) ) ;
#11303 = CARTESIAN_POINT ( 'NONE',  ( 3.562500000000000444, -5.773502691896255534, -1.060575238724906372E-15 ) ) ;
#11304 = CARTESIAN_POINT ( 'NONE',  ( 4.243569643749999898, 18.73437500061451644, 30.00000000000000000 ) ) ;
#11305 = CARTESIAN_POINT ( 'NONE',  ( 9.740625000614516082, -3.027376345333610441, -5.243569643749999898 ) ) ;
#11306 = LINE ( 'NONE', #39020, #13566 ) ;
#11307 = CARTESIAN_POINT ( 'NONE',  ( 5.934375000614517504, 4.541064518000418104, 2.621784821874999949 ) ) ;
#11308 = CARTESIAN_POINT ( 'NONE',  ( 29.15625000122903288, 0.000000000000000000, 4.999999999999998224 ) ) ;
#11309 = CARTESIAN_POINT ( 'NONE',  ( 6.590625000614518392, -3.027376345333610441, -5.243569643749999898 ) ) ;
#11310 = CARTESIAN_POINT ( 'NONE',  ( 12.08437500061451608, 6.421520780324663323E-16, -5.243569643749999010 ) ) ;
#11311 = FILL_AREA_STYLE_COLOUR ( '', #17852 ) ;
#11312 = CARTESIAN_POINT ( 'NONE',  ( 18.26250000122903216, 4.330127018922192761, -2.499999999999997780 ) ) ;
#11313 = CARTESIAN_POINT ( 'NONE',  ( 7.959375000614516971, -4.541064518000417216, -2.621784821875001281 ) ) ;
#11314 = CARTESIAN_POINT ( 'NONE',  ( 9.065625000614517148, 3.027376345333611329, 5.243569643749999010 ) ) ;
#11315 = CARTESIAN_POINT ( 'NONE',  ( 5.165625000614517681, -6.054752690667223547, -1.112240025338166033E-15 ) ) ;
#11316 = CARTESIAN_POINT ( 'NONE',  ( 26.60625000122903216, -4.330127018922190985, -2.500000000000001332 ) ) ;
#11317 = CARTESIAN_POINT ( 'NONE',  ( 19.09687500061451360, -3.027376345333614438, 5.243569643749998122 ) ) ;
#11318 = CARTESIAN_POINT ( 'NONE',  ( 9.187500001229034652, 6.123233995736764310E-16, -4.999999999999998224 ) ) ;
#11319 = CARTESIAN_POINT ( 'NONE',  ( 27.77812500061451573, 6.421520780324663323E-16, -5.243569643749999010 ) ) ;
#11320 = CARTESIAN_POINT ( 'NONE',  ( 10.94062500061451537, -3.027376345333614438, 5.243569643749998122 ) ) ;
#11321 = CARTESIAN_POINT ( 'NONE',  ( 0.000000000000000000, -4.999999999999999112, 0.000000000000000000 ) ) ;
#11322 = CARTESIAN_POINT ( 'NONE',  ( 4.243569643749999898, 11.53437500061451892, -30.00000000000000000 ) ) ;
#11323 = CARTESIAN_POINT ( 'NONE',  ( 12.37500000122903465, 2.886751345948129099, -4.999999999999998224 ) ) ;
#11324 = CARTESIAN_POINT ( 'NONE',  ( 27.47812500061451502, 4.541064518000418104, 2.621784821874999949 ) ) ;
#11325 = VECTOR ( 'NONE', #66975, 1000.000000000000000 ) ;
#11326 = CARTESIAN_POINT ( 'NONE',  ( -2.121784821874996840, 15.37812500061451892, -26.32496088578401583 ) ) ;
#11327 = CARTESIAN_POINT ( 'NONE',  ( 13.98750000122903359, -4.330127018922194537, 2.499999999999995559 ) ) ;
#11328 = AXIS2_PLACEMENT_3D ( 'NONE', #40628, #19522, #46895 ) ;
#11329 = CARTESIAN_POINT ( 'NONE',  ( 12.30000000000000249, 4.330127018922192761, -2.499999999999997780 ) ) ;
#11330 = FACE_OUTER_BOUND ( 'NONE', #35477, .T. ) ;
#11331 = CARTESIAN_POINT ( 'NONE',  ( 23.54062500061451146, -3.027376345333614438, 5.243569643749998122 ) ) ;
#11332 = CARTESIAN_POINT ( 'NONE',  ( 8.521875000614517859, 3.027376345333612662, -5.243569643749998122 ) ) ;
#11333 = CARTESIAN_POINT ( 'NONE',  ( 7.987500001229032698, 4.330127018922191873, 2.499999999999999556 ) ) ;
#11334 = CARTESIAN_POINT ( 'NONE',  ( 15.90000000122903501, -2.886751345948125991, -5.000000000000000000 ) ) ;
#11335 =( BOUNDED_CURVE ( )  B_SPLINE_CURVE ( 2, ( #6703, #440, #58012, #56579, #24038, #29948, #52488, #1899, #46588 ),
 .UNSPECIFIED., .F., .F. ) 
 B_SPLINE_CURVE_WITH_KNOTS ( ( 3, 2, 2, 2, 3 ),
 ( 0.3152173913043478382, 0.3188405797101449002, 0.3260869565217391353, 0.3333333333333333148, 0.3369565217391304324 ),
 .UNSPECIFIED. ) 
 CURVE ( )  GEOMETRIC_REPRESENTATION_ITEM ( )  RATIONAL_B_SPLINE_CURVE ( ( 0.9330127018922194093, 0.9330127018922198534, 1.000000000000000000, 0.8660254037844387076, 1.000000000000000000, 0.8660254037844387076, 1.000000000000000000, 0.9330127018922194093, 0.9330127018922194093 ) ) 
 REPRESENTATION_ITEM ( '' )  );
#11336 = CARTESIAN_POINT ( 'NONE',  ( 12.92812500061451786, 6.421520780324663323E-16, -5.243569643749999010 ) ) ;
#11337 = CARTESIAN_POINT ( 'NONE',  ( 16.49062500061451786, -3.027376345333610441, -5.243569643749999898 ) ) ;
#11338 =( BOUNDED_CURVE ( )  B_SPLINE_CURVE ( 2, ( #7659, #46469, #64167, #24646, #13555, #18368, #2135, #30564, #63083 ),
 .UNSPECIFIED., .F., .F. ) 
 B_SPLINE_CURVE_WITH_KNOTS ( ( 3, 2, 2, 2, 3 ),
 ( 0.03260869565217391908, 0.03623188405797101580, 0.04347826086956521618, 0.05072463768115942351, 0.05434782608695652717 ),
 .UNSPECIFIED. ) 
 CURVE ( )  GEOMETRIC_REPRESENTATION_ITEM ( )  RATIONAL_B_SPLINE_CURVE ( ( 0.9330127018922192983, 0.9330127018922194093, 1.000000000000000000, 0.8660254037844387076, 1.000000000000000000, 0.8660254037844387076, 1.000000000000000000, 0.9330127018922192983, 0.9330127018922194093 ) ) 
 REPRESENTATION_ITEM ( '' )  );
#11339 = CARTESIAN_POINT ( 'NONE',  ( 28.53750000122903074, 6.123233995736764310E-16, -4.999999999999998224 ) ) ;
#11340 = CARTESIAN_POINT ( 'NONE',  ( 22.27499999999999858, 4.330127018922191873, 2.499999999999999556 ) ) ;
#11341 = CARTESIAN_POINT ( 'NONE',  ( 23.63437500061451502, -4.541064518000419881, 2.621784821874995952 ) ) ;
#11342 = CARTESIAN_POINT ( 'NONE',  ( 10.53750000122903252, 6.123233995736764310E-16, -4.999999999999998224 ) ) ;
#11343 = CARTESIAN_POINT ( 'NONE',  ( 28.92187500061451644, 3.027376345333611329, 5.243569643749999010 ) ) ;
#11344 =( BOUNDED_CURVE ( )  B_SPLINE_CURVE ( 2, ( #19326, #19696, #18962, #53698, #8266, #52966, #47066 ),
 .UNSPECIFIED., .F., .F. ) 
 B_SPLINE_CURVE_WITH_KNOTS ( ( 3, 2, 2, 3 ),
 ( 0.8699999999999999956, 0.8733333333333332948, 0.8766666666666667052, 0.8800000000000000044 ),
 .UNSPECIFIED. ) 
 CURVE ( )  GEOMETRIC_REPRESENTATION_ITEM ( )  RATIONAL_B_SPLINE_CURVE ( ( 1.000000000000000000, 0.8660254037844387076, 1.000000000000000000, 0.8660254037844387076, 1.000000000000000000, 0.8660254037844387076, 1.000000000000000000 ) ) 
 REPRESENTATION_ITEM ( '' )  );
#11345 = CARTESIAN_POINT ( 'NONE',  ( 4.659375000614518925, 0.000000000000000000, 5.243569643749999010 ) ) ;
#11346 = CARTESIAN_POINT ( 'NONE',  ( 22.67812500061451431, -4.541064518000419881, 2.621784821874995952 ) ) ;
#11347 = CARTESIAN_POINT ( 'NONE',  ( -1.878215178125001827, 14.85312499938548214, 33.25316411605952283 ) ) ;
#11348 = CARTESIAN_POINT ( 'NONE',  ( 7.050000000000000711, 0.000000000000000000, 4.999999999999998224 ) ) ;
#11349 = CARTESIAN_POINT ( 'NONE',  ( 11.29687500061451644, 6.054752690667223547, 3.707466751127219781E-16 ) ) ;
#11350 = CARTESIAN_POINT ( 'NONE',  ( 3.384375000614517237, -4.541064518000419881, 2.621784821874995952 ) ) ;
#11351 = CARTESIAN_POINT ( 'NONE',  ( 7.021875000614518747, -6.054752690667223547, -1.112240025338166033E-15 ) ) ;
#11352 = CARTESIAN_POINT ( 'NONE',  ( 25.94999999999999929, 0.000000000000000000, 4.999999999999998224 ) ) ;
#11353 = CARTESIAN_POINT ( 'NONE',  ( 28.43437500061451573, 4.541064518000418104, 2.621784821874999949 ) ) ;
#11354 = CARTESIAN_POINT ( 'NONE',  ( 27.76875000122903359, 2.886751345948119774, 5.000000000000010658 ) ) ;
#11355 = CARTESIAN_POINT ( 'NONE',  ( 19.94999999999999929, 4.330127018922192761, -2.499999999999997780 ) ) ;
#11356 = ORIENTED_EDGE ( 'NONE', *, *, #40217, .T. ) ;
#11357 = CARTESIAN_POINT ( 'NONE',  ( 26.02499999999999858, -4.330127018922194537, 2.499999999999995559 ) ) ;
#11358 = CARTESIAN_POINT ( 'NONE',  ( 28.84687500061452070, 6.054752690667223547, 3.707466751127219781E-16 ) ) ;
#11359 = VERTEX_POINT ( 'NONE', #15263 ) ;
#11360 = CARTESIAN_POINT ( 'NONE',  ( 14.54062500061451679, -3.027376345333614438, 5.243569643749998122 ) ) ;
#11361 = CARTESIAN_POINT ( 'NONE',  ( 8.953125000614518214, 4.541064518000418104, -2.621784821874998173 ) ) ;
#11362 = CARTESIAN_POINT ( 'NONE',  ( 19.50937500061451857, -5.492252693125287522, -1.008910452111647106E-15 ) ) ;
#11363 = CARTESIAN_POINT ( 'NONE',  ( 4.321875000614517681, -6.054752690667223547, -1.112240025338166033E-15 ) ) ;
#11364 = CARTESIAN_POINT ( 'NONE',  ( 17.36250000122903359, 4.330127018922192761, -2.499999999999997780 ) ) ;
#11365 = CARTESIAN_POINT ( 'NONE',  ( 21.56250000000000000, -5.773502691896255534, -1.060575238724906372E-15 ) ) ;
#11366 = DIRECTION ( 'NONE',  ( -1.000000000000000000, -0.000000000000000000, -0.000000000000000000 ) ) ;
#11367 = CARTESIAN_POINT ( 'NONE',  ( 6.946875000614517681, -3.027376345333614438, 5.243569643749998122 ) ) ;
#11368 = CARTESIAN_POINT ( 'NONE',  ( 10.69687500061451679, -3.027376345333610441, -5.243569643749999898 ) ) ;
#11369 = CARTESIAN_POINT ( 'NONE',  ( 22.09687500061451715, 6.054752690667223547, 3.707466751127219781E-16 ) ) ;
#11370 = VERTEX_POINT ( 'NONE', #32265 ) ;
#11371 = CARTESIAN_POINT ( 'NONE',  ( 3.984375000614517326, 6.421520780324663323E-16, -5.243569643749999010 ) ) ;
#11372 = CARTESIAN_POINT ( 'NONE',  ( 6.759375000614516793, 4.541064518000418104, -2.621784821874998173 ) ) ;
#11373 = CARTESIAN_POINT ( 'NONE',  ( 18.26249999999999929, 2.886751345948126879, 4.999999999999999112 ) ) ;
#11374 = CARTESIAN_POINT ( 'NONE',  ( 16.52812500061451573, 6.421520780324663323E-16, -5.243569643749999010 ) ) ;
#11375 = CARTESIAN_POINT ( 'NONE',  ( 2.828200636599751609E-16, 18.46249999999999858, 25.38119784648299415 ) ) ;
#11376 = CARTESIAN_POINT ( 'NONE',  ( 45.00000000000000000, 0.000000000000000000, 0.000000000000000000 ) ) ;
#11377 = CARTESIAN_POINT ( 'NONE',  ( 22.84687500061451715, -2.746126346562642428, -4.756430356249999214 ) ) ;
#11378 = CARTESIAN_POINT ( 'NONE',  ( 9.515625000614518214, 3.027376345333611329, 5.243569643749999010 ) ) ;
#11379 = CARTESIAN_POINT ( 'NONE',  ( 26.74687500061451573, -3.027376345333614438, 5.243569643749998122 ) ) ;
#11380 = CARTESIAN_POINT ( 'NONE',  ( 20.32499999999999929, 6.123233995736764310E-16, -4.999999999999998224 ) ) ;
#11381 = CARTESIAN_POINT ( 'NONE',  ( 29.25937500061451502, 4.541064518000418104, -2.621784821874998173 ) ) ;
#11382 = CARTESIAN_POINT ( 'NONE',  ( 10.83750000000000036, -2.886751345948125991, -5.000000000000000000 ) ) ;
#11383 = CARTESIAN_POINT ( 'NONE',  ( 1.999999999999998668, 14.56250000122903288, 26.53589838486224650 ) ) ;
#11384 = CARTESIAN_POINT ( 'NONE',  ( 9.712500001229033231, 4.330127018922192761, -2.499999999999997780 ) ) ;
#11385 = CARTESIAN_POINT ( 'NONE',  ( 19.50937500061451857, 0.000000000000000000, 5.243569643749999010 ) ) ;
#11386 = CARTESIAN_POINT ( 'NONE',  ( 15.00937500061451679, 0.000000000000000000, 5.243569643749999010 ) ) ;
#11387 = CARTESIAN_POINT ( 'NONE',  ( -3.183805653906651933, 3.859810113929996067, -32.43433874829330676 ) ) ;
#11388 = VERTEX_POINT ( 'NONE', #65513 ) ;
#11389 = CARTESIAN_POINT ( 'NONE',  ( 13.71562500061451750, -6.054752690667223547, -1.112240025338166033E-15 ) ) ;
#11390 = CARTESIAN_POINT ( 'NONE',  ( 25.16250000122903074, 0.000000000000000000, 4.999999999999998224 ) ) ;
#11391 = CARTESIAN_POINT ( 'NONE',  ( 14.97187500061451892, 3.027376345333611329, 5.243569643749999010 ) ) ;
#11392 = CARTESIAN_POINT ( 'NONE',  ( 5.191822204397932516, 8.550203871005534140, -33.03186005587161134 ) ) ;
#11393 = CARTESIAN_POINT ( 'NONE',  ( 18.14062500061451644, -3.027376345333614438, 5.243569643749998122 ) ) ;
#11394 = CARTESIAN_POINT ( 'NONE',  ( 45.00000000000000000, 6.123233995736764310E-16, -4.999999999999998224 ) ) ;
#11395 = CARTESIAN_POINT ( 'NONE',  ( 25.54687500061451644, -3.027376345333610441, -5.243569643749999898 ) ) ;
#11396 = CARTESIAN_POINT ( 'NONE',  ( 4.243569643749999010, 11.06562500061451715, 27.54997392385601174 ) ) ;
#11397 = ADVANCED_FACE ( 'NONE', ( #60688 ), #66245, .F. ) ;
#11398 = CARTESIAN_POINT ( 'NONE',  ( 15.64687500061451608, -3.027376345333610441, -5.243569643749999898 ) ) ;
#11399 = CARTESIAN_POINT ( 'NONE',  ( 14.06250000122903288, -4.330127018922190985, -2.500000000000001332 ) ) ;
#11400 = CARTESIAN_POINT ( 'NONE',  ( 8.221875000614518925, 2.746126346562643317, 4.756430356249998326 ) ) ;
#11401 = CARTESIAN_POINT ( 'NONE',  ( 9.001249775931846008E-16, 19.07187500061451857, -25.09994784771203058 ) ) ;
#11402 = CARTESIAN_POINT ( 'NONE',  ( 17.03437500061451715, 6.421520780324663323E-16, -5.243569643749999010 ) ) ;
#11403 = CARTESIAN_POINT ( 'NONE',  ( 20.13750000122903216, 4.330127018922191873, 2.499999999999999556 ) ) ;
#11404 = EDGE_CURVE ( 'NONE', #25148, #8380, #72157, .T. ) ;
#11405 = CARTESIAN_POINT ( 'NONE',  ( 15.34687500061451537, 6.054752690667223547, 3.707466751127219781E-16 ) ) ;
#11406 = CARTESIAN_POINT ( 'NONE',  ( -4.243569643749997233, 13.14687500061451786, 32.45002607614398471 ) ) ;
#11407 = CARTESIAN_POINT ( 'NONE',  ( 22.98750000122903003, -4.330127018922194537, 2.499999999999995559 ) ) ;
#11408 = VECTOR ( 'NONE', #49139, 1000.000000000000000 ) ;
#11409 = CARTESIAN_POINT ( 'NONE',  ( 15.10312500061451502, -4.541064518000417216, -2.621784821875001281 ) ) ;
#11410 = CARTESIAN_POINT ( 'NONE',  ( 29.27812500061451573, 4.541064518000418104, 2.621784821874999949 ) ) ;
#11411 = ORIENTED_EDGE ( 'NONE', *, *, #49257, .T. ) ;
#11412 = ORIENTED_EDGE ( 'NONE', *, *, #64823, .F. ) ;
#11413 = CARTESIAN_POINT ( 'NONE',  ( 21.67500000000000071, 6.123233995736764310E-16, -4.999999999999998224 ) ) ;
#11414 = LINE ( 'NONE', #39125, #38547 ) ;
#11415 = CARTESIAN_POINT ( 'NONE',  ( 3.065625000614517592, 3.027376345333613106, -5.243569643749998122 ) ) ;
#11416 = CARTESIAN_POINT ( 'NONE',  ( 14.13750000122903394, 6.123233995736764310E-16, -4.999999999999998224 ) ) ;
#11417 = CARTESIAN_POINT ( 'NONE',  ( 18.92812500061451431, 4.541064518000418104, 2.621784821874999949 ) ) ;
#11418 = CARTESIAN_POINT ( 'NONE',  ( 24.44062500061451715, -3.027376345333614438, 5.243569643749998122 ) ) ;
#11419 = CARTESIAN_POINT ( 'NONE',  ( 6.853125000614516793, 0.000000000000000000, 5.243569643749999010 ) ) ;
#11420 = CARTESIAN_POINT ( 'NONE',  ( 5.810221930991193690E-16, 20.20624999877096428, 26.00000000000000000 ) ) ;
#11421 = CARTESIAN_POINT ( 'NONE',  ( 3.365625000614516082, -6.054752690667223547, -1.112240025338166033E-15 ) ) ;
#11422 = CARTESIAN_POINT ( 'NONE',  ( 9.571875000614518569, 2.746126346562643317, 4.756430356249998326 ) ) ;
#11423 = CARTESIAN_POINT ( 'NONE',  ( 45.00000000000000000, 0.000000000000000000, 0.000000000000000000 ) ) ;
#11424 = CARTESIAN_POINT ( 'NONE',  ( 8.484601909799253346E-16, 10.77500000122903501, -25.38119784648299770 ) ) ;
#11425 = CARTESIAN_POINT ( 'NONE',  ( 4.243569643749999898, 17.38437500061451502, -30.00000000000000000 ) ) ;
#11426 = CARTESIAN_POINT ( 'NONE',  ( 5.400000001229032343, -2.886751345948129988, 4.999999999999997335 ) ) ;
#11427 = CARTESIAN_POINT ( 'NONE',  ( 8.287499999999999645, 5.773502691896255534, 3.535250795749688894E-16 ) ) ;
#11428 = CARTESIAN_POINT ( 'NONE',  ( 5.250000001229035540, 5.773502691896255534, 3.535250795749688894E-16 ) ) ;
#11429 = CARTESIAN_POINT ( 'NONE',  ( 12.42187500061451821, -6.054752690667223547, -1.112240025338166033E-15 ) ) ;
#11430 = CARTESIAN_POINT ( 'NONE',  ( 19.42500000122903714, -5.773502691896255534, -1.060575238724906372E-15 ) ) ;
#11431 = CARTESIAN_POINT ( 'NONE',  ( 3.639202574798650947, 4.093918037350785966, 3.396265244785773074 ) ) ;
#11432 = CARTESIAN_POINT ( 'NONE',  ( 12.86250000122903359, 4.330127018922192761, -2.499999999999997780 ) ) ;
#11433 = CARTESIAN_POINT ( 'NONE',  ( 9.600000000000001421, 4.330127018922192761, -2.499999999999997780 ) ) ;
#11434 = CARTESIAN_POINT ( 'NONE',  ( 11.22187500061451892, 3.027376345333613106, -5.243569643749998122 ) ) ;
#11435 = CARTESIAN_POINT ( 'NONE',  ( 17.51250000122903216, 0.000000000000000000, 4.999999999999998224 ) ) ;
#11436 = AXIS2_PLACEMENT_3D ( 'NONE', #24316, #1808, #30953 ) ;
#11437 = DIRECTION ( 'NONE',  ( -1.000000000000000000, -0.000000000000000000, -0.000000000000000000 ) ) ;
#11438 = CARTESIAN_POINT ( 'NONE',  ( -2.121784821874996840, 16.72812500061459673, 33.67503911421598417 ) ) ;
#11439 = CARTESIAN_POINT ( 'NONE',  ( 21.87187500061451573, -6.054752690667223547, -1.112240025338166033E-15 ) ) ;
#11440 = DIRECTION ( 'NONE',  ( -0.000000000000000000, -1.000000000000000000, -0.000000000000000000 ) ) ;
#11441 = CARTESIAN_POINT ( 'NONE',  ( 28.50000000122903288, -2.886751345948125991, -5.000000000000000000 ) ) ;
#11442 = CARTESIAN_POINT ( 'NONE',  ( 17.33437500061451431, -2.746126346562642428, -4.756430356249999214 ) ) ;
#11443 = CARTESIAN_POINT ( 'NONE',  ( 23.35312500061451857, 4.541064518000418104, -2.621784821874998173 ) ) ;
#11444 = CARTESIAN_POINT ( 'NONE',  ( 16.04062500061451857, -3.027376345333610441, -5.243569643749999898 ) ) ;
#11445 = CARTESIAN_POINT ( 'NONE',  ( 13.06875000122903252, -5.773502691896255534, -1.060575238724906372E-15 ) ) ;
#11446 = CARTESIAN_POINT ( 'NONE',  ( 12.87187500061451750, -6.054752690667223547, -1.112240025338166033E-15 ) ) ;
#11447 = CARTESIAN_POINT ( 'NONE',  ( 29.17500000000000071, -4.330127018922194537, 2.499999999999995559 ) ) ;
#11448 = CARTESIAN_POINT ( 'NONE',  ( 26.13750000122903216, -4.330127018922194537, 2.499999999999995559 ) ) ;
#11449 = CARTESIAN_POINT ( 'NONE',  ( 3.459375000614519635, -4.541064518000417216, -2.621784821875001281 ) ) ;
#11450 = CARTESIAN_POINT ( 'NONE',  ( 15.00937500061451679, 0.000000000000000000, 5.243569643749999010 ) ) ;
#11451 = CARTESIAN_POINT ( 'NONE',  ( 28.88437500061451502, 4.541064518000418104, 2.621784821874999949 ) ) ;
#11452 = CARTESIAN_POINT ( 'NONE',  ( 15.76875000122903181, -5.773502691896255534, -1.060575238724906372E-15 ) ) ;
#11453 = CARTESIAN_POINT ( 'NONE',  ( 21.23437500061451644, 4.541064518000418104, 2.621784821874999949 ) ) ;
#11454 = CARTESIAN_POINT ( 'NONE',  ( 13.88437500061451679, 6.421520780324663323E-16, -5.243569643749999010 ) ) ;
#11455 = CARTESIAN_POINT ( 'NONE',  ( -3.756430356250001434, 15.26562499938548356, 32.16877607737301048 ) ) ;
#11456 = CARTESIAN_POINT ( 'NONE',  ( 28.83749999999999858, -2.886751345948125991, -5.000000000000000000 ) ) ;
#11457 = CARTESIAN_POINT ( 'NONE',  ( 3.937500001229034208, 4.330127018922191873, 2.499999999999999556 ) ) ;
#11458 = CARTESIAN_POINT ( 'NONE',  ( 29.18437500061451573, 5.824947211148865298E-16, -4.756430356249998326 ) ) ;
#11459 = CARTESIAN_POINT ( 'NONE',  ( 16.56562500061451715, 3.027376345333613106, -5.243569643749998122 ) ) ;
#11460 = CARTESIAN_POINT ( 'NONE',  ( 7.912499999999999645, 2.886751345948126879, 4.999999999999999112 ) ) ;
#11461 = CARTESIAN_POINT ( 'NONE',  ( 34.99999999999999289, -4.500000000000000000, -5.500000000000000000 ) ) ;
#11462 = CARTESIAN_POINT ( 'NONE',  ( 17.77499999999999858, 4.330127018922191873, 2.499999999999999556 ) ) ;
#11463 = CARTESIAN_POINT ( 'NONE',  ( -3.000416591977282496E-16, 12.94062500061451537, 25.09994784771203058 ) ) ;
#11464 = CARTESIAN_POINT ( 'NONE',  ( 30.00000000000000000, 0.000000000000000000, 4.999999999999998224 ) ) ;
#11465 = CARTESIAN_POINT ( 'NONE',  ( 19.91250000122903074, -4.330127018922190985, -2.500000000000001332 ) ) ;
#11466 = CARTESIAN_POINT ( 'NONE',  ( 10.65000000000000036, 0.000000000000000000, 4.999999999999998224 ) ) ;
#11467 = CARTESIAN_POINT ( 'NONE',  ( 26.37187500061451217, -6.054752690667223547, -1.112240025338166033E-15 ) ) ;
#11468 = VERTEX_POINT ( 'NONE', #55172 ) ;
#11469 = CARTESIAN_POINT ( 'NONE',  ( 22.34062500061451573, -3.027376345333610441, -5.243569643749999898 ) ) ;
#11470 = CARTESIAN_POINT ( 'NONE',  ( 21.75937500061451502, 0.000000000000000000, 5.243569643749999010 ) ) ;
#11471 = CARTESIAN_POINT ( 'NONE',  ( 6.675000000000000711, -4.330127018922194537, 2.499999999999995559 ) ) ;
#11472 = CARTESIAN_POINT ( 'NONE',  ( 10.64062500061451644, -3.027376345333610441, -5.243569643749999898 ) ) ;
#11473 = CARTESIAN_POINT ( 'NONE',  ( 24.66562500061451502, 3.027376345333613106, -5.243569643749998122 ) ) ;
#11474 = CARTESIAN_POINT ( 'NONE',  ( 14.33437500061451786, 6.421520780324663323E-16, -5.243569643749999010 ) ) ;
#11475 = CARTESIAN_POINT ( 'NONE',  ( 16.58437500061451786, 6.421520780324663323E-16, -5.243569643749999010 ) ) ;
#11476 = CARTESIAN_POINT ( 'NONE',  ( 4.416509438036825941, 2.344049510472278719, -4.690477066236870662 ) ) ;
#11477 = CARTESIAN_POINT ( 'NONE',  ( -2.121784821874996840, 16.72812500061451857, 33.67503911421598417 ) ) ;
#11478 = CARTESIAN_POINT ( 'NONE',  ( 20.32500000122903572, -5.773502691896255534, -1.060575238724906372E-15 ) ) ;
#11479 = CARTESIAN_POINT ( 'NONE',  ( 13.77187500061451786, -5.492252693125287522, -1.008910452111647106E-15 ) ) ;
#11480 = CARTESIAN_POINT ( 'NONE',  ( 12.74062500061451786, -3.027376345333614438, 5.243569643749998122 ) ) ;
#11481 = CARTESIAN_POINT ( 'NONE',  ( 6.271875000614517859, 3.027376345333613106, -5.243569643749998122 ) ) ;
#11482 = CARTESIAN_POINT ( 'NONE',  ( 5.821875000614519458, 3.027376345333613106, -5.243569643749998122 ) ) ;
#11483 = ORIENTED_EDGE ( 'NONE', *, *, #41079, .T. ) ;
#11484 = CARTESIAN_POINT ( 'NONE',  ( 25.88437500061451502, -4.541064518000419881, 2.621784821874995952 ) ) ;
#11485 = CARTESIAN_POINT ( 'NONE',  ( 17.05312500061451786, 4.541064518000418104, -2.621784821874998173 ) ) ;
#11486 = CARTESIAN_POINT ( 'NONE',  ( 27.71250000122903145, 4.330127018922192761, -2.499999999999997780 ) ) ;
#11487 = EDGE_CURVE ( 'NONE', #54979, #24521, #70011, .T. ) ;
#11488 = CARTESIAN_POINT ( 'NONE',  ( 27.29062500061451502, -3.027376345333610441, -5.243569643749999898 ) ) ;
#11489 = CARTESIAN_POINT ( 'NONE',  ( 21.68437500061451573, 4.541064518000418104, 2.621784821874999949 ) ) ;
#11490 = CARTESIAN_POINT ( 'NONE',  ( 16.37812500061451715, -4.541064518000419881, 2.621784821874995952 ) ) ;
#11491 = CARTESIAN_POINT ( 'NONE',  ( 2.000000000000001332, 10.70000000000000107, 33.46410161513774995 ) ) ;
#11492 = CARTESIAN_POINT ( 'NONE',  ( 23.95312500061451289, 0.000000000000000000, 5.243569643749999010 ) ) ;
#11493 = CARTESIAN_POINT ( 'NONE',  ( 5.775000001229033231, 2.886751345948126879, 4.999999999999999112 ) ) ;
#11494 = VERTEX_POINT ( 'NONE', #37441 ) ;
#11495 = CARTESIAN_POINT ( 'NONE',  ( 28.19999999999999929, 0.000000000000000000, 4.999999999999998224 ) ) ;
#11496 = CARTESIAN_POINT ( 'NONE',  ( -1.999999999999997113, 14.22500000000000142, -26.53589838486224295 ) ) ;
#11497 = CARTESIAN_POINT ( 'NONE',  ( -3.756430356250000102, 17.02812499938548285, 30.00000000000000000 ) ) ;
#11498 = CARTESIAN_POINT ( 'NONE',  ( 28.60312500061451502, -4.541064518000417216, -2.621784821875001281 ) ) ;
#11499 = CARTESIAN_POINT ( 'NONE',  ( 9.553125000614517859, 0.000000000000000000, 5.243569643749999010 ) ) ;
#11500 = CARTESIAN_POINT ( 'NONE',  ( 24.00000000122902932, -2.886751345948125991, -5.000000000000000000 ) ) ;
#11501 = CARTESIAN_POINT ( 'NONE',  ( 12.79687500061451821, -3.027376345333614438, 5.243569643749998122 ) ) ;
#11502 = CARTESIAN_POINT ( 'NONE',  ( 29.27812500061451573, 4.541064518000418104, 2.621784821874999949 ) ) ;
#11503 = CARTESIAN_POINT ( 'NONE',  ( 28.72500000000000142, -4.330127018922194537, 2.499999999999995559 ) ) ;
#11504 = CARTESIAN_POINT ( 'NONE',  ( 4.003125000614518925, 4.541064518000418104, -2.621784821874998173 ) ) ;
#11505 = CARTESIAN_POINT ( 'NONE',  ( 14.05312500061451431, 0.000000000000000000, 5.243569643749999010 ) ) ;
#11506 = ORIENTED_EDGE ( 'NONE', *, *, #17845, .T. ) ;
#11507 = CARTESIAN_POINT ( 'NONE',  ( 9.553125000614517859, 0.000000000000000000, 5.243569643749999010 ) ) ;
#11508 = CARTESIAN_POINT ( 'NONE',  ( 4.940625000614515372, 6.054752690667223547, 3.707466751127219781E-16 ) ) ;
#11509 = CARTESIAN_POINT ( 'NONE',  ( 19.13437500061451857, -4.119189519843968306, 2.378215178124996054 ) ) ;
#11510 = CARTESIAN_POINT ( 'NONE',  ( 14.75625000122903252, 0.000000000000000000, 4.999999999999998224 ) ) ;
#11511 = CARTESIAN_POINT ( 'NONE',  ( 16.42500000000000071, 4.330127018922191873, 2.499999999999999556 ) ) ;
#11512 = CARTESIAN_POINT ( 'NONE',  ( 16.58437500061451786, 6.421520780324663323E-16, -5.243569643749999010 ) ) ;
#11513 = CARTESIAN_POINT ( 'NONE',  ( 11.81250000122903465, -4.330127018922190985, -2.500000000000001332 ) ) ;
#11514 = CARTESIAN_POINT ( 'NONE',  ( 18.90937500061451360, 4.541064518000418104, -2.621784821874998173 ) ) ;
#11515 = CARTESIAN_POINT ( 'NONE',  ( 20.92500000000000071, 4.330127018922191873, 2.499999999999999556 ) ) ;
#11516 = CARTESIAN_POINT ( 'NONE',  ( 20.03437500061451715, -4.541064518000419881, 2.621784821874995952 ) ) ;
#11517 = CARTESIAN_POINT ( 'NONE',  ( 4.243569643749999898, 14.14062500061451644, -27.54997392385601529 ) ) ;
#11518 = CARTESIAN_POINT ( 'NONE',  ( 21.03750000122903074, 4.330127018922191873, 2.499999999999999556 ) ) ;
#11519 = CARTESIAN_POINT ( 'NONE',  ( 25.92187500061451644, 5.824947211148865298E-16, -4.756430356249998326 ) ) ;
#11520 = CYLINDRICAL_SURFACE ( 'NONE', #57210, 4.999999999999998224 ) ;
#11521 = CARTESIAN_POINT ( 'NONE',  ( 26.65312500061451573, 0.000000000000000000, 5.243569643749999010 ) ) ;
#11522 = CARTESIAN_POINT ( 'NONE',  ( 17.28750000122903430, 6.123233995736764310E-16, -4.999999999999998224 ) ) ;
#11523 = CARTESIAN_POINT ( 'NONE',  ( 27.27187500061451431, -6.054752690667223547, -1.112240025338166033E-15 ) ) ;
#11524 = CARTESIAN_POINT ( 'NONE',  ( 23.85000000000000142, -4.330127018922190985, -2.500000000000001332 ) ) ;
#11525 = EDGE_CURVE ( 'NONE', #65099, #18895, #50189, .T. ) ;
#11526 = CARTESIAN_POINT ( 'NONE',  ( 8.165625000614516793, 3.027376345333611329, 5.243569643749999010 ) ) ;
#11527 = CARTESIAN_POINT ( 'NONE',  ( 24.30937500061451573, 2.746126346562643317, 4.756430356249998326 ) ) ;
#11528 = CARTESIAN_POINT ( 'NONE',  ( 18.00937500061451502, 4.541064518000418104, -2.621784821874998173 ) ) ;
#11529 = CARTESIAN_POINT ( 'NONE',  ( 12.00937500061451502, 2.746126346562645981, -4.756430356249997438 ) ) ;
#11530 = ADVANCED_FACE ( 'NONE', ( #17081 ), #46896, .T. ) ;
#11531 = CARTESIAN_POINT ( 'NONE',  ( 4.078125000614517326, 4.541064518000418104, 2.621784821874999949 ) ) ;
#11532 = CARTESIAN_POINT ( 'NONE',  ( 11.29687500061451644, 6.054752690667223547, 3.707466751127219781E-16 ) ) ;
#11533 = VERTEX_POINT ( 'NONE', #13256 ) ;
#11534 = CARTESIAN_POINT ( 'NONE',  ( 20.40937500061451715, 0.000000000000000000, 5.243569643749999010 ) ) ;
#11535 = CARTESIAN_POINT ( 'NONE',  ( -4.000000000000000000, 15.81874999877096499, 30.00000000000000000 ) ) ;
#11536 = CARTESIAN_POINT ( 'NONE',  ( 29.28749999999999787, -2.886751345948125991, -5.000000000000000000 ) ) ;
#11537 = CARTESIAN_POINT ( 'NONE',  ( 3.037500000000002309, -2.886751345948129988, 4.999999999999997335 ) ) ;
#11538 = VECTOR ( 'NONE', #13168, 1000.000000000000000 ) ;
#11539 = CARTESIAN_POINT ( 'NONE',  ( 14.06250000122903288, -4.330127018922190985, -2.500000000000001332 ) ) ;
#11540 = CARTESIAN_POINT ( 'NONE',  ( 11.60625000122903216, 0.000000000000000000, 4.999999999999998224 ) ) ;
#11541 = CARTESIAN_POINT ( 'NONE',  ( 14.47500000122903430, -5.773502691896255534, -1.060575238724906372E-15 ) ) ;
#11542 = ORIENTED_EDGE ( 'NONE', *, *, #43393, .T. ) ;
#11543 = APPLICATION_CONTEXT ( 'automotive_design' ) ;
#11544 = CARTESIAN_POINT ( 'NONE',  ( 11.84999999999999964, 4.330127018922192761, -2.499999999999997780 ) ) ;
#11545 = CARTESIAN_POINT ( 'NONE',  ( 25.11562500061451431, 3.027376345333613106, -5.243569643749998122 ) ) ;
#11546 = CARTESIAN_POINT ( 'NONE',  ( 15.03749999999999964, 5.773502691896255534, 3.535250795749688894E-16 ) ) ;
#11547 = EDGE_CURVE ( 'NONE', #64545, #69242, #17443, .T. ) ;
#11548 = CARTESIAN_POINT ( 'NONE',  ( 9.637500001229033941, 6.123233995736764310E-16, -4.999999999999998224 ) ) ;
#11549 = CARTESIAN_POINT ( 'NONE',  ( 8.915625000614515017, 3.027376345333613106, -5.243569643749998122 ) ) ;
#11550 =( BOUNDED_CURVE ( )  B_SPLINE_CURVE ( 2, ( #46506, #6982, #14333, #30601, #58294, #41332, #64942, #69044, #42421 ),
 .UNSPECIFIED., .F., .F. ) 
 B_SPLINE_CURVE_WITH_KNOTS ( ( 3, 2, 2, 2, 3 ),
 ( 0.1847826086956521896, 0.1884057971014492794, 0.1956521739130434867, 0.2028985507246376940, 0.2065217391304347838 ),
 .UNSPECIFIED. ) 
 CURVE ( )  GEOMETRIC_REPRESENTATION_ITEM ( )  RATIONAL_B_SPLINE_CURVE ( ( 0.9330127018922194093, 0.9330127018922196314, 1.000000000000000000, 0.8660254037844387076, 1.000000000000000000, 0.8660254037844387076, 1.000000000000000000, 0.9330127018922194093, 0.9330127018922194093 ) ) 
 REPRESENTATION_ITEM ( '' )  );
#11551 = CARTESIAN_POINT ( 'NONE',  ( 8.212500000000000355, 2.886751345948129099, -4.999999999999998224 ) ) ;
#11552 = CARTESIAN_POINT ( 'NONE',  ( 65.00000000000000000, 0.000000000000000000, 0.000000000000000000 ) ) ;
#11553 = CARTESIAN_POINT ( 'NONE',  ( 4.243569643749999898, 13.74687500061451750, -27.54997392385601529 ) ) ;
#11554 = CARTESIAN_POINT ( 'NONE',  ( 28.68750000122903288, 4.330127018922191873, 2.499999999999999556 ) ) ;
#11555 = CARTESIAN_POINT ( 'NONE',  ( 3.756430356250000546, 16.72812499938548569, 27.83122392262697886 ) ) ;
#11556 = CARTESIAN_POINT ( 'NONE',  ( 8.062500000000000000, -5.773502691896255534, -1.060575238724906372E-15 ) ) ;
#11557 = CARTESIAN_POINT ( 'NONE',  ( -1.071796769724491005, 12.70759618943233349, 26.00000000000000355 ) ) ;
#11558 = EDGE_LOOP ( 'NONE', ( #14162, #22645, #29640, #11714 ) ) ;
#11559 = CARTESIAN_POINT ( 'NONE',  ( 22.26562500061451644, -6.054752690667223547, -1.112240025338166033E-15 ) ) ;
#11560 = CARTESIAN_POINT ( 'NONE',  ( 14.96250000122903323, -4.330127018922190985, -2.500000000000001332 ) ) ;
#11561 = CARTESIAN_POINT ( 'NONE',  ( 3.289418471268391819, -3.765642822148987712, -3.324553038165963148 ) ) ;
#11562 = LINE ( 'NONE', #479, #21911 ) ;
#11563 = CARTESIAN_POINT ( 'NONE',  ( 20.14687500061451786, -3.027376345333610441, -5.243569643749999898 ) ) ;
#11564 = EDGE_CURVE ( 'NONE', #19922, #42983, #25119, .T. ) ;
#11565 = CARTESIAN_POINT ( 'NONE',  ( 17.16562500061451502, 3.027376345333611329, 5.243569643749999010 ) ) ;
#11566 = CARTESIAN_POINT ( 'NONE',  ( 9.001249775931846008E-16, 11.36562500061459424, -25.09994784771203058 ) ) ;
#11567 = CARTESIAN_POINT ( 'NONE',  ( 7.790625000614518569, -3.027376345333614438, 5.243569643749998122 ) ) ;
#11568 = CARTESIAN_POINT ( 'NONE',  ( 28.46250000122903145, -4.330127018922190985, -2.500000000000001332 ) ) ;
#11569 = CARTESIAN_POINT ( 'NONE',  ( 20.93437500061451573, -4.119189519843968306, 2.378215178124996054 ) ) ;
#11570 = CARTESIAN_POINT ( 'NONE',  ( 18.59062500061451573, -3.027376345333614438, 5.243569643749998122 ) ) ;
#11571 = CARTESIAN_POINT ( 'NONE',  ( 25.03125000122903288, 4.330127018922191873, 2.499999999999999556 ) ) ;
#11572 = CARTESIAN_POINT ( 'NONE',  ( 4.200000001229033053, -2.886751345948125991, -5.000000000000000000 ) ) ;
#11573 = CARTESIAN_POINT ( 'NONE',  ( 13.58437500061451786, 4.541064518000418104, 2.621784821874999949 ) ) ;
#11574 = CARTESIAN_POINT ( 'NONE',  ( 12.75937500061451857, 0.000000000000000000, 5.243569643749999010 ) ) ;
#11575 = CARTESIAN_POINT ( 'NONE',  ( 20.29687500061451644, 6.054752690667223547, 3.707466751127219781E-16 ) ) ;
#11576 = ORIENTED_EDGE ( 'NONE', *, *, #41629, .F. ) ;
#11577 = CARTESIAN_POINT ( 'NONE',  ( 3.140625000614516882, 6.054752690667223547, 3.707466751127219781E-16 ) ) ;
#11578 = CARTESIAN_POINT ( 'NONE',  ( 24.06562500061451715, -6.054752690667223547, -1.112240025338166033E-15 ) ) ;
#11579 = CARTESIAN_POINT ( 'NONE',  ( 23.61562500061451431, -6.054752690667223547, -1.112240025338166033E-15 ) ) ;
#11580 = DIRECTION ( 'NONE',  ( 0.000000000000000000, 0.000000000000000000, 1.000000000000000000 ) ) ;
#11581 = CARTESIAN_POINT ( 'NONE',  ( -3.999999999999997335, 16.43750000000000000, 32.30940107675850470 ) ) ;
#11582 = CARTESIAN_POINT ( 'NONE',  ( 4.359375000614517326, -4.541064518000417216, -2.621784821875001281 ) ) ;
#11583 = CARTESIAN_POINT ( 'NONE',  ( 11.70000000122903216, -2.886751345948129988, 4.999999999999997335 ) ) ;
#11584 = CARTESIAN_POINT ( 'NONE',  ( 7.012500001229035718, 4.330127018922192761, -2.499999999999997780 ) ) ;
#11585 = CARTESIAN_POINT ( 'NONE',  ( 21.56250000122903288, 0.000000000000000000, 4.999999999999998224 ) ) ;
#11586 = CARTESIAN_POINT ( 'NONE',  ( 27.07500000122903216, -5.773502691896255534, -1.060575238724906372E-15 ) ) ;
#11587 = CARTESIAN_POINT ( 'NONE',  ( 1.999999999999997335, 18.21874999877096712, 33.46410161513775705 ) ) ;
#11588 = CARTESIAN_POINT ( 'NONE',  ( 15.84375000122903465, -2.886751345948125991, -5.000000000000000000 ) ) ;
#11589 = CARTESIAN_POINT ( 'NONE',  ( 11.55937500061451928, -4.541064518000417216, -2.621784821875001281 ) ) ;
#11590 = CARTESIAN_POINT ( 'NONE',  ( 5.810221930991193690E-16, 17.50624999877096499, 26.00000000000000000 ) ) ;
#11591 = CARTESIAN_POINT ( 'NONE',  ( 18.25312500061451715, -4.541064518000417216, -2.621784821875001281 ) ) ;
#11592 = CARTESIAN_POINT ( 'NONE',  ( 13.24687500061451750, -3.027376345333614438, 5.243569643749998122 ) ) ;
#11593 = CARTESIAN_POINT ( 'NONE',  ( 4.228125000614517681, -4.541064518000419881, 2.621784821874995952 ) ) ;
#11594 = CARTESIAN_POINT ( 'NONE',  ( 21.68437500061451573, 4.541064518000418104, 2.621784821874999949 ) ) ;
#11595 = CARTESIAN_POINT ( 'NONE',  ( 9.009375000614518569, 4.541064518000418104, -2.621784821874998173 ) ) ;
#11596 = CARTESIAN_POINT ( 'NONE',  ( 5.128125000614516260, -4.541064518000419881, 2.621784821874995952 ) ) ;
#11597 = CARTESIAN_POINT ( 'NONE',  ( -2.672702088255949472E-15, 13.90624999877096890, 26.00000000000000000 ) ) ;
#11598 = CARTESIAN_POINT ( 'NONE',  ( 5.100000001229034297, -2.886751345948125991, -5.000000000000000000 ) ) ;
#11599 = CARTESIAN_POINT ( 'NONE',  ( 19.79062500061451502, 6.054752690667223547, 3.707466751127219781E-16 ) ) ;
#11600 = CARTESIAN_POINT ( 'NONE',  ( 6.937500001229033764, 6.123233995736764310E-16, -4.999999999999998224 ) ) ;
#11601 = CARTESIAN_POINT ( 'NONE',  ( 17.16562500061451502, 3.027376345333611329, 5.243569643749999010 ) ) ;
#11602 = CARTESIAN_POINT ( 'NONE',  ( 14.05312500061451431, 0.000000000000000000, 5.243569643749999010 ) ) ;
#11603 = CARTESIAN_POINT ( 'NONE',  ( 26.55937500061451573, 4.119189519843966529, -2.378215178124998275 ) ) ;
#11604 = CARTESIAN_POINT ( 'NONE',  ( 14.13750000000000107, 5.773502691896255534, 3.535250795749688894E-16 ) ) ;
#11605 = CARTESIAN_POINT ( 'NONE',  ( 9.825000001229033941, 2.886751345948126879, 4.999999999999999112 ) ) ;
#11606 = CARTESIAN_POINT ( 'NONE',  ( 5.690625000614516260, -3.027376345333610441, -5.243569643749999898 ) ) ;
#11607 = CARTESIAN_POINT ( 'NONE',  ( 18.90000000122902790, -2.886751345948129988, 4.999999999999997335 ) ) ;
#11608 = CARTESIAN_POINT ( 'NONE',  ( 26.02499999999999858, -4.330127018922194537, 2.499999999999995559 ) ) ;
#11609 = CARTESIAN_POINT ( 'NONE',  ( 2.121784821874999061, 11.60937500061451821, -33.67503911421598417 ) ) ;
#11610 = CARTESIAN_POINT ( 'NONE',  ( 4.588602605000858148, -1.986133463133878285, 4.773510639627289720 ) ) ;
#11611 = CARTESIAN_POINT ( 'NONE',  ( 3.600000001229033408, -2.886751345948129988, 4.999999999999997335 ) ) ;
#11612 = CARTESIAN_POINT ( 'NONE',  ( 28.46250000122903145, -4.330127018922190985, -2.500000000000001332 ) ) ;
#11613 = CARTESIAN_POINT ( 'NONE',  ( 20.14687500061451786, -3.027376345333610441, -5.243569643749999898 ) ) ;
#11614 = CARTESIAN_POINT ( 'NONE',  ( 23.00625000122903430, -4.330127018922190985, -2.500000000000001332 ) ) ;
#11615 = ADVANCED_FACE ( 'NONE', ( #11192 ), #34437, .F. ) ;
#11616 = CARTESIAN_POINT ( 'NONE',  ( 15.92812500061451608, -4.541064518000419881, 2.621784821874995952 ) ) ;
#11617 = CARTESIAN_POINT ( 'NONE',  ( 11.68125000122903145, -4.330127018922194537, 2.499999999999995559 ) ) ;
#11618 = CARTESIAN_POINT ( 'NONE',  ( -1.071796769724496556, 14.80490381179669690, 33.99999999999998579 ) ) ;
#11619 = CARTESIAN_POINT ( 'NONE',  ( 24.43125000122903145, 6.123233995736764310E-16, -4.999999999999998224 ) ) ;
#11620 = CARTESIAN_POINT ( 'NONE',  ( 25.47187500061451715, -6.054752690667223547, -1.112240025338166033E-15 ) ) ;
#11621 = CARTESIAN_POINT ( 'NONE',  ( 18.94687500061451857, 0.000000000000000000, 4.756430356249998326 ) ) ;
#11622 = CARTESIAN_POINT ( 'NONE',  ( 11.65312500061451573, 4.541064518000418104, -2.621784821874998173 ) ) ;
#11623 = CARTESIAN_POINT ( 'NONE',  ( 9.646875000614516082, -3.027376345333614438, 5.243569643749998122 ) ) ;
#11624 = VERTEX_POINT ( 'NONE', #1840 ) ;
#11625 = CARTESIAN_POINT ( 'NONE',  ( 29.80312500061451431, 0.000000000000000000, 5.243569643749999010 ) ) ;
#11626 = CARTESIAN_POINT ( 'NONE',  ( 21.51562500061451644, 3.027376345333613106, -5.243569643749998122 ) ) ;
#11627 = CARTESIAN_POINT ( 'NONE',  ( 22.91250000122903430, 0.000000000000000000, 4.999999999999998224 ) ) ;
#11628 = EDGE_CURVE ( 'NONE', #57370, #53683, #56965, .T. ) ;
#11629 = CARTESIAN_POINT ( 'NONE',  ( 10.89375000122903003, -2.886751345948181946, -4.999999999999904077 ) ) ;
#11630 = CARTESIAN_POINT ( 'NONE',  ( 11.13750000000000284, -2.886751345948129988, 4.999999999999997335 ) ) ;
#11631 = CARTESIAN_POINT ( 'NONE',  ( 21.60000000122903430, -2.886751345948129988, 4.999999999999997335 ) ) ;
#11632 = CARTESIAN_POINT ( 'NONE',  ( 16.15312500061451573, 4.541064518000418104, -2.621784821874998173 ) ) ;
#11633 = CARTESIAN_POINT ( 'NONE',  ( 13.39687500061451431, 4.119189519843966529, -2.378215178124998275 ) ) ;
#11634 = VERTEX_POINT ( 'NONE', #35794 ) ;
#11635 = CARTESIAN_POINT ( 'NONE',  ( 21.18749999999999645, -2.886751345948125991, -5.000000000000000000 ) ) ;
#11636 = ADVANCED_FACE ( 'NONE', ( #45178 ), #41356, .T. ) ;
#11637 = CARTESIAN_POINT ( 'NONE',  ( 24.75000000000000000, -4.330127018922190985, -2.500000000000001332 ) ) ;
#11638 = CARTESIAN_POINT ( 'NONE',  ( 21.38437500061451502, -4.541064518000419881, 2.621784821874995952 ) ) ;
#11639 = CARTESIAN_POINT ( 'NONE',  ( 24.89062500061451644, -3.027376345333614438, 5.243569643749998122 ) ) ;
#11640 = ORIENTED_EDGE ( 'NONE', *, *, #34544, .T. ) ;
#11641 = CARTESIAN_POINT ( 'NONE',  ( 1.071796769724491227, 19.34240381056766722, 26.00000000000000000 ) ) ;
#11642 = CARTESIAN_POINT ( 'NONE',  ( 9.328125000614518214, 6.421520780324663323E-16, -5.243569643749999010 ) ) ;
#11643 = CARTESIAN_POINT ( 'NONE',  ( 10.95000000000000107, 4.330127018922192761, -2.499999999999997780 ) ) ;
#11644 = CARTESIAN_POINT ( 'NONE',  ( 15.75000000000000000, -4.330127018922190985, -2.500000000000001332 ) ) ;
#11645 = CARTESIAN_POINT ( 'NONE',  ( 4.243569643749999898, 17.77812500061451928, 30.00000000000000000 ) ) ;
#11646 = CARTESIAN_POINT ( 'NONE',  ( 4.659375000614518925, 0.000000000000000000, 5.243569643749999010 ) ) ;
#11647 = CARTESIAN_POINT ( 'NONE',  ( 27.23437500061451644, -4.541064518000419881, 2.621784821874995952 ) ) ;
#11648 = ORIENTED_EDGE ( 'NONE', *, *, #44780, .F. ) ;
#11649 = CARTESIAN_POINT ( 'NONE',  ( 23.05312500061451431, 0.000000000000000000, 5.243569643749999010 ) ) ;
#11650 = CARTESIAN_POINT ( 'NONE',  ( 25.35937500061451644, 0.000000000000000000, 5.243569643749999010 ) ) ;
#11651 = CARTESIAN_POINT ( 'NONE',  ( -4.243569643749999898, 18.41562500061459318, -32.45002607614398471 ) ) ;
#11652 = CARTESIAN_POINT ( 'NONE',  ( 12.30000000000000249, 4.330127018922192761, -2.499999999999997780 ) ) ;
#11653 = CARTESIAN_POINT ( 'NONE',  ( 8.353125000614518569, -4.541064518000417216, -2.621784821875001281 ) ) ;
#11654 = CARTESIAN_POINT ( 'NONE',  ( 29.10937500061451644, -4.119189519843965641, -2.378215178125001383 ) ) ;
#11655 = CARTESIAN_POINT ( 'NONE',  ( 28.45312500061451289, 0.000000000000000000, 5.243569643749999010 ) ) ;
#11656 = CARTESIAN_POINT ( 'NONE',  ( 25.71562500061451573, 3.027376345333611329, 5.243569643749999010 ) ) ;
#11657 = CARTESIAN_POINT ( 'NONE',  ( 12.60000000122903430, -2.886751345948130876, 4.999999999999996447 ) ) ;
#11658 = CARTESIAN_POINT ( 'NONE',  ( 13.77187500061451786, -5.492252693125287522, -1.008910452111647106E-15 ) ) ;
#11659 = CARTESIAN_POINT ( 'NONE',  ( 20.67187500061451289, 3.027376345333613106, -5.243569643749998122 ) ) ;
#11660 = CARTESIAN_POINT ( 'NONE',  ( -4.243569643749999898, 14.00937500061451857, 30.00000000000000000 ) ) ;
#11661 = CARTESIAN_POINT ( 'NONE',  ( 18.79687500061451644, -3.027376345333610441, -5.243569643749999898 ) ) ;
#11662 = CARTESIAN_POINT ( 'NONE',  ( 29.18437500061451573, 6.421520780324663323E-16, -5.243569643749999010 ) ) ;
#11663 = CARTESIAN_POINT ( 'NONE',  ( -2.121784821874999949, 16.63437500061451857, 26.32496088578401938 ) ) ;
#11664 = CARTESIAN_POINT ( 'NONE',  ( 10.37812500061451715, 4.541064518000418104, 2.621784821874999949 ) ) ;
#11665 = CARTESIAN_POINT ( 'NONE',  ( 0.000000000000000000, 20.00000000000000000, 24.00000000000000000 ) ) ;
#11666 = CARTESIAN_POINT ( 'NONE',  ( 3.946875000614517681, -3.027376345333610441, -5.243569643749999898 ) ) ;
#11667 = CARTESIAN_POINT ( 'NONE',  ( -3.999999999999999112, 16.06250000122903288, -30.00000000000000000 ) ) ;
#11668 = CARTESIAN_POINT ( 'NONE',  ( 7.190625000614518036, 6.054752690667223547, 3.707466751127219781E-16 ) ) ;
#11669 = CARTESIAN_POINT ( 'NONE',  ( 11.07187500061451679, -6.054752690667223547, -1.112240025338166033E-15 ) ) ;
#11670 = CARTESIAN_POINT ( 'NONE',  ( 18.33750000122903501, 4.330127018922191873, 2.499999999999999556 ) ) ;
#11671 = CARTESIAN_POINT ( 'NONE',  ( 4.996875000614516615, 6.054752690667223547, 3.707466751127219781E-16 ) ) ;
#11672 = B_SPLINE_CURVE_WITH_KNOTS ( 'NONE', 3,
 ( #46051, #17947, #64106, #1712, #18671, #24948, #19030, #40509, #23503, #13491 ),
 .UNSPECIFIED., .F., .F.,
 ( 4, 3, 3, 4 ),
 ( 0.000000000000000000, 0.0001572268757737857144, 0.0003144538226509923230, 0.0005227749235523226640 ),
 .UNSPECIFIED. ) ;
#11673 = CARTESIAN_POINT ( 'NONE',  ( 8.840625000614515727, -3.027376345333610441, -5.243569643749999898 ) ) ;
#11674 = CARTESIAN_POINT ( 'NONE',  ( 5.878125000614517148, 4.541064518000418104, 2.621784821874999949 ) ) ;
#11675 = CARTESIAN_POINT ( 'NONE',  ( 23.94375000122903074, -2.886751345948125991, -5.000000000000000000 ) ) ;
#11676 = CARTESIAN_POINT ( 'NONE',  ( 19.99687500061451573, -3.027376345333614438, 5.243569643749998122 ) ) ;
#11677 = CARTESIAN_POINT ( 'NONE',  ( 9.150000001229033231, -2.886751345948126435, -5.000000000000000000 ) ) ;
#11678 = ORIENTED_EDGE ( 'NONE', *, *, #56574, .F. ) ;
#11679 = CARTESIAN_POINT ( 'NONE',  ( 26.65312500061451573, 0.000000000000000000, 5.243569643749999010 ) ) ;
#11680 = CARTESIAN_POINT ( 'NONE',  ( 12.66562500061451502, 3.027376345333611329, 5.243569643749999010 ) ) ;
#11681 = EDGE_CURVE ( 'NONE', #25555, #19407, #39276, .T. ) ;
#11682 = CARTESIAN_POINT ( 'NONE',  ( 28.39687500061451431, 6.054752690667223547, 3.707466751127219781E-16 ) ) ;
#11683 = CARTESIAN_POINT ( 'NONE',  ( 13.11562500061451786, 3.027376345333611329, 5.243569643749999010 ) ) ;
#11684 = CARTESIAN_POINT ( 'NONE',  ( 2.121784821875001281, 10.55937500061451750, -26.32496088578401938 ) ) ;
#11685 = CARTESIAN_POINT ( 'NONE',  ( 12.48750000122903359, 4.330127018922191873, 2.499999999999999556 ) ) ;
#11686 = CARTESIAN_POINT ( 'NONE',  ( 26.42812500061451431, 6.421520780324663323E-16, -5.243569643749999010 ) ) ;
#11687 = CARTESIAN_POINT ( 'NONE',  ( -2.121784821874999949, 12.52812500061451573, -33.67503911421598417 ) ) ;
#11688 = CARTESIAN_POINT ( 'NONE',  ( 15.82500000122903216, -5.773502691896255534, -1.060575238724906372E-15 ) ) ;
#11689 = CARTESIAN_POINT ( 'NONE',  ( 14.55000000000000071, 4.330127018922192761, -2.499999999999997780 ) ) ;
#11690 = CARTESIAN_POINT ( 'NONE',  ( 20.76562500061451644, 3.027376345333611329, 5.243569643749999010 ) ) ;
#11691 = CARTESIAN_POINT ( 'NONE',  ( 6.759375000614516793, 4.541064518000418104, -2.621784821874998173 ) ) ;
#11692 = CARTESIAN_POINT ( 'NONE',  ( 8.662500001229034297, -4.330127018922190985, -2.500000000000001332 ) ) ;
#11693 = CARTESIAN_POINT ( 'NONE',  ( 15.63750000122903216, 4.330127018922191873, 2.499999999999999556 ) ) ;
#11694 = CARTESIAN_POINT ( 'NONE',  ( 11.84062500061451750, -3.027376345333614438, 5.243569643749998122 ) ) ;
#11695 = CARTESIAN_POINT ( 'NONE',  ( 16.60312500061451857, 4.541064518000418104, -2.621784821874998173 ) ) ;
#11696 = CARTESIAN_POINT ( 'NONE',  ( 26.96250000122903145, 0.000000000000000000, 4.999999999999998224 ) ) ;
#11697 = CARTESIAN_POINT ( 'NONE',  ( 22.50000000000000000, -4.330127018922190985, -2.500000000000001332 ) ) ;
#11698 = CARTESIAN_POINT ( 'NONE',  ( 24.19687500061451857, -3.027376345333610441, -5.243569643749999898 ) ) ;
#11699 = CARTESIAN_POINT ( 'NONE',  ( 45.00000000000000000, 6.123233995736764310E-16, -4.999999999999998224 ) ) ;
#11700 = CARTESIAN_POINT ( 'NONE',  ( 10.72500000122903252, 2.886751345948126879, 4.999999999999999112 ) ) ;
#11701 = CARTESIAN_POINT ( 'NONE',  ( 27.60937500061451644, 0.000000000000000000, 5.243569643749999010 ) ) ;
#11702 =( BOUNDED_CURVE ( )  B_SPLINE_CURVE ( 2, ( #48376, #8842, #31747, #26202, #46642, #1585, #70903 ),
 .UNSPECIFIED., .F., .F. ) 
 B_SPLINE_CURVE_WITH_KNOTS ( ( 3, 2, 2, 3 ),
 ( 0.7333333333333332815, 0.7361111111111111605, 0.7388888888888889284, 0.7416666666666666963 ),
 .UNSPECIFIED. ) 
 CURVE ( )  GEOMETRIC_REPRESENTATION_ITEM ( )  RATIONAL_B_SPLINE_CURVE ( ( 1.000000000000000000, 0.8660254037844387076, 1.000000000000000000, 0.8660254037844387076, 1.000000000000000000, 0.8660254037844387076, 1.000000000000000000 ) ) 
 REPRESENTATION_ITEM ( '' )  );
#11703 = CARTESIAN_POINT ( 'NONE',  ( 5.559375000614517504, 0.000000000000000000, 5.243569643749999010 ) ) ;
#11704 = CARTESIAN_POINT ( 'NONE',  ( 22.71562500061451573, -6.054752690667223547, -1.112240025338166033E-15 ) ) ;
#11705 = CARTESIAN_POINT ( 'NONE',  ( 3.756430356249998770, 15.86562499938548321, 32.16877607737301759 ) ) ;
#11706 = CARTESIAN_POINT ( 'NONE',  ( 1.626862140677534273E-15, 10.77500000122903323, 34.00000000000000000 ) ) ;
#11707 = CARTESIAN_POINT ( 'NONE',  ( 11.07187500061451679, -6.054752690667223547, -1.112240025338166033E-15 ) ) ;
#11708 = CARTESIAN_POINT ( 'NONE',  ( 15.86249999999999893, 2.886751345948129099, -4.999999999999997335 ) ) ;
#11709 = CARTESIAN_POINT ( 'NONE',  ( 29.01562500061451644, -6.054752690667223547, -1.112240025338166033E-15 ) ) ;
#11710 = CARTESIAN_POINT ( 'NONE',  ( 7.059375000614518392, -4.541064518000417216, -2.621784821875001281 ) ) ;
#11711 = CARTESIAN_POINT ( 'NONE',  ( 26.85937500061451644, -4.541064518000417216, -2.621784821875001281 ) ) ;
#11712 = CARTESIAN_POINT ( 'NONE',  ( -2.121784821874999949, 10.27812500061459566, 26.32496088578401938 ) ) ;
#11713 = CARTESIAN_POINT ( 'NONE',  ( 20.24999999999999645, -4.330127018922190985, -2.500000000000001332 ) ) ;
#11714 = ORIENTED_EDGE ( 'NONE', *, *, #2386, .F. ) ;
#11715 = CARTESIAN_POINT ( 'NONE',  ( 28.04999999999999716, 4.330127018922192761, -2.499999999999997780 ) ) ;
#11716 = EDGE_CURVE ( 'NONE', #38366, #36659, #52795, .T. ) ;
#11717 = CARTESIAN_POINT ( 'NONE',  ( 29.33437500061451431, 4.541064518000418104, 2.621784821874999949 ) ) ;
#11718 = VERTEX_POINT ( 'NONE', #24711 ) ;
#11719 = CARTESIAN_POINT ( 'NONE',  ( 15.47812500061451679, -4.541064518000419881, 2.621784821874995952 ) ) ;
#11720 = CARTESIAN_POINT ( 'NONE',  ( 8.840625000614515727, -3.027376345333610441, -5.243569643749999898 ) ) ;
#11721 = CARTESIAN_POINT ( 'NONE',  ( 18.68437500061451573, -2.746126346562642428, -4.756430356249999214 ) ) ;
#11722 = CARTESIAN_POINT ( 'NONE',  ( 4.696875000614518569, -3.027376345333614438, 5.243569643749998122 ) ) ;
#11723 = CARTESIAN_POINT ( 'NONE',  ( 17.85000000122903430, 5.773502691896255534, 3.535250795749688894E-16 ) ) ;
#11724 = CARTESIAN_POINT ( 'NONE',  ( 22.12500000000000000, 6.123233995736764310E-16, -4.999999999999998224 ) ) ;
#11725 = CARTESIAN_POINT ( 'NONE',  ( 45.00000000000000000, 6.123233995736764310E-16, -4.999999999999998224 ) ) ;
#11726 = CARTESIAN_POINT ( 'NONE',  ( 5.259375000614518569, -4.541064518000417216, -2.621784821875001281 ) ) ;
#11727 = CARTESIAN_POINT ( 'NONE',  ( 11.07187500061451679, -6.054752690667223547, -1.112240025338166033E-15 ) ) ;
#11728 = CARTESIAN_POINT ( 'NONE',  ( 22.39687500061451075, -3.027376345333610441, -5.243569643749999898 ) ) ;
#11729 = CARTESIAN_POINT ( 'NONE',  ( -3.999999999999997335, 17.33749999999999858, -27.69059892324149530 ) ) ;
#11730 = ORIENTED_EDGE ( 'NONE', *, *, #39611, .F. ) ;
#11731 = CARTESIAN_POINT ( 'NONE',  ( 3.796875000614517326, -3.027376345333614438, 5.243569643749998122 ) ) ;
#11732 = CARTESIAN_POINT ( 'NONE',  ( 8.221875000614518925, 3.027376345333611329, 5.243569643749999010 ) ) ;
#11733 = CARTESIAN_POINT ( 'NONE',  ( 18.30000000000000071, 0.000000000000000000, 4.999999999999998224 ) ) ;
#11734 = CARTESIAN_POINT ( 'NONE',  ( 16.67812500061451786, 4.541064518000418104, 2.621784821874999949 ) ) ;
#11735 = CARTESIAN_POINT ( 'NONE',  ( -8.484601909799255319E-16, 16.43750000000000000, 34.61880215351700940 ) ) ;
#11736 = CARTESIAN_POINT ( 'NONE',  ( 24.75000000122903288, -2.886751345948130876, 4.999999999999996447 ) ) ;
#11737 = CARTESIAN_POINT ( 'NONE',  ( 19.13437500061451857, -4.119189519843968306, 2.378215178124996054 ) ) ;
#11738 = CARTESIAN_POINT ( 'NONE',  ( 10.37812500061451715, 4.541064518000418104, 2.621784821874999949 ) ) ;
#11739 = CARTESIAN_POINT ( 'NONE',  ( 25.77187500061451075, 3.027376345333611329, 5.243569643749999010 ) ) ;
#11740 = CARTESIAN_POINT ( 'NONE',  ( 4.898587196589411843E-16, 20.00000000000000000, -26.00000000000000000 ) ) ;
#11741 = CARTESIAN_POINT ( 'NONE',  ( 27.42187500061451644, 3.027376345333613106, -5.243569643749998122 ) ) ;
#11742 = CARTESIAN_POINT ( 'NONE',  ( 9.787499999999999645, -2.886751345948129988, 4.999999999999997335 ) ) ;
#11743 = CARTESIAN_POINT ( 'NONE',  ( -2.828200636599751609E-16, 15.95000000122903216, 25.38119784648299770 ) ) ;
#11744 = CARTESIAN_POINT ( 'NONE',  ( 8.325000001229033941, 2.886751345948129099, -4.999999999999998224 ) ) ;
#11745 = CARTESIAN_POINT ( 'NONE',  ( 20.78437500061451715, 4.541064518000418104, 2.621784821874999949 ) ) ;
#11746 = CARTESIAN_POINT ( 'NONE',  ( 14.25937500061451679, -4.541064518000417216, -2.621784821875001281 ) ) ;
#11747 = FACE_OUTER_BOUND ( 'NONE', #37781, .T. ) ;
#11748 = ORIENTED_EDGE ( 'NONE', *, *, #1852, .F. ) ;
#11749 = CARTESIAN_POINT ( 'NONE',  ( 15.51562500061451644, -6.054752690667223547, -1.112240025338166033E-15 ) ) ;
#11750 = CARTESIAN_POINT ( 'NONE',  ( 26.13750000122903216, -4.330127018922194537, 2.499999999999995559 ) ) ;
#11751 = CARTESIAN_POINT ( 'NONE',  ( 14.18437500061451750, -4.541064518000419881, 2.621784821874995952 ) ) ;
#11752 = DIRECTION ( 'NONE',  ( -1.000000000000000000, -0.000000000000000000, -0.000000000000000000 ) ) ;
#11753 = CARTESIAN_POINT ( 'NONE',  ( 17.20312500061451644, 0.000000000000000000, 5.243569643749999010 ) ) ;
#11754 = LINE ( 'NONE', #28738, #36215 ) ;
#11755 = CARTESIAN_POINT ( 'NONE',  ( 25.39687500061451431, -3.027376345333614438, 5.243569643749998122 ) ) ;
#11756 = CARTESIAN_POINT ( 'NONE',  ( -4.243569643749999898, 10.35312500061451857, 30.00000000000000000 ) ) ;
#11757 = CARTESIAN_POINT ( 'NONE',  ( 14.44687500061451679, 6.054752690667223547, 3.707466751127219781E-16 ) ) ;
#11758 =( BOUNDED_CURVE ( )  B_SPLINE_CURVE ( 2, ( #5887, #28418, #51317, #23593, #6976 ),
 .UNSPECIFIED., .F., .F. ) 
 B_SPLINE_CURVE_WITH_KNOTS ( ( 3, 2, 3 ),
 ( 0.000000000000000000, 0.007246376811594202987, 0.01086956521739130578 ),
 .UNSPECIFIED. ) 
 CURVE ( )  GEOMETRIC_REPRESENTATION_ITEM ( )  RATIONAL_B_SPLINE_CURVE ( ( 1.000000000000000000, 0.8660254037844387076, 1.000000000000000000, 0.9330127018922192983, 0.9330127018922194093 ) ) 
 REPRESENTATION_ITEM ( '' )  );
#11759 = CARTESIAN_POINT ( 'NONE',  ( 12.18750000122903465, -4.330127018922194537, 2.499999999999995559 ) ) ;
#11760 = CARTESIAN_POINT ( 'NONE',  ( 7.734375000614517326, 4.119189519843966529, 2.378215178124999607 ) ) ;
#11761 = CARTESIAN_POINT ( 'NONE',  ( -2.121784821874996840, 15.88437500061451857, -26.32496088578401583 ) ) ;
#11762 = CARTESIAN_POINT ( 'NONE',  ( 17.89687500061451431, -3.027376345333610441, -5.243569643749999898 ) ) ;
#11763 = CARTESIAN_POINT ( 'NONE',  ( 21.07500000122903572, 2.886751345948126879, 4.999999999999999112 ) ) ;
#11764 =( BOUNDED_CURVE ( )  B_SPLINE_CURVE ( 2, ( #38237, #15333, #33064, #26432, #10173, #54147, #48603, #37511, #3910 ),
 .UNSPECIFIED., .F., .F. ) 
 B_SPLINE_CURVE_WITH_KNOTS ( ( 3, 2, 2, 2, 3 ),
 ( 0.7717391304347825942, 0.7753623188405797118, 0.7826086956521739468, 0.7898550724637680709, 0.7934782608695651884 ),
 .UNSPECIFIED. ) 
 CURVE ( )  GEOMETRIC_REPRESENTATION_ITEM ( )  RATIONAL_B_SPLINE_CURVE ( ( 0.9330127018922194093, 0.9330127018922194093, 1.000000000000000000, 0.8660254037844387076, 1.000000000000000000, 0.8660254037844387076, 1.000000000000000000, 0.9330127018922194093, 0.9330127018922194093 ) ) 
 REPRESENTATION_ITEM ( '' )  );
#11765 = CARTESIAN_POINT ( 'NONE',  ( 15.00937500061451679, 0.000000000000000000, 5.243569643749999010 ) ) ;
#11766 = CARTESIAN_POINT ( 'NONE',  ( 4.243569643749999010, 11.12187500061451928, 27.54997392385601174 ) ) ;
#11767 = CARTESIAN_POINT ( 'NONE',  ( 23.13750000122903216, 6.123233995736764310E-16, -4.999999999999998224 ) ) ;
#11768 = CARTESIAN_POINT ( 'NONE',  ( 15.29062500061451679, 6.054752690667223547, 3.707466751127219781E-16 ) ) ;
#11769 = DIRECTION ( 'NONE',  ( -1.000000000000000000, -0.000000000000000000, -0.000000000000000000 ) ) ;
#11770 = EDGE_LOOP ( 'NONE', ( #38255, #68411, #63895, #16632 ) ) ;
#11771 = ORIENTED_EDGE ( 'NONE', *, *, #29976, .F. ) ;
#11772 = CARTESIAN_POINT ( 'NONE',  ( 20.17499999999999716, -4.330127018922194537, 2.499999999999995559 ) ) ;
#11773 = DIRECTION ( 'NONE',  ( -1.000000000000000000, -0.000000000000000000, -0.000000000000000000 ) ) ;
#11774 = CARTESIAN_POINT ( 'NONE',  ( 3.478125000614517237, 6.421520780324663323E-16, -5.243569643749999010 ) ) ;
#11775 = EDGE_CURVE ( 'NONE', #25475, #39806, #52660, .T. ) ;
#11776 = CARTESIAN_POINT ( 'NONE',  ( 14.70000000122903394, 5.773502691896255534, 3.535250795749688894E-16 ) ) ;
#11777 = CARTESIAN_POINT ( 'NONE',  ( 20.80312500061451431, 0.000000000000000000, 5.243569643749999010 ) ) ;
#11778 = CARTESIAN_POINT ( 'NONE',  ( 22.75312500061451360, -4.541064518000417216, -2.621784821875001281 ) ) ;
#11779 = CARTESIAN_POINT ( 'NONE',  ( 6.290625000614517681, 6.054752690667223547, 3.707466751127219781E-16 ) ) ;
#11780 =( BOUNDED_CURVE ( )  B_SPLINE_CURVE ( 2, ( #42613, #37062, #13802, #59587, #8999, #31531, #30797, #54071, #24522 ),
 .UNSPECIFIED., .F., .F. ) 
 B_SPLINE_CURVE_WITH_KNOTS ( ( 3, 2, 2, 2, 3 ),
 ( 0.4583333333333333703, 0.4629629629629629650, 0.4722222222222222099, 0.4814814814814814548, 0.4861111111111111049 ),
 .UNSPECIFIED. ) 
 CURVE ( )  GEOMETRIC_REPRESENTATION_ITEM ( )  RATIONAL_B_SPLINE_CURVE ( ( 0.9330127018922194093, 0.9330127018922197424, 1.000000000000000000, 0.8660254037844387076, 1.000000000000000000, 0.8660254037844387076, 1.000000000000000000, 0.9330127018922194093, 0.9330127018922194093 ) ) 
 REPRESENTATION_ITEM ( '' )  );
#11781 = CARTESIAN_POINT ( 'NONE',  ( 28.91250000000000497, 2.886751345948129099, -4.999999999999998224 ) ) ;
#11782 = CARTESIAN_POINT ( 'NONE',  ( 9.271875000614516082, -5.492252693125287522, -1.008910452111647106E-15 ) ) ;
#11783 = CARTESIAN_POINT ( 'NONE',  ( 29.70937500061451431, 4.541064518000418104, -2.621784821874998173 ) ) ;
#11784 = CARTESIAN_POINT ( 'NONE',  ( 2.000000000000001332, 11.26250000122903394, -26.53589838486224650 ) ) ;
#11785 = CARTESIAN_POINT ( 'NONE',  ( -3.000416591977282496E-16, 17.94687500061451502, -34.90005215228797653 ) ) ;
#11786 = CARTESIAN_POINT ( 'NONE',  ( 6.225000001229036073, 2.886751345948126879, 4.999999999999999112 ) ) ;
#11787 = CARTESIAN_POINT ( 'NONE',  ( 8.587500000000002132, -2.886751345948125991, -5.000000000000000000 ) ) ;
#11788 = CARTESIAN_POINT ( 'NONE',  ( 3.112500001229034918, 0.000000000000000000, 4.999999999999998224 ) ) ;
#11789 = CARTESIAN_POINT ( 'NONE',  ( 11.78437500061451892, 4.541064518000418104, 2.621784821874999949 ) ) ;
#11790 = CARTESIAN_POINT ( 'NONE',  ( 23.62500000122902932, 2.886751345948095793, -5.000000000000055067 ) ) ;
#11791 = CARTESIAN_POINT ( 'NONE',  ( 3.946875000614517681, -3.027376345333610441, -5.243569643749999898 ) ) ;
#11792 = CARTESIAN_POINT ( 'NONE',  ( 12.00000000000000000, 0.000000000000000000, 4.999999999999998224 ) ) ;
#11793 = FACE_OUTER_BOUND ( 'NONE', #53184, .T. ) ;
#11794 = CARTESIAN_POINT ( 'NONE',  ( 10.54687500061451644, -3.027376345333614438, 5.243569643749998122 ) ) ;
#11795 = CARTESIAN_POINT ( 'NONE',  ( 14.10937500061451644, 0.000000000000000000, 5.243569643749999010 ) ) ;
#11796 = CARTESIAN_POINT ( 'NONE',  ( -1.999999999999997113, 18.72500000000000142, -26.53589838486224295 ) ) ;
#11797 = CARTESIAN_POINT ( 'NONE',  ( 6.262500000000000178, -5.773502691896255534, -1.060575238724906372E-15 ) ) ;
#11798 = CARTESIAN_POINT ( 'NONE',  ( -3.000416591977282496E-16, 16.99062500061459602, 25.09994784771203058 ) ) ;
#11799 = CARTESIAN_POINT ( 'NONE',  ( 20.82187500061451857, 3.027376345333611329, 5.243569643749999010 ) ) ;
#11800 = CYLINDRICAL_SURFACE ( 'NONE', #12750, 4.000000000000000000 ) ;
#11801 = EDGE_CURVE ( 'NONE', #18961, #7272, #32258, .T. ) ;
#11802 = CARTESIAN_POINT ( 'NONE',  ( 26.66250000122903430, -4.330127018922190985, -2.500000000000001332 ) ) ;
#11803 = CARTESIAN_POINT ( 'NONE',  ( 17.89687500061451431, 4.119189519843966529, -2.378215178124998275 ) ) ;
#11804 = CARTESIAN_POINT ( 'NONE',  ( 23.27812500061451573, 6.421520780324663323E-16, -5.243569643749999010 ) ) ;
#11805 = CARTESIAN_POINT ( 'NONE',  ( 14.65312500061451573, -4.541064518000417216, -2.621784821875001281 ) ) ;
#11806 = CARTESIAN_POINT ( 'NONE',  ( 25.09687500061451360, 4.119189519843966529, -2.378215178124998275 ) ) ;
#11807 = CARTESIAN_POINT ( 'NONE',  ( 13.05937500061451750, 4.541064518000418104, -2.621784821874998173 ) ) ;
#11808 = CARTESIAN_POINT ( 'NONE',  ( 27.48749999999999716, -2.886751345948125991, -5.000000000000000000 ) ) ;
#11809 = CARTESIAN_POINT ( 'NONE',  ( 24.30000000122903359, -2.886751345948129988, 4.999999999999997335 ) ) ;
#11810 = CARTESIAN_POINT ( 'NONE',  ( 2.934375000614518392, -4.541064518000419881, 2.621784821874995952 ) ) ;
#11811 = CARTESIAN_POINT ( 'NONE',  ( 14.74687500061451573, -3.027376345333610441, -5.243569643749999898 ) ) ;
#11812 = CARTESIAN_POINT ( 'NONE',  ( 5.810221930991193690E-16, 18.01249999999999574, 26.00000000000000000 ) ) ;
#11813 = CARTESIAN_POINT ( 'NONE',  ( 8.175000001229031810, -5.773502691896255534, -1.060575238724906372E-15 ) ) ;
#11814 = FACE_OUTER_BOUND ( 'NONE', #21555, .T. ) ;
#11815 = CARTESIAN_POINT ( 'NONE',  ( 22.28437500061451715, -4.541064518000419881, 2.621784821874995952 ) ) ;
#11816 = CARTESIAN_POINT ( 'NONE',  ( 13.39687500061451608, -3.027376345333610441, -5.243569643749999898 ) ) ;
#11817 = CARTESIAN_POINT ( 'NONE',  ( 3.756430356250000102, 18.60312499938548214, 30.00000000000000000 ) ) ;
#11818 = CARTESIAN_POINT ( 'NONE',  ( 26.36249999999999716, 2.886751345948126879, 4.999999999999999112 ) ) ;
#11819 = CARTESIAN_POINT ( 'NONE',  ( 2.737500001229034474, -4.330127018922194537, 2.499999999999995559 ) ) ;
#11820 = CARTESIAN_POINT ( 'NONE',  ( 27.08437500061451786, 4.119189519843966529, 2.378215178124999607 ) ) ;
#11821 = CARTESIAN_POINT ( 'NONE',  ( 16.71562500061451573, 3.027376345333611329, 5.243569643749999010 ) ) ;
#11822 = CARTESIAN_POINT ( 'NONE',  ( 6.150000000000003020, 0.000000000000000000, 4.999999999999998224 ) ) ;
#11823 = LINE ( 'NONE', #28097, #15998 ) ;
#11824 = CARTESIAN_POINT ( 'NONE',  ( 16.76249999999999929, 2.886751345948129099, -4.999999999999998224 ) ) ;
#11825 = CARTESIAN_POINT ( 'NONE',  ( -4.243569643749999898, 13.91562500061451679, 27.54997392385601529 ) ) ;
#11826 = CARTESIAN_POINT ( 'NONE',  ( -4.000000000000000000, 16.32499999999999929, 30.00000000000000000 ) ) ;
#11827 = CARTESIAN_POINT ( 'NONE',  ( 21.48750000122903003, 4.330127018922191873, 2.499999999999999556 ) ) ;
#11828 = CARTESIAN_POINT ( 'NONE',  ( 27.34687500061451360, -3.027376345333610441, -5.243569643749999898 ) ) ;
#11829 = ORIENTED_EDGE ( 'NONE', *, *, #38793, .F. ) ;
#11830 = CARTESIAN_POINT ( 'NONE',  ( 20.95312500061451999, -4.541064518000417216, -2.621784821875001281 ) ) ;
#11831 = CARTESIAN_POINT ( 'NONE',  ( 21.27187500061451786, 3.027376345333611329, 5.243569643749999010 ) ) ;
#11832 = CARTESIAN_POINT ( 'NONE',  ( 4.312500000000000000, 2.886751345948126879, 4.999999999999999112 ) ) ;
#11833 = CARTESIAN_POINT ( 'NONE',  ( 8.690625000614515372, -3.027376345333614438, 5.243569643749998122 ) ) ;
#11834 = CARTESIAN_POINT ( 'NONE',  ( 24.10312500061451502, -4.541064518000417216, -2.621784821875001281 ) ) ;
#11835 = CARTESIAN_POINT ( 'NONE',  ( 12.57187500061451857, 3.027376345333613106, -5.243569643749998122 ) ) ;
#11836 = CARTESIAN_POINT ( 'NONE',  ( 17.67187500061451644, 3.027376345333611329, 5.243569643749999010 ) ) ;
#11837 = CARTESIAN_POINT ( 'NONE',  ( -4.243569643749999898, 18.00312500061451715, 30.00000000000000000 ) ) ;
#11838 = CARTESIAN_POINT ( 'NONE',  ( 22.01250000122903216, 0.000000000000000000, 4.999999999999998224 ) ) ;
#11839 = CARTESIAN_POINT ( 'NONE',  ( 13.54687500061451821, 5.492252693125287522, 3.363034840372157021E-16 ) ) ;
#11840 = CARTESIAN_POINT ( 'NONE',  ( 11.76562500061451644, 3.027376345333611329, 5.243569643749999010 ) ) ;
#11841 = CARTESIAN_POINT ( 'NONE',  ( 4.621875000614516615, 3.027376345333611329, 5.243569643749999010 ) ) ;
#11842 = CARTESIAN_POINT ( 'NONE',  ( 5.071875000614519458, 3.027376345333611329, 5.243569643749999010 ) ) ;
#11843 = ORIENTED_EDGE ( 'NONE', *, *, #72200, .T. ) ;
#11844 = CARTESIAN_POINT ( 'NONE',  ( 25.39687500061451431, -3.027376345333614438, 5.243569643749998122 ) ) ;
#11845 = CARTESIAN_POINT ( 'NONE',  ( 16.00312500061451715, -4.541064518000417216, -2.621784821875001281 ) ) ;
#11846 = CARTESIAN_POINT ( 'NONE',  ( 27.63750000122903216, 6.123233995736764310E-16, -4.999999999999998224 ) ) ;
#11847 = CARTESIAN_POINT ( 'NONE',  ( 28.41562500061451502, 3.027376345333611329, 5.243569643749999010 ) ) ;
#11848 = CARTESIAN_POINT ( 'NONE',  ( 22.69687500061451857, -3.027376345333614438, 5.243569643749998122 ) ) ;
#11849 = CARTESIAN_POINT ( 'NONE',  ( 16.11562500061451786, 3.027376345333613106, -5.243569643749998122 ) ) ;
#11850 = CARTESIAN_POINT ( 'NONE',  ( -1.999999999999997113, 10.62500000000000000, 33.46410161513775705 ) ) ;
#11851 = CARTESIAN_POINT ( 'NONE',  ( 22.64062500061451644, -3.027376345333614438, 5.243569643749998122 ) ) ;
#11852 = CARTESIAN_POINT ( 'NONE',  ( 29.30625000122903145, -4.330127018922190985, -2.500000000000001332 ) ) ;
#11853 = ORIENTED_EDGE ( 'NONE', *, *, #19369, .F. ) ;
#11854 = CARTESIAN_POINT ( 'NONE',  ( 28.49999999999999645, 4.330127018922192761, -2.499999999999997780 ) ) ;
#11855 = CARTESIAN_POINT ( 'NONE',  ( 8.484601909799253346E-16, 13.81250000000000000, -25.38119784648299770 ) ) ;
#11856 = CARTESIAN_POINT ( 'NONE',  ( 1.878215178125000495, 18.22812499938548214, 26.74683588394047007 ) ) ;
#11857 = CARTESIAN_POINT ( 'NONE',  ( 29.35312500061451502, 0.000000000000000000, 5.243569643749999010 ) ) ;
#11858 = CARTESIAN_POINT ( 'NONE',  ( 9.778125000614517504, 6.421520780324663323E-16, -5.243569643749999010 ) ) ;
#11859 = CARTESIAN_POINT ( 'NONE',  ( 22.23750000122903003, 6.123233995736764310E-16, -4.999999999999998224 ) ) ;
#11860 = CARTESIAN_POINT ( 'NONE',  ( 12.38437500061451857, -4.541064518000419881, 2.621784821874995952 ) ) ;
#11861 = CARTESIAN_POINT ( 'NONE',  ( 27.44062500061451715, 6.054752690667223547, 3.707466751127219781E-16 ) ) ;
#11862 = CARTESIAN_POINT ( 'NONE',  ( 28.01249999999999574, 2.886751345948129099, -4.999999999999998224 ) ) ;
#11863 = CARTESIAN_POINT ( 'NONE',  ( 8.484601909799253346E-16, 19.32500000122902861, -25.38119784648299770 ) ) ;
#11864 = CARTESIAN_POINT ( 'NONE',  ( 25.23750000122903359, -4.330127018922194537, 2.499999999999995559 ) ) ;
#11865 = CARTESIAN_POINT ( 'NONE',  ( 11.87812500061451537, -4.541064518000419881, 2.621784821874995952 ) ) ;
#11866 = VERTEX_POINT ( 'NONE', #5655 ) ;
#11867 = CARTESIAN_POINT ( 'NONE',  ( 6.853125000614516793, 0.000000000000000000, 5.243569643749999010 ) ) ;
#11868 = CARTESIAN_POINT ( 'NONE',  ( 6.328125000614515550, 4.541064518000418104, 2.621784821874999949 ) ) ;
#11869 = CARTESIAN_POINT ( 'NONE',  ( 15.60937500061451644, -4.119189519843965641, -2.378215178125001383 ) ) ;
#11870 = DIRECTION ( 'NONE',  ( -0.000000000000000000, -1.000000000000000000, -0.000000000000000000 ) ) ;
#11871 = CARTESIAN_POINT ( 'NONE',  ( 15.75000000000000000, -4.330127018922190985, -2.500000000000001332 ) ) ;
#11872 = CARTESIAN_POINT ( 'NONE',  ( 15.60937500061451644, -4.541064518000417216, -2.621784821875001281 ) ) ;
#11873 = CARTESIAN_POINT ( 'NONE',  ( 11.92500000122903181, 2.886751345948129099, -4.999999999999998224 ) ) ;
#11874 = EDGE_CURVE ( 'NONE', #56056, #5140, #50719, .T. ) ;
#11875 = CARTESIAN_POINT ( 'NONE',  ( 18.53437500061451715, 4.541064518000418104, 2.621784821874999949 ) ) ;
#11876 = CARTESIAN_POINT ( 'NONE',  ( 16.76249999999999929, 2.886751345948129099, -4.999999999999998224 ) ) ;
#11877 = CARTESIAN_POINT ( 'NONE',  ( 20.63437500061451857, 6.421520780324663323E-16, -5.243569643749999010 ) ) ;
#11878 = CARTESIAN_POINT ( 'NONE',  ( 4.243569643749999010, 13.76562500061451644, -32.45002607614398471 ) ) ;
#11879 = CARTESIAN_POINT ( 'NONE',  ( 30.00000000000000000, 0.000000000000000000, 0.000000000000000000 ) ) ;
#11880 = CARTESIAN_POINT ( 'NONE',  ( 24.42187500061451289, -4.119189519843968306, 2.378215178124996054 ) ) ;
#11881 = CARTESIAN_POINT ( 'NONE',  ( 1.071796769724488785, 15.05134618820330061, 34.00000000000000000 ) ) ;
#11882 = CARTESIAN_POINT ( 'NONE',  ( 26.31562500061451715, -6.054752690667223547, -1.112240025338166033E-15 ) ) ;
#11883 = CARTESIAN_POINT ( 'NONE',  ( 28.28437500061451715, 6.421520780324663323E-16, -5.243569643749999010 ) ) ;
#11884 = CARTESIAN_POINT ( 'NONE',  ( 23.73749999999999716, -2.886751345948129988, 4.999999999999997335 ) ) ;
#11885 = EDGE_CURVE ( 'NONE', #54799, #11143, #51078, .T. ) ;
#11886 = CARTESIAN_POINT ( 'NONE',  ( 6.028125000614517504, -4.541064518000419881, 2.621784821874995952 ) ) ;
#11887 = CARTESIAN_POINT ( 'NONE',  ( 25.50937500061451502, 2.746126346562645981, -4.756430356249997438 ) ) ;
#11888 = CARTESIAN_POINT ( 'NONE',  ( 17.89687500061451431, -3.027376345333610441, -5.243569643749999898 ) ) ;
#11889 = CARTESIAN_POINT ( 'NONE',  ( 12.15937500061451537, 2.746126346562643317, 4.756430356249998326 ) ) ;
#11890 = CARTESIAN_POINT ( 'NONE',  ( 5.353125000614515905, 4.541064518000418104, -2.621784821874998173 ) ) ;
#11891 = CARTESIAN_POINT ( 'NONE',  ( 10.28437500061451715, 6.421520780324663323E-16, -5.243569643749999010 ) ) ;
#11892 = VERTEX_POINT ( 'NONE', #32090 ) ;
#11893 = CARTESIAN_POINT ( 'NONE',  ( 20.33437500061451786, 4.541064518000418104, 2.621784821874999949 ) ) ;
#11894 = DIRECTION ( 'NONE',  ( 0.000000000000000000, 0.000000000000000000, 1.000000000000000000 ) ) ;
#11895 = CARTESIAN_POINT ( 'NONE',  ( 28.08749999999999858, 5.773502691896255534, 3.535250795749688894E-16 ) ) ;
#11896 = CARTESIAN_POINT ( 'NONE',  ( 29.63437500061451502, 6.421520780324663323E-16, -5.243569643749999010 ) ) ;
#11897 = FACE_OUTER_BOUND ( 'NONE', #26436, .T. ) ;
#11898 = LINE ( 'NONE', #29256, #851 ) ;
#11899 = ORIENTED_EDGE ( 'NONE', *, *, #26844, .F. ) ;
#11900 = CARTESIAN_POINT ( 'NONE',  ( 9.449999999999999289, -4.330127018922190985, -2.500000000000001332 ) ) ;
#11901 = CARTESIAN_POINT ( 'NONE',  ( 14.03437500061451892, -2.746126346562646425, 4.756430356249996549 ) ) ;
#11902 = CARTESIAN_POINT ( 'NONE',  ( 24.14062500061451289, -3.027376345333610441, -5.243569643749999898 ) ) ;
#11903 = CARTESIAN_POINT ( 'NONE',  ( 14.84999999999999964, -4.330127018922190985, -2.500000000000001332 ) ) ;
#11904 = ADVANCED_FACE ( 'NONE', ( #3658 ), #49092, .F. ) ;
#11905 = CARTESIAN_POINT ( 'NONE',  ( 11.28750000122903252, -4.330127018922194537, 2.499999999999995559 ) ) ;
#11906 = CARTESIAN_POINT ( 'NONE',  ( 9.103125000614515017, 0.000000000000000000, 5.243569643749999010 ) ) ;
#11907 = CARTESIAN_POINT ( 'NONE',  ( 7.762500000000001954, 2.886751345948129099, -4.999999999999998224 ) ) ;
#11908 = DIRECTION ( 'NONE',  ( -1.000000000000000000, -0.000000000000000000, -0.000000000000000000 ) ) ;
#11909 = CARTESIAN_POINT ( 'NONE',  ( 29.02500000122903145, 2.886751345948129099, -4.999999999999998224 ) ) ;
#11910 = CARTESIAN_POINT ( 'NONE',  ( -3.756430356250000102, 16.01562499938548356, 30.00000000000000000 ) ) ;
#11911 = CARTESIAN_POINT ( 'NONE',  ( 7.612500000000000711, -5.773502691896255534, -1.060575238724906372E-15 ) ) ;
#11912 = CARTESIAN_POINT ( 'NONE',  ( 18.97499999999999787, 6.123233995736764310E-16, -4.999999999999998224 ) ) ;
#11913 = ORIENTED_EDGE ( 'NONE', *, *, #29578, .T. ) ;
#11914 = CARTESIAN_POINT ( 'NONE',  ( 21.55312500061451431, 4.541064518000418104, -2.621784821874998173 ) ) ;
#11915 = CARTESIAN_POINT ( 'NONE',  ( 29.72812500061451502, 4.541064518000418104, 2.621784821874999949 ) ) ;
#11916 = CARTESIAN_POINT ( 'NONE',  ( 28.84687500061452070, 6.054752690667223547, 3.707466751127219781E-16 ) ) ;
#11917 = CARTESIAN_POINT ( 'NONE',  ( 19.65937500061451360, -4.541064518000417216, -2.621784821875001281 ) ) ;
#11918 = CARTESIAN_POINT ( 'NONE',  ( 17.27812500061451217, -4.541064518000419881, 2.621784821874995952 ) ) ;
#11919 = CARTESIAN_POINT ( 'NONE',  ( -4.243569643749998122, 12.64062500061459460, -27.54997392385601174 ) ) ;
#11920 = CARTESIAN_POINT ( 'NONE',  ( 4.115625000614516082, 3.027376345333611329, 5.243569643749999010 ) ) ;
#11921 = CARTESIAN_POINT ( 'NONE',  ( 28.95000000122903572, -2.886751345948125991, -5.000000000000000000 ) ) ;
#11922 = CARTESIAN_POINT ( 'NONE',  ( 22.92187500061451644, 2.746126346562645981, -4.756430356249997438 ) ) ;
#11923 = CARTESIAN_POINT ( 'NONE',  ( 19.90312500061451573, 0.000000000000000000, 5.243569643749999010 ) ) ;
#11924 = CARTESIAN_POINT ( 'NONE',  ( 24.99375000122903145, 5.773502691896255534, 3.535250795749688401E-16 ) ) ;
#11925 = CARTESIAN_POINT ( 'NONE',  ( 3.862500001229035362, 4.330127018922192761, -2.499999999999997780 ) ) ;
#11926 = CARTESIAN_POINT ( 'NONE',  ( 13.50937500061451679, 4.541064518000418104, -2.621784821874998173 ) ) ;
#11927 = CARTESIAN_POINT ( 'NONE',  ( 13.17187500061451999, 3.027376345333611329, 5.243569643749999010 ) ) ;
#11928 = CARTESIAN_POINT ( 'NONE',  ( 20.93437500061451573, -4.541064518000419881, 2.621784821874995952 ) ) ;
#11929 = ORIENTED_EDGE ( 'NONE', *, *, #22798, .T. ) ;
#11930 = CARTESIAN_POINT ( 'NONE',  ( -5.810221930991193690E-16, 15.83749999999999680, -34.00000000000000000 ) ) ;
#11931 = CARTESIAN_POINT ( 'NONE',  ( 25.19062500061451715, 6.054752690667223547, 3.707466751127219781E-16 ) ) ;
#11932 = CARTESIAN_POINT ( 'NONE',  ( 17.93437500061451928, 6.421520780324663323E-16, -5.243569643749999010 ) ) ;
#11933 = CARTESIAN_POINT ( 'NONE',  ( 24.29062500061451502, 6.054752690667223547, 3.707466751127219781E-16 ) ) ;
#11934 = CARTESIAN_POINT ( 'NONE',  ( 27.26249999999999929, 2.886751345948161074, 4.999999999999941380 ) ) ;
#11935 = CARTESIAN_POINT ( 'NONE',  ( -3.999999999999999112, 16.85000000000000142, 30.00000000000000000 ) ) ;
#11936 = CARTESIAN_POINT ( 'NONE',  ( 3.459375000614519635, -4.541064518000417216, -2.621784821875001281 ) ) ;
#11937 = CARTESIAN_POINT ( 'NONE',  ( 11.81250000122903465, -4.330127018922190985, -2.500000000000001332 ) ) ;
#11938 = CARTESIAN_POINT ( 'NONE',  ( 7.575000001229033053, 2.886751345948126879, 4.999999999999999112 ) ) ;
#11939 = CARTESIAN_POINT ( 'NONE',  ( 28.98750000122903359, 6.123233995736764310E-16, -4.999999999999998224 ) ) ;
#11940 = CARTESIAN_POINT ( 'NONE',  ( 26.70000000122903572, -2.886751345948125991, -5.000000000000000000 ) ) ;
#11941 = CARTESIAN_POINT ( 'NONE',  ( 4.000000000000000000, 18.74374999877096570, 30.00000000000000000 ) ) ;
#11942 = CARTESIAN_POINT ( 'NONE',  ( 15.43125000122903323, 6.123233995736764310E-16, -4.999999999999998224 ) ) ;
#11943 = CARTESIAN_POINT ( 'NONE',  ( 10.62187500061451928, -6.054752690667223547, -1.112240025338166033E-15 ) ) ;
#11944 = CARTESIAN_POINT ( 'NONE',  ( 1.999999999999998668, 14.90000000000000036, -33.46410161513775705 ) ) ;
#11945 = CARTESIAN_POINT ( 'NONE',  ( 16.22812500061451857, 4.541064518000418104, 2.621784821874999949 ) ) ;
#11946 = CARTESIAN_POINT ( 'NONE',  ( 13.43437500061451750, 6.421520780324663323E-16, -5.243569643749999010 ) ) ;
#11947 = CARTESIAN_POINT ( 'NONE',  ( 3.403125000614518836, -4.541064518000417216, -2.621784821875001281 ) ) ;
#11948 = CARTESIAN_POINT ( 'NONE',  ( 19.73437500061451644, 6.421520780324663323E-16, -5.243569643749999010 ) ) ;
#11949 = CARTESIAN_POINT ( 'NONE',  ( 8.034375000614518925, 6.421520780324663323E-16, -5.243569643749999010 ) ) ;
#11950 = CARTESIAN_POINT ( 'NONE',  ( 3.065625000614517592, 3.027376345333613106, -5.243569643749998122 ) ) ;
#11951 = CARTESIAN_POINT ( 'NONE',  ( 3.999999999999998668, 16.06250000000000000, 32.30940107675850470 ) ) ;
#11952 = CARTESIAN_POINT ( 'NONE',  ( 11.27812500061451573, 4.541064518000418104, 2.621784821874999949 ) ) ;
#11953 = CARTESIAN_POINT ( 'NONE',  ( 19.56562500061451715, -6.054752690667223547, -1.112240025338166033E-15 ) ) ;
#11954 = VERTEX_POINT ( 'NONE', #37263 ) ;
#11955 = CARTESIAN_POINT ( 'NONE',  ( 4.950000001229033941, -2.886751345948129988, 4.999999999999997335 ) ) ;
#11956 = CARTESIAN_POINT ( 'NONE',  ( 16.79062500061451857, -3.027376345333614438, 5.243569643749998122 ) ) ;
#11957 = CARTESIAN_POINT ( 'NONE',  ( 12.96562500061451750, 3.027376345333613106, -5.243569643749998122 ) ) ;
#11958 = CARTESIAN_POINT ( 'NONE',  ( 24.53437500061451715, -4.119189519843968306, 2.378215178124996054 ) ) ;
#11959 = CARTESIAN_POINT ( 'NONE',  ( 12.48750000000000249, -2.886751345948129988, 4.999999999999997335 ) ) ;
#11960 = CARTESIAN_POINT ( 'NONE',  ( 8.100000001229034297, -2.886751345948129988, 4.999999999999997335 ) ) ;
#11961 = PRODUCT_DEFINITION_SHAPE ( 'NONE', 'NONE',  #58930 ) ;
#11962 = CARTESIAN_POINT ( 'NONE',  ( 5.203125000614518214, -4.541064518000417216, -2.621784821875001281 ) ) ;
#11963 = CARTESIAN_POINT ( 'NONE',  ( 18.82500000122903216, 2.886751345948126879, 4.999999999999999112 ) ) ;
#11964 = CARTESIAN_POINT ( 'NONE',  ( 26.84999999999999787, 0.000000000000000000, 4.999999999999998224 ) ) ;
#11965 = CARTESIAN_POINT ( 'NONE',  ( -4.243569643749999898, 10.40937500061451892, -30.00000000000000000 ) ) ;
#11966 = DIRECTION ( 'NONE',  ( 0.000000000000000000, 0.000000000000000000, -1.000000000000000000 ) ) ;
#11967 = ADVANCED_FACE ( 'NONE', ( #25071 ), #70145, .T. ) ;
#11968 = CARTESIAN_POINT ( 'NONE',  ( 3.862500001229035362, 4.330127018922192761, -2.499999999999997780 ) ) ;
#11969 = CARTESIAN_POINT ( 'NONE',  ( 1.999999999999997335, 14.67500000000000071, 33.46410161513775705 ) ) ;
#11970 = CARTESIAN_POINT ( 'NONE',  ( 18.34687500061451715, -3.027376345333610441, -5.243569643749999898 ) ) ;
#11971 =( BOUNDED_CURVE ( )  B_SPLINE_CURVE ( 2, ( #12833, #63078, #17639, #18363, #51278, #24282, #40199, #46830, #2131 ),
 .UNSPECIFIED., .F., .F. ) 
 B_SPLINE_CURVE_WITH_KNOTS ( ( 3, 2, 2, 2, 3 ),
 ( 0.09782608695652174335, 0.1014492753623188470, 0.1086956521739130405, 0.1159420289855072478, 0.1195652173913043514 ),
 .UNSPECIFIED. ) 
 CURVE ( )  GEOMETRIC_REPRESENTATION_ITEM ( )  RATIONAL_B_SPLINE_CURVE ( ( 0.9330127018922194093, 0.9330127018922194093, 1.000000000000000000, 0.8660254037844387076, 1.000000000000000000, 0.8660254037844387076, 1.000000000000000000, 0.9330127018922194093, 0.9330127018922194093 ) ) 
 REPRESENTATION_ITEM ( '' )  );
#11972 = CYLINDRICAL_SURFACE ( 'NONE', #30363, 4.999999999999998224 ) ;
#11973 = CARTESIAN_POINT ( 'NONE',  ( 17.24062500061451786, -3.027376345333614438, 5.243569643749998122 ) ) ;
#11974 = CARTESIAN_POINT ( 'NONE',  ( 9.693750001229032520, 5.773502691896255534, 3.535250795749688894E-16 ) ) ;
#11975 = DIRECTION ( 'NONE',  ( 0.000000000000000000, 0.000000000000000000, 1.000000000000000000 ) ) ;
#11976 = CARTESIAN_POINT ( 'NONE',  ( 28.99687500061451573, -3.027376345333614438, 5.243569643749998122 ) ) ;
#11977 = CARTESIAN_POINT ( 'NONE',  ( 27.04687500061451644, 6.054752690667223547, 3.707466751127219781E-16 ) ) ;
#11978 = CARTESIAN_POINT ( 'NONE',  ( 19.50937500061451857, -5.492252693125287522, -1.008910452111647106E-15 ) ) ;
#11979 = CARTESIAN_POINT ( 'NONE',  ( 12.59062500061451573, 6.054752690667223547, 3.707466751127219781E-16 ) ) ;
#11980 = CARTESIAN_POINT ( 'NONE',  ( 10.13437500061451679, -4.541064518000419881, 2.621784821874995952 ) ) ;
#11981 = EDGE_LOOP ( 'NONE', ( #48610, #31142, #50193, #30737 ) ) ;
#11982 = CARTESIAN_POINT ( 'NONE',  ( 9.487499999999997158, -2.886751345948126435, -5.000000000000000000 ) ) ;
#11983 = CARTESIAN_POINT ( 'NONE',  ( 19.41562500061451146, 3.027376345333611329, 5.243569643749999010 ) ) ;
#11984 = CARTESIAN_POINT ( 'NONE',  ( 17.70000000122903216, -2.886751345948126435, -5.000000000000000000 ) ) ;
#11985 = CARTESIAN_POINT ( 'NONE',  ( 34.99999999999999289, -4.500000000000000000, 5.500000000000000000 ) ) ;
#11986 = CARTESIAN_POINT ( 'NONE',  ( 10.01250000000000107, 2.886751345948129099, -4.999999999999998224 ) ) ;
#11987 = CARTESIAN_POINT ( 'NONE',  ( 21.30000000122903359, -2.886751345948125991, -5.000000000000000000 ) ) ;
#11988 = CARTESIAN_POINT ( 'NONE',  ( 15.21562500061451750, 3.027376345333613106, -5.243569643749998122 ) ) ;
#11989 = CARTESIAN_POINT ( 'NONE',  ( 12.12187500061451573, 4.119189519843966529, 2.378215178124999607 ) ) ;
#11990 = ORIENTED_EDGE ( 'NONE', *, *, #25258, .T. ) ;
#11991 = CARTESIAN_POINT ( 'NONE',  ( 19.87500000000000000, 6.123233995736764310E-16, -4.999999999999998224 ) ) ;
#11992 = CARTESIAN_POINT ( 'NONE',  ( 21.15000000000000213, -4.330127018922190985, -2.500000000000001332 ) ) ;
#11993 = CARTESIAN_POINT ( 'NONE',  ( 22.17187500061451644, 3.027376345333611329, 5.243569643749999010 ) ) ;
#11994 = CARTESIAN_POINT ( 'NONE',  ( 26.01562500061451289, 3.027376345333613106, -5.243569643749998122 ) ) ;
#11995 = ORIENTED_EDGE ( 'NONE', *, *, #17977, .F. ) ;
#11996 = CARTESIAN_POINT ( 'NONE',  ( 13.72500000000000142, 4.330127018922191873, 2.499999999999999556 ) ) ;
#11997 = CARTESIAN_POINT ( 'NONE',  ( 7.303125000614516082, 0.000000000000000000, 5.243569643749999010 ) ) ;
#11998 = CARTESIAN_POINT ( 'NONE',  ( 4.000000000000000000, 12.08750000000000036, 32.30940107675849760 ) ) ;
#11999 = CARTESIAN_POINT ( 'NONE',  ( 13.98750000000000249, -2.886751345948125991, -5.000000000000000000 ) ) ;
#12000 = CARTESIAN_POINT ( 'NONE',  ( 2.121784821875001281, 16.80312500061451786, 33.67503911421598417 ) ) ;
#12001 = CARTESIAN_POINT ( 'NONE',  ( 29.05312500061451431, -4.541064518000417216, -2.621784821875001281 ) ) ;
#12002 = CARTESIAN_POINT ( 'NONE',  ( 25.80937500061451928, 0.000000000000000000, 5.243569643749999010 ) ) ;
#12003 = ORIENTED_EDGE ( 'NONE', *, *, #3447, .F. ) ;
#12004 = CARTESIAN_POINT ( 'NONE',  ( 23.31562500061451715, 3.027376345333613106, -5.243569643749998122 ) ) ;
#12005 = CARTESIAN_POINT ( 'NONE',  ( 26.10937500061451644, 4.541064518000418104, -2.621784821874998173 ) ) ;
#12006 = CARTESIAN_POINT ( 'NONE',  ( 4.243569643749999898, 17.77812500061459389, -30.00000000000000000 ) ) ;
#12007 = CARTESIAN_POINT ( 'NONE',  ( 10.95000000000000107, 4.330127018922192761, -2.499999999999997780 ) ) ;
#12008 = CARTESIAN_POINT ( 'NONE',  ( 9.178125000614517859, -4.541064518000419881, 2.621784821874995952 ) ) ;
#12009 = CARTESIAN_POINT ( 'NONE',  ( 29.67187500061451644, 2.746126346562645981, -4.756430356249997438 ) ) ;
#12010 = CARTESIAN_POINT ( 'NONE',  ( 29.80312500061451431, 0.000000000000000000, 5.243569643749999010 ) ) ;
#12011 = CARTESIAN_POINT ( 'NONE',  ( 26.20312500061451644, 0.000000000000000000, 5.243569643749999010 ) ) ;
#12012 = CARTESIAN_POINT ( 'NONE',  ( 26.82187500061451502, 5.824947211148865298E-16, -4.756430356249998326 ) ) ;
#12013 = CARTESIAN_POINT ( 'NONE',  ( 13.32187500061451502, -5.492252693125287522, -1.008910452111647106E-15 ) ) ;
#12014 = CARTESIAN_POINT ( 'NONE',  ( 18.75937500061451857, -4.541064518000417216, -2.621784821875001281 ) ) ;
#12015 = CARTESIAN_POINT ( 'NONE',  ( -3.000416591977282496E-16, 12.09687500061451715, 25.09994784771203058 ) ) ;
#12016 = CARTESIAN_POINT ( 'NONE',  ( 20.29687500061451644, 6.054752690667223547, 3.707466751127219781E-16 ) ) ;
#12017 = CARTESIAN_POINT ( 'NONE',  ( 26.85937500061451644, -4.541064518000417216, -2.621784821875001281 ) ) ;
#12018 = CARTESIAN_POINT ( 'NONE',  ( -4.243569643749999898, 16.22187500061452070, 27.54997392385601529 ) ) ;
#12019 = CARTESIAN_POINT ( 'NONE',  ( 6.965625000614518392, -6.054752690667223547, -1.112240025338166033E-15 ) ) ;
#12020 = CARTESIAN_POINT ( 'NONE',  ( -6.275039685470489619E-15, 18.31250000000000000, -26.00000000000000355 ) ) ;
#12021 = CARTESIAN_POINT ( 'NONE',  ( 5.071875000614519458, 3.027376345333611329, 5.243569643749999010 ) ) ;
#12022 = CARTESIAN_POINT ( 'NONE',  ( -1.071796769724483234, 15.97009619066136565, -34.00000000000000711 ) ) ;
#12023 = CARTESIAN_POINT ( 'NONE',  ( 6.965625000614518392, -6.054752690667223547, -1.112240025338166033E-15 ) ) ;
#12024 = CARTESIAN_POINT ( 'NONE',  ( 12.79687500061451821, -3.027376345333614438, 5.243569643749998122 ) ) ;
#12025 = CARTESIAN_POINT ( 'NONE',  ( 19.57500000122903216, 2.886751345948129099, -4.999999999999998224 ) ) ;
#12026 = CARTESIAN_POINT ( 'NONE',  ( 6.159375000614517148, -4.541064518000417216, -2.621784821875001281 ) ) ;
#12027 = CARTESIAN_POINT ( 'NONE',  ( 7.415625000614516793, -6.054752690667223547, -1.112240025338166033E-15 ) ) ;
#12028 = CARTESIAN_POINT ( 'NONE',  ( 5.203125000614518214, -4.541064518000417216, -2.621784821875001281 ) ) ;
#12029 = CARTESIAN_POINT ( 'NONE',  ( 22.29375000122903216, 5.773502691896255534, 3.535250795749688894E-16 ) ) ;
#12030 = CARTESIAN_POINT ( 'NONE',  ( 15.79687500061451821, 6.054752690667223547, 3.707466751127219781E-16 ) ) ;
#12031 = CARTESIAN_POINT ( 'NONE',  ( 19.53750000122903430, 6.123233995736764310E-16, -4.999999999999998224 ) ) ;
#12032 = ORIENTED_EDGE ( 'NONE', *, *, #3723, .F. ) ;
#12033 = CARTESIAN_POINT ( 'NONE',  ( 24.32812500061451289, 4.541064518000418104, 2.621784821874999949 ) ) ;
#12034 = CARTESIAN_POINT ( 'NONE',  ( 8.990625000614516082, 6.054752690667223547, 3.707466751127219781E-16 ) ) ;
#12035 = CARTESIAN_POINT ( 'NONE',  ( 28.05937500061451573, 0.000000000000000000, 5.243569643749999010 ) ) ;
#12036 = CARTESIAN_POINT ( 'NONE',  ( 11.01562500061451821, -6.054752690667223547, -1.112240025338166033E-15 ) ) ;
#12037 = CARTESIAN_POINT ( 'NONE',  ( 28.94999999999999929, 4.330127018922192761, -2.499999999999997780 ) ) ;
#12038 = CARTESIAN_POINT ( 'NONE',  ( 13.98750000122903359, -4.330127018922194537, 2.499999999999995559 ) ) ;
#12039 = ADVANCED_FACE ( 'NONE', ( #59785 ), #48357, .T. ) ;
#12040 = CARTESIAN_POINT ( 'NONE',  ( 27.66562500061451146, -6.054752690667223547, -1.112240025338166033E-15 ) ) ;
#12041 = VECTOR ( 'NONE', #69183, 1000.000000000000000 ) ;
#12042 = CARTESIAN_POINT ( 'NONE',  ( -4.243569643749999898, 12.11562500061451608, -32.45002607614398471 ) ) ;
#12043 = CARTESIAN_POINT ( 'NONE',  ( 13.42500000122903536, 2.886751345948126879, 4.999999999999999112 ) ) ;
#12044 = CARTESIAN_POINT ( 'NONE',  ( 11.13750000000000284, -2.886751345948129988, 4.999999999999997335 ) ) ;
#12045 = CARTESIAN_POINT ( 'NONE',  ( 19.64062500061451644, -3.027376345333610441, -5.243569643749999898 ) ) ;
#12046 = CARTESIAN_POINT ( 'NONE',  ( 8.746875000614515727, -3.027376345333614438, 5.243569643749998122 ) ) ;
#12047 = CARTESIAN_POINT ( 'NONE',  ( 20.32499999999999929, 6.123233995736764310E-16, -4.999999999999998224 ) ) ;
#12048 = CARTESIAN_POINT ( 'NONE',  ( 7.237500001229035362, -4.330127018922194537, 2.499999999999995559 ) ) ;
#12049 = CARTESIAN_POINT ( 'NONE',  ( 15.82500000122903216, -5.773502691896255534, -1.060575238724906372E-15 ) ) ;
#12050 = CARTESIAN_POINT ( 'NONE',  ( 12.74062500061451786, -3.027376345333614438, 5.243569643749998122 ) ) ;
#12051 = CARTESIAN_POINT ( 'NONE',  ( 15.77812500061451573, 4.541064518000418104, 2.621784821874999949 ) ) ;
#12052 = CARTESIAN_POINT ( 'NONE',  ( 24.48750000122903359, 6.123233995736764310E-16, -4.999999999999998224 ) ) ;
#12053 = CARTESIAN_POINT ( 'NONE',  ( 21.03750000000000142, -2.886751345948129988, 4.999999999999997335 ) ) ;
#12054 = CARTESIAN_POINT ( 'NONE',  ( 23.18437500061451573, -4.541064518000419881, 2.621784821874995952 ) ) ;
#12055 = CARTESIAN_POINT ( 'NONE',  ( 25.61250000122903359, 0.000000000000000000, 4.999999999999998224 ) ) ;
#12056 = EDGE_CURVE ( 'NONE', #6778, #36605, #29871, .T. ) ;
#12057 = CARTESIAN_POINT ( 'NONE',  ( 9.300000001229035362, 5.773502691896255534, 3.535250795749688894E-16 ) ) ;
#12058 = CARTESIAN_POINT ( 'NONE',  ( 9.121875000614517504, 3.027376345333611329, 5.243569643749999010 ) ) ;
#12059 = CARTESIAN_POINT ( 'NONE',  ( 25.28437500061451715, 4.541064518000418104, 2.621784821874999949 ) ) ;
#12060 = CARTESIAN_POINT ( 'NONE',  ( 4.241234947910677455, -2.648004176096003803, -4.329066063250716745 ) ) ;
#12061 = CARTESIAN_POINT ( 'NONE',  ( 24.36562500061451786, 3.027376345333611329, 5.243569643749999010 ) ) ;
#12062 = CARTESIAN_POINT ( 'NONE',  ( 27.00937500061451857, 4.541064518000418104, -2.621784821874998173 ) ) ;
#12063 = CARTESIAN_POINT ( 'NONE',  ( 1.878215178125000495, 15.52812499938548285, 26.74683588394047007 ) ) ;
#12064 = CARTESIAN_POINT ( 'NONE',  ( 65.00000000000000000, -5.218601775200160553, -7.332543590861065219 ) ) ;
#12065 = CARTESIAN_POINT ( 'NONE',  ( 9.009375000614518569, 4.541064518000418104, -2.621784821874998173 ) ) ;
#12066 = CARTESIAN_POINT ( 'NONE',  ( 4.411272977760241965, 2.353862934769528792, -4.685547128476531320 ) ) ;
#12067 = CARTESIAN_POINT ( 'NONE',  ( 28.67812500061451431, 6.421520780324663323E-16, -5.243569643749999010 ) ) ;
#12068 = CARTESIAN_POINT ( 'NONE',  ( 5.934375000614517504, 4.541064518000418104, 2.621784821874999949 ) ) ;
#12069 = CARTESIAN_POINT ( 'NONE',  ( -1.071796769724483234, 16.42009619066137205, -34.00000000000000711 ) ) ;
#12070 = CARTESIAN_POINT ( 'NONE',  ( 25.39687500061451431, -3.027376345333614438, 5.243569643749998122 ) ) ;
#12071 = EDGE_CURVE ( 'NONE', #60642, #58564, #7846, .T. ) ;
#12072 = CARTESIAN_POINT ( 'NONE',  ( 4.243569643749999010, 11.06562500061459531, 27.54997392385601174 ) ) ;
#12073 = CARTESIAN_POINT ( 'NONE',  ( 18.07499999999999929, 6.123233995736764310E-16, -4.999999999999998224 ) ) ;
#12074 = EDGE_LOOP ( 'NONE', ( #67690, #43712, #6897, #4856, #61410, #3773 ) ) ;
#12075 = CARTESIAN_POINT ( 'NONE',  ( 26.28749999999999432, 5.773502691896255534, 3.535250795749688894E-16 ) ) ;
#12076 = CARTESIAN_POINT ( 'NONE',  ( 29.40937500061451715, 0.000000000000000000, 5.243569643749999010 ) ) ;
#12077 = EDGE_LOOP ( 'NONE', ( #60413, #20561, #29935, #57048, #69383, #13880, #29068, #39982 ) ) ;
#12078 = VECTOR ( 'NONE', #71891, 1000.000000000000000 ) ;
#12079 = CARTESIAN_POINT ( 'NONE',  ( 16.07812500061451289, 6.421520780324663323E-16, -5.243569643749999010 ) ) ;
#12080 = CARTESIAN_POINT ( 'NONE',  ( 6.140625000614516438, -3.027376345333610441, -5.243569643749999898 ) ) ;
#12081 = CARTESIAN_POINT ( 'NONE',  ( 19.05937500061451217, -5.492252693125287522, -1.008910452111647106E-15 ) ) ;
#12082 = CARTESIAN_POINT ( 'NONE',  ( 5.146875000614517859, -3.027376345333614438, 5.243569643749998122 ) ) ;
#12083 = CARTESIAN_POINT ( 'NONE',  ( 16.01250000122903216, 4.330127018922192761, -2.499999999999997780 ) ) ;
#12084 = CARTESIAN_POINT ( 'NONE',  ( 21.63749999999999929, -2.886751345948125991, -5.000000000000000000 ) ) ;
#12085 = CARTESIAN_POINT ( 'NONE',  ( 29.92500000000000071, 4.330127018922191873, 2.499999999999999556 ) ) ;
#12086 = CARTESIAN_POINT ( 'NONE',  ( 4.621875000614516615, 3.027376345333611329, 5.243569643749999010 ) ) ;
#12087 = CARTESIAN_POINT ( 'NONE',  ( 10.39687500061451786, 6.054752690667223547, 3.707466751127219781E-16 ) ) ;
#12088 = CARTESIAN_POINT ( 'NONE',  ( 21.19687500061451502, 6.054752690667223547, 3.707466751127219781E-16 ) ) ;
#12089 = LINE ( 'NONE', #23525, #8826 ) ;
#12090 = ORIENTED_EDGE ( 'NONE', *, *, #56574, .T. ) ;
#12091 = CARTESIAN_POINT ( 'NONE',  ( 4.059375000614519280, 4.541064518000418104, -2.621784821874998173 ) ) ;
#12092 = CARTESIAN_POINT ( 'NONE',  ( 7.996875000614519280, -3.027376345333610441, -5.243569643749999898 ) ) ;
#12093 = CARTESIAN_POINT ( 'NONE',  ( 17.55000000000000071, -4.330127018922190985, -2.500000000000001332 ) ) ;
#12094 = CARTESIAN_POINT ( 'NONE',  ( 16.60312500061451857, 4.541064518000418104, -2.621784821874998173 ) ) ;
#12095 = CARTESIAN_POINT ( 'NONE',  ( 4.000000000000000000, 19.28750000000000142, 27.69059892324149530 ) ) ;
#12096 = CARTESIAN_POINT ( 'NONE',  ( -2.000000000000000000, 19.92500000000000071, 26.53589838486224650 ) ) ;
#12097 = CARTESIAN_POINT ( 'NONE',  ( 21.15937500061451715, 4.119189519843966529, -2.378215178124998275 ) ) ;
#12098 = CARTESIAN_POINT ( 'NONE',  ( 10.67812500061451608, 6.421520780324663323E-16, -5.243569643749999010 ) ) ;
#12099 = CARTESIAN_POINT ( 'NONE',  ( 25.50937500061451502, -4.541064518000417216, -2.621784821875001281 ) ) ;
#12100 = CARTESIAN_POINT ( 'NONE',  ( 12.67499999999999893, 6.123233995736764310E-16, -4.999999999999998224 ) ) ;
#12101 = CARTESIAN_POINT ( 'NONE',  ( 25.32187500061451857, 3.027376345333611329, 5.243569643749999010 ) ) ;
#12102 = CARTESIAN_POINT ( 'NONE',  ( 7.575000000000001954, -4.330127018922194537, 2.499999999999995559 ) ) ;
#12103 = CARTESIAN_POINT ( 'NONE',  ( 8.484601909799253346E-16, 12.12500000122903465, 34.61880215351700230 ) ) ;
#12104 = CARTESIAN_POINT ( 'NONE',  ( 6.637500001229035718, 4.330127018922191873, 2.499999999999999556 ) ) ;
#12105 = CARTESIAN_POINT ( 'NONE',  ( 19.35937500061451644, 4.541064518000418104, -2.621784821874998173 ) ) ;
#12106 = CARTESIAN_POINT ( 'NONE',  ( 10.62187500061451928, -6.054752690667223547, -1.112240025338166033E-15 ) ) ;
#12107 = CARTESIAN_POINT ( 'NONE',  ( -3.992479141629562633, 3.010095094815111505, -29.71890115206955585 ) ) ;
#12108 = ORIENTED_EDGE ( 'NONE', *, *, #55155, .T. ) ;
#12109 = CARTESIAN_POINT ( 'NONE',  ( 14.72812500061451679, 6.421520780324663323E-16, -5.243569643749999010 ) ) ;
#12110 = CARTESIAN_POINT ( 'NONE',  ( 27.11250000122903359, -4.330127018922190985, -2.500000000000001332 ) ) ;
#12111 = CARTESIAN_POINT ( 'NONE',  ( 12.94687500061451857, -3.027376345333610441, -5.243569643749999898 ) ) ;
#12112 = CARTESIAN_POINT ( 'NONE',  ( 3.821851807532226530, -4.035565604595362288, 3.497334623063416803 ) ) ;
#12113 = CARTESIAN_POINT ( 'NONE',  ( 14.16562500061451679, -6.054752690667223547, -1.112240025338166033E-15 ) ) ;
#12114 = DIRECTION ( 'NONE',  ( -1.000000000000000000, -0.000000000000000000, -0.000000000000000000 ) ) ;
#12115 = CARTESIAN_POINT ( 'NONE',  ( 25.88437500061451502, -4.541064518000419881, 2.621784821874995952 ) ) ;
#12116 = CARTESIAN_POINT ( 'NONE',  ( -2.121784821874999949, 10.27812500061451750, 26.32496088578401938 ) ) ;
#12117 = CARTESIAN_POINT ( 'NONE',  ( 12.11250000122903181, 0.000000000000000000, 4.999999999999998224 ) ) ;
#12118 = CARTESIAN_POINT ( 'NONE',  ( 8.634375000614518569, 4.119189519843966529, 2.378215178124999607 ) ) ;
#12119 = CARTESIAN_POINT ( 'NONE',  ( 4.243569643749999898, 17.83437500061451786, -30.00000000000000000 ) ) ;
#12120 = CARTESIAN_POINT ( 'NONE',  ( 18.57187500061451857, 3.027376345333611329, 5.243569643749999010 ) ) ;
#12121 = CARTESIAN_POINT ( 'NONE',  ( 19.20000000122903572, 5.773502691896255534, 3.535250795749688894E-16 ) ) ;
#12122 = CARTESIAN_POINT ( 'NONE',  ( 15.49687500061451750, -3.027376345333614438, 5.243569643749998122 ) ) ;
#12123 = CARTESIAN_POINT ( 'NONE',  ( 23.06250000122903288, -4.330127018922190985, -2.500000000000001332 ) ) ;
#12124 = CARTESIAN_POINT ( 'NONE',  ( 15.77812500061451573, 4.541064518000418104, 2.621784821874999949 ) ) ;
#12125 = CARTESIAN_POINT ( 'NONE',  ( 29.16562500061451502, 3.027376345333613106, -5.243569643749998122 ) ) ;
#12126 = ORIENTED_EDGE ( 'NONE', *, *, #63735, .T. ) ;
#12127 = ORIENTED_EDGE ( 'NONE', *, *, #32319, .T. ) ;
#12128 = CARTESIAN_POINT ( 'NONE',  ( 17.55000000000000071, -4.330127018922190985, -2.500000000000001332 ) ) ;
#12129 = CARTESIAN_POINT ( 'NONE',  ( 22.18125000122903145, 6.123233995736764310E-16, -4.999999999999998224 ) ) ;
#12130 = CARTESIAN_POINT ( 'NONE',  ( 2.990625000614519191, -3.027376345333610441, -5.243569643749999898 ) ) ;
#12131 = CARTESIAN_POINT ( 'NONE',  ( 16.05000000122903359, 5.773502691896255534, 3.535250795749688894E-16 ) ) ;
#12132 = CARTESIAN_POINT ( 'NONE',  ( 20.84062500061451573, -3.027376345333614438, 5.243569643749998122 ) ) ;
#12133 =( BOUNDED_CURVE ( )  B_SPLINE_CURVE ( 2, ( #18297, #23854, #34947, #23495, #63734, #24216, #29764 ),
 .UNSPECIFIED., .F., .F. ) 
 B_SPLINE_CURVE_WITH_KNOTS ( ( 3, 2, 2, 3 ),
 ( 0.3199999999999999512, 0.3233333333333333059, 0.3266666666666666607, 0.3300000000000000711 ),
 .UNSPECIFIED. ) 
 CURVE ( )  GEOMETRIC_REPRESENTATION_ITEM ( )  RATIONAL_B_SPLINE_CURVE ( ( 1.000000000000002220, 0.8660254037844364872, 1.000000000000000000, 0.8660254037844387076, 1.000000000000000000, 0.8660254037844364872, 1.000000000000002220 ) ) 
 REPRESENTATION_ITEM ( '' )  );
#12134 = ADVANCED_FACE ( 'NONE', ( #54262 ), #31726, .F. ) ;
#12135 = CARTESIAN_POINT ( 'NONE',  ( 24.21562500061451573, 3.027376345333613106, -5.243569643749998122 ) ) ;
#12136 = CARTESIAN_POINT ( 'NONE',  ( 3.515625000614516882, 3.027376345333613106, -5.243569643749998122 ) ) ;
#12137 = CARTESIAN_POINT ( 'NONE',  ( 27.29999999999999716, 0.000000000000000000, 4.999999999999998224 ) ) ;
#12138 = CARTESIAN_POINT ( 'NONE',  ( 4.603329117574985752, 1.951758446961684434, -4.603329117574985752 ) ) ;
#12139 = CARTESIAN_POINT ( 'NONE',  ( 10.28437500061451715, 5.824947211148865298E-16, -4.756430356249998326 ) ) ;
#12140 = DIRECTION ( 'NONE',  ( -0.000000000000000000, -1.000000000000000000, -0.000000000000000000 ) ) ;
#12141 = CARTESIAN_POINT ( 'NONE',  ( 8.484601909799253346E-16, 12.12500000122903465, -25.38119784648299770 ) ) ;
#12142 = CARTESIAN_POINT ( 'NONE',  ( -2.121784821874999949, 15.28437500061451892, -33.67503911421598417 ) ) ;
#12143 = CARTESIAN_POINT ( 'NONE',  ( 5.550000001229032698, -2.886751345948125991, -5.000000000000000000 ) ) ;
#12144 = CARTESIAN_POINT ( 'NONE',  ( 7.762500000000001954, 2.886751345948129099, -4.999999999999998224 ) ) ;
#12145 = CARTESIAN_POINT ( 'NONE',  ( 4.500000001229034652, -2.886751345948129988, 4.999999999999997335 ) ) ;
#12146 = CARTESIAN_POINT ( 'NONE',  ( 8.971875000614515372, 3.027376345333613106, -5.243569643749998122 ) ) ;
#12147 = CARTESIAN_POINT ( 'NONE',  ( 4.171875000614517326, 3.027376345333611329, 5.243569643749999010 ) ) ;
#12148 = DIRECTION ( 'NONE',  ( -0.000000000000000000, -1.000000000000000000, -0.000000000000000000 ) ) ;
#12149 = DIRECTION ( 'NONE',  ( -1.000000000000000000, -0.000000000000000000, -0.000000000000000000 ) ) ;
#12150 = CARTESIAN_POINT ( 'NONE',  ( 7.959375000614516971, -4.541064518000417216, -2.621784821875001281 ) ) ;
#12151 = CARTESIAN_POINT ( 'NONE',  ( 12.64687500061451608, 6.054752690667223547, 3.707466751127219781E-16 ) ) ;
#12152 = CARTESIAN_POINT ( 'NONE',  ( 8.400000000000000355, 0.000000000000000000, 4.999999999999998224 ) ) ;
#12153 = CARTESIAN_POINT ( 'NONE',  ( 6.975000000000002309, 4.330127018922191873, 2.499999999999999556 ) ) ;
#12154 = CARTESIAN_POINT ( 'NONE',  ( 2.121784821874999061, 17.40312500061459744, 26.32496088578401583 ) ) ;
#12155 = CARTESIAN_POINT ( 'NONE',  ( 22.09687500061451715, 6.054752690667223547, 3.707466751127219781E-16 ) ) ;
#12156 = CARTESIAN_POINT ( 'NONE',  ( 26.06250000122903288, 0.000000000000000000, 4.999999999999998224 ) ) ;
#12157 = CARTESIAN_POINT ( 'NONE',  ( 17.63437500061451502, -2.746126346562646425, 4.756430356249996549 ) ) ;
#12158 = CARTESIAN_POINT ( 'NONE',  ( 23.46562500061451573, 3.027376345333611329, 5.243569643749999010 ) ) ;
#12159 = CARTESIAN_POINT ( 'NONE',  ( 16.49062500061451786, -3.027376345333610441, -5.243569643749999898 ) ) ;
#12160 = CARTESIAN_POINT ( 'NONE',  ( 26.55937500061451217, 2.746126346562643317, 4.756430356249998326 ) ) ;
#12161 = CARTESIAN_POINT ( 'NONE',  ( 12.90937500061451537, -4.541064518000417216, -2.621784821875001281 ) ) ;
#12162 = CARTESIAN_POINT ( 'NONE',  ( 28.46249999999999858, 2.886751345948129099, -4.999999999999998224 ) ) ;
#12163 = CARTESIAN_POINT ( 'NONE',  ( 25.23750000122903359, -4.330127018922194537, 2.499999999999995559 ) ) ;
#12164 = CARTESIAN_POINT ( 'NONE',  ( 26.92499999999999716, -4.330127018922194537, 2.499999999999995559 ) ) ;
#12165 = CARTESIAN_POINT ( 'NONE',  ( 11.74687500061451573, 6.054752690667223547, 3.707466751127219781E-16 ) ) ;
#12166 = CARTESIAN_POINT ( 'NONE',  ( 20.99999999999999645, 0.000000000000000000, 4.999999999999998224 ) ) ;
#12167 = CARTESIAN_POINT ( 'NONE',  ( 3.909375000614518481, -4.541064518000417216, -2.621784821875001281 ) ) ;
#12168 = EDGE_CURVE ( 'NONE', #11370, #21163, #37624, .T. ) ;
#12169 = CARTESIAN_POINT ( 'NONE',  ( 16.65000000122903501, -2.886751345948096681, 5.000000000000054179 ) ) ;
#12170 = CARTESIAN_POINT ( 'NONE',  ( 22.50937500061451857, 4.541064518000418104, -2.621784821874998173 ) ) ;
#12171 = CARTESIAN_POINT ( 'NONE',  ( 13.28437500061451715, -4.541064518000419881, 2.621784821874995952 ) ) ;
#12172 = CARTESIAN_POINT ( 'NONE',  ( 1.878215178125000495, 19.12812499938548427, 26.74683588394047007 ) ) ;
#12173 = CARTESIAN_POINT ( 'NONE',  ( 25.94999999999999929, 0.000000000000000000, 4.999999999999998224 ) ) ;
#12174 = CARTESIAN_POINT ( 'NONE',  ( 4.849326327477522014, 20.72494550184886819, 32.95932117208439394 ) ) ;
#12175 = CARTESIAN_POINT ( 'NONE',  ( 27.68437500061451573, -4.119189519843968306, 2.378215178124996054 ) ) ;
#12176 = CARTESIAN_POINT ( 'NONE',  ( 17.76562500061451644, -6.054752690667223547, -1.112240025338166033E-15 ) ) ;
#12177 = CARTESIAN_POINT ( 'NONE',  ( 7.012500000000001066, 2.886751345948126879, 4.999999999999999112 ) ) ;
#12178 = CARTESIAN_POINT ( 'NONE',  ( 1.071796769724491893, 13.49509619066136779, 33.99999999999999289 ) ) ;
#12179 =( BOUNDED_CURVE ( )  B_SPLINE_CURVE ( 2, ( #11352, #33870, #61948, #57120, #29065, #1001, #23508 ),
 .UNSPECIFIED., .F., .F. ) 
 B_SPLINE_CURVE_WITH_KNOTS ( ( 3, 2, 2, 3 ),
 ( 0.1499999999999999389, 0.1527777777777777624, 0.1555555555555555858, 0.1583333333333333814 ),
 .UNSPECIFIED. ) 
 CURVE ( )  GEOMETRIC_REPRESENTATION_ITEM ( )  RATIONAL_B_SPLINE_CURVE ( ( 1.000000000000002665, 0.8660254037844360431, 1.000000000000000000, 0.8660254037844387076, 1.000000000000000000, 0.8660254037844360431, 1.000000000000002665 ) ) 
 REPRESENTATION_ITEM ( '' )  );
#12180 = CARTESIAN_POINT ( 'NONE',  ( 14.81250000000000000, -5.773502691896255534, -1.060575238724906372E-15 ) ) ;
#12181 = CARTESIAN_POINT ( 'NONE',  ( 2.121784821875001281, 10.05312500061451608, 33.67503911421598417 ) ) ;
#12182 = CYLINDRICAL_SURFACE ( 'NONE', #64334, 4.999999999999998224 ) ;
#12183 = CARTESIAN_POINT ( 'NONE',  ( 26.74687500061451573, -3.027376345333614438, 5.243569643749998122 ) ) ;
#12184 = ORIENTED_EDGE ( 'NONE', *, *, #69324, .F. ) ;
#12185 = CARTESIAN_POINT ( 'NONE',  ( 21.40312500061451573, -4.541064518000417216, -2.621784821875001281 ) ) ;
#12186 = CARTESIAN_POINT ( 'NONE',  ( 20.93437500061451573, -4.541064518000419881, 2.621784821874995952 ) ) ;
#12187 = CARTESIAN_POINT ( 'NONE',  ( 4.349999999999999645, 0.000000000000000000, 4.999999999999998224 ) ) ;
#12188 = CARTESIAN_POINT ( 'NONE',  ( 6.065625000614516260, -6.054752690667223547, -1.112240025338166033E-15 ) ) ;
#12189 = CARTESIAN_POINT ( 'NONE',  ( 25.04062500061451502, -3.027376345333610441, -5.243569643749999898 ) ) ;
#12190 = CARTESIAN_POINT ( 'NONE',  ( 11.63437500061451857, 6.421520780324663323E-16, -5.243569643749999010 ) ) ;
#12191 = CARTESIAN_POINT ( 'NONE',  ( 16.92187500061451999, -6.054752690667223547, -1.112240025338166033E-15 ) ) ;
#12192 = CARTESIAN_POINT ( 'NONE',  ( 4.243569643749999898, 18.22812500061451502, 30.00000000000000000 ) ) ;
#12193 = CARTESIAN_POINT ( 'NONE',  ( 18.90000000122902790, -2.886751345948129988, 4.999999999999997335 ) ) ;
#12194 = CARTESIAN_POINT ( 'NONE',  ( 15.00937500061451679, 0.000000000000000000, 4.756430356249998326 ) ) ;
#12195 = CARTESIAN_POINT ( 'NONE',  ( 8.915625000614515017, 3.027376345333612662, -5.243569643749998122 ) ) ;
#12196 = CARTESIAN_POINT ( 'NONE',  ( 4.771875000614516971, -6.054752690667223547, -1.112240025338166033E-15 ) ) ;
#12197 = CARTESIAN_POINT ( 'NONE',  ( 4.509375000614518569, 4.541064518000418104, -2.621784821874998173 ) ) ;
#12198 = VERTEX_POINT ( 'NONE', #26552 ) ;
#12199 = CARTESIAN_POINT ( 'NONE',  ( 26.14687500061451431, 6.054752690667223547, 3.707466751127219781E-16 ) ) ;
#12200 = CARTESIAN_POINT ( 'NONE',  ( 17.24062500061451786, -3.027376345333614438, 5.243569643749998122 ) ) ;
#12201 = CARTESIAN_POINT ( 'NONE',  ( 28.35000000122903430, -2.886751345948129988, 4.999999999999997335 ) ) ;
#12202 = CARTESIAN_POINT ( 'NONE',  ( 27.17812500061451786, -4.541064518000419881, 2.621784821874995952 ) ) ;
#12203 = CARTESIAN_POINT ( 'NONE',  ( 21.15937500061451715, 4.541064518000418104, -2.621784821874998173 ) ) ;
#12204 = CARTESIAN_POINT ( 'NONE',  ( 17.01562500061451644, 3.027376345333613106, -5.243569643749998122 ) ) ;
#12205 = CARTESIAN_POINT ( 'NONE',  ( 4.243569643749999898, 16.44687500061451857, 32.45002607614398471 ) ) ;
#12206 = CARTESIAN_POINT ( 'NONE',  ( 21.40312500061451573, -4.541064518000417216, -2.621784821875001281 ) ) ;
#12207 = CARTESIAN_POINT ( 'NONE',  ( 30.00000000000000000, 0.000000000000000000, 4.999999999999998224 ) ) ;
#12208 = ORIENTED_EDGE ( 'NONE', *, *, #26195, .T. ) ;
#12209 = CARTESIAN_POINT ( 'NONE',  ( 28.31250000000000000, -5.773502691896255534, -1.060575238724906372E-15 ) ) ;
#12210 = CARTESIAN_POINT ( 'NONE',  ( -3.999999999999999556, 14.11249999999999893, -32.30940107675850470 ) ) ;
#12211 = CARTESIAN_POINT ( 'NONE',  ( -3.756430356250000102, 20.17812499938548143, 30.00000000000000000 ) ) ;
#12212 = CARTESIAN_POINT ( 'NONE',  ( 28.30312500061451431, 4.541064518000418104, -2.621784821874998173 ) ) ;
#12213 = CARTESIAN_POINT ( 'NONE',  ( 11.05312500061451608, -4.541064518000417216, -2.621784821875001281 ) ) ;
#12214 = CARTESIAN_POINT ( 'NONE',  ( 21.33750000122903145, 6.123233995736764310E-16, -4.999999999999998224 ) ) ;
#12215 = CARTESIAN_POINT ( 'NONE',  ( 28.04062500061451502, -3.027376345333614438, 5.243569643749998122 ) ) ;
#12216 = CARTESIAN_POINT ( 'NONE',  ( 28.31250000000000000, -5.773502691896255534, -1.060575238724906372E-15 ) ) ;
#12217 = ADVANCED_FACE ( 'NONE', ( #15446 ), #20256, .T. ) ;
#12218 = CARTESIAN_POINT ( 'NONE',  ( -3.999999999999999112, 18.31250000122903288, -30.00000000000000000 ) ) ;
#12219 = PLANE ( 'NONE',  #4353 ) ;
#12220 = CARTESIAN_POINT ( 'NONE',  ( 10.82812500061451644, 4.541064518000418104, 2.621784821874999949 ) ) ;
#12221 = ORIENTED_EDGE ( 'NONE', *, *, #29224, .T. ) ;
#12222 = CARTESIAN_POINT ( 'NONE',  ( 7.865625000614516971, -6.054752690667223547, -1.112240025338166033E-15 ) ) ;
#12223 = PRODUCT_DEFINITION_CONTEXT ( 'detailed design', #21462, 'design' ) ;
#12224 = CARTESIAN_POINT ( 'NONE',  ( 7.003125000614518036, -4.541064518000417216, -2.621784821875001281 ) ) ;
#12225 = CARTESIAN_POINT ( 'NONE',  ( 16.92187500061451999, -5.492252693125287522, -1.008910452111647106E-15 ) ) ;
#12226 = CARTESIAN_POINT ( 'NONE',  ( 21.22500000000000142, 6.123233995736764310E-16, -4.999999999999998224 ) ) ;
#12227 = CARTESIAN_POINT ( 'NONE',  ( 14.51250000000000107, 2.886751345948129099, -4.999999999999998224 ) ) ;
#12228 = CARTESIAN_POINT ( 'NONE',  ( 16.35937500061451644, 0.000000000000000000, 5.243569643749999010 ) ) ;
#12229 = CARTESIAN_POINT ( 'NONE',  ( 11.62500000122903465, 2.886751345948126879, 4.999999999999999112 ) ) ;
#12230 = CARTESIAN_POINT ( 'NONE',  ( 18.68437500061451928, -4.541064518000419881, 2.621784821874995952 ) ) ;
#12231 = CARTESIAN_POINT ( 'NONE',  ( 17.88749999999999929, -2.886751345948129988, 4.999999999999997335 ) ) ;
#12232 = CARTESIAN_POINT ( 'NONE',  ( 21.57187500061451502, 3.027376345333613106, -5.243569643749998122 ) ) ;
#12233 = CARTESIAN_POINT ( 'NONE',  ( -4.243569643749999898, 14.36562500061451786, -32.45002607614398471 ) ) ;
#12234 = CARTESIAN_POINT ( 'NONE',  ( 21.11250000122903359, 0.000000000000000000, 4.999999999999998224 ) ) ;
#12235 = CARTESIAN_POINT ( 'NONE',  ( 26.07187500061451146, 4.119189519843966529, 2.378215178124999607 ) ) ;
#12236 = CARTESIAN_POINT ( 'NONE',  ( 4.000000000000000000, 11.63750000000000284, -27.69059892324149885 ) ) ;
#12237 = CARTESIAN_POINT ( 'NONE',  ( 27.14062500061451644, -3.027376345333614438, 5.243569643749998122 ) ) ;
#12238 = CARTESIAN_POINT ( 'NONE',  ( 24.93750000000000000, 5.773502691896255534, 3.535250795749688401E-16 ) ) ;
#12239 = CARTESIAN_POINT ( 'NONE',  ( 28.88437500061451502, 4.541064518000418104, 2.621784821874999949 ) ) ;
#12240 = CARTESIAN_POINT ( 'NONE',  ( 23.62500000000000000, 4.330127018922191873, 2.499999999999999556 ) ) ;
#12241 = B_SPLINE_CURVE_WITH_KNOTS ( 'NONE', 3,
 ( #6095, #66331, #34158, #55255, #61511, #67795, #49714, #72972, #4651, #38629 ),
 .UNSPECIFIED., .F., .F.,
 ( 4, 3, 3, 4 ),
 ( 6.133173666733496745E-19, 7.861287778095982833E-05, 0.0001572259190930990044, 0.0002915343808913384120 ),
 .UNSPECIFIED. ) ;
#12242 = CARTESIAN_POINT ( 'NONE',  ( 7.378125000614518036, -4.541064518000419881, 2.621784821874995952 ) ) ;
#12243 = CARTESIAN_POINT ( 'NONE',  ( 23.74687500061451573, 4.119189519843966529, -2.378215178124998275 ) ) ;
#12244 = CARTESIAN_POINT ( 'NONE',  ( 19.73437500061451644, 6.421520780324663323E-16, -5.243569643749999010 ) ) ;
#12245 = CARTESIAN_POINT ( 'NONE',  ( 10.05937500061451750, -5.492252693125287522, -1.008910452111647106E-15 ) ) ;
#12246 = CARTESIAN_POINT ( 'NONE',  ( 4.678125000614516971, -4.541064518000419881, 2.621784821874995952 ) ) ;
#12247 = CARTESIAN_POINT ( 'NONE',  ( 8.859375000614518214, -4.541064518000417216, -2.621784821875001281 ) ) ;
#12248 = VERTEX_POINT ( 'NONE', #42081 ) ;
#12249 = CARTESIAN_POINT ( 'NONE',  ( 20.14687500061451786, -3.027376345333610441, -5.243569643749999898 ) ) ;
#12250 = CARTESIAN_POINT ( 'NONE',  ( 13.91250000122903252, 0.000000000000000000, 4.999999999999998224 ) ) ;
#12251 = CARTESIAN_POINT ( 'NONE',  ( 28.19999999999999929, 0.000000000000000000, 4.999999999999998224 ) ) ;
#12252 = CARTESIAN_POINT ( 'NONE',  ( 3.000000000000002665, 0.000000000000000000, 4.999999999999998224 ) ) ;
#12253 = CARTESIAN_POINT ( 'NONE',  ( 26.26875000122903003, 2.886751345948129099, -4.999999999999997335 ) ) ;
#12254 = CARTESIAN_POINT ( 'NONE',  ( 34.99999999999999289, 0.000000000000000000, 0.000000000000000000 ) ) ;
#12255 = VERTEX_POINT ( 'NONE', #42808 ) ;
#12256 = CARTESIAN_POINT ( 'NONE',  ( 10.80000000000000071, -4.330127018922190985, -2.500000000000001332 ) ) ;
#12257 = CARTESIAN_POINT ( 'NONE',  ( 11.55937500061451573, 2.746126346562645981, -4.756430356249997438 ) ) ;
#12258 = CARTESIAN_POINT ( 'NONE',  ( 24.89062500061451644, -3.027376345333614438, 5.243569643749998122 ) ) ;
#12259 = CARTESIAN_POINT ( 'NONE',  ( 13.87500000000000178, -4.330127018922194537, 2.499999999999995559 ) ) ;
#12260 = EDGE_CURVE ( 'NONE', #8633, #25827, #53155, .T. ) ;
#12261 = CARTESIAN_POINT ( 'NONE',  ( 11.70000000122903216, -2.886751345948129988, 4.999999999999997335 ) ) ;
#12262 = CARTESIAN_POINT ( 'NONE',  ( 9.253125000614517148, -4.541064518000417216, -2.621784821875001281 ) ) ;
#12263 = CARTESIAN_POINT ( 'NONE',  ( 23.25000000000000000, 0.000000000000000000, 4.999999999999998224 ) ) ;
#12264 = CARTESIAN_POINT ( 'NONE',  ( 21.85312500061451502, -4.541064518000417216, -2.621784821875001281 ) ) ;
#12265 = CYLINDRICAL_SURFACE ( 'NONE', #31328, 4.999999999999998224 ) ;
#12266 = CARTESIAN_POINT ( 'NONE',  ( 27.71250000122903145, 4.330127018922192761, -2.499999999999997780 ) ) ;
#12267 = CARTESIAN_POINT ( 'NONE',  ( 3.756430356250000546, 17.17812499938548498, 27.83122392262697886 ) ) ;
#12268 = CARTESIAN_POINT ( 'NONE',  ( 6.862500000000002487, 2.886751345948129099, -4.999999999999998224 ) ) ;
#12269 = VERTEX_POINT ( 'NONE', #13990 ) ;
#12270 = CARTESIAN_POINT ( 'NONE',  ( 21.74062500061451431, -3.027376345333614438, 5.243569643749998122 ) ) ;
#12271 = CARTESIAN_POINT ( 'NONE',  ( 28.11562500061451431, -6.054752690667223547, -1.112240025338166033E-15 ) ) ;
#12272 = DIRECTION ( 'NONE',  ( -1.000000000000000000, -0.000000000000000000, -0.000000000000000000 ) ) ;
#12273 = CARTESIAN_POINT ( 'NONE',  ( 18.68437500061451928, -4.541064518000419881, 2.621784821874995952 ) ) ;
#12274 = CARTESIAN_POINT ( 'NONE',  ( 14.61562500061451608, -6.054752690667223547, -1.112240025338166033E-15 ) ) ;
#12275 = DIRECTION ( 'NONE',  ( 1.000000000000000000, 0.000000000000000000, 0.000000000000000000 ) ) ;
#12276 = CARTESIAN_POINT ( 'NONE',  ( 26.40000000122902790, 5.773502691896255534, 3.535250795749688894E-16 ) ) ;
#12277 = CARTESIAN_POINT ( 'NONE',  ( 22.50937500061451857, 4.119189519843966529, -2.378215178124998275 ) ) ;
#12278 = CARTESIAN_POINT ( 'NONE',  ( 16.04062500061451857, -3.027376345333610441, -5.243569643749999898 ) ) ;
#12279 = CARTESIAN_POINT ( 'NONE',  ( 4.312500001229034652, 4.330127018922192761, -2.499999999999997780 ) ) ;
#12280 = CARTESIAN_POINT ( 'NONE',  ( 12.00937500061451857, -4.541064518000417216, -2.621784821875001281 ) ) ;
#12281 = CARTESIAN_POINT ( 'NONE',  ( 12.27187500061451786, 3.027376345333611329, 5.243569643749999010 ) ) ;
#12282 = CARTESIAN_POINT ( 'NONE',  ( 19.28437500061451360, 6.421520780324663323E-16, -5.243569643749999010 ) ) ;
#12283 = ORIENTED_EDGE ( 'NONE', *, *, #24627, .T. ) ;
#12284 = CARTESIAN_POINT ( 'NONE',  ( -5.378075516623670893, 8.432637420806665673, 32.68862326928266526 ) ) ;
#12285 = CARTESIAN_POINT ( 'NONE',  ( 25.15312500061451217, 4.541064518000418104, -2.621784821874998173 ) ) ;
#12286 = CARTESIAN_POINT ( 'NONE',  ( 18.79687500061451644, -3.027376345333610441, -5.243569643749999898 ) ) ;
#12287 = CARTESIAN_POINT ( 'NONE',  ( 25.49062500061451786, -3.027376345333610441, -5.243569643749999898 ) ) ;
#12288 = CARTESIAN_POINT ( 'NONE',  ( 30.00000000000000000, 0.000000000000000000, 4.999999999999998224 ) ) ;
#12289 = CARTESIAN_POINT ( 'NONE',  ( 3.999999999999999112, 16.17500000000000071, 30.00000000000000000 ) ) ;
#12290 = AXIS2_PLACEMENT_3D ( 'NONE', #71861, #61491, #56324 ) ;
#12291 = CARTESIAN_POINT ( 'NONE',  ( 28.71562500061451573, 3.027376345333613106, -5.243569643749998122 ) ) ;
#12292 = CARTESIAN_POINT ( 'NONE',  ( 10.68750000122903288, 4.330127018922191873, 2.499999999999999556 ) ) ;
#12293 = CARTESIAN_POINT ( 'NONE',  ( 5.812500001229035540, 0.000000000000000000, 4.999999999999998224 ) ) ;
#12294 = CARTESIAN_POINT ( 'NONE',  ( 3.999999999999998668, 19.81250000000000000, -32.30940107675850470 ) ) ;
#12295 = CARTESIAN_POINT ( 'NONE',  ( 26.96250000122903145, 0.000000000000000000, 4.999999999999998224 ) ) ;
#12296 = CARTESIAN_POINT ( 'NONE',  ( 2.828200636599751609E-16, 19.30624999877096570, 25.38119784648299415 ) ) ;
#12297 = CARTESIAN_POINT ( 'NONE',  ( 16.25625000122903074, -4.330127018922190985, -2.500000000000001332 ) ) ;
#12298 = CARTESIAN_POINT ( 'NONE',  ( 9.084375000614517859, 4.541064518000418104, 2.621784821874999949 ) ) ;
#12299 = CARTESIAN_POINT ( 'NONE',  ( 17.12812500061451715, 4.541064518000418104, 2.621784821874999949 ) ) ;
#12300 = CARTESIAN_POINT ( 'NONE',  ( 10.80937500061451928, 4.541064518000418104, -2.621784821874998173 ) ) ;
#12301 = CARTESIAN_POINT ( 'NONE',  ( 3.328125000614516438, -4.541064518000419881, 2.621784821874995952 ) ) ;
#12302 = CARTESIAN_POINT ( 'NONE',  ( 19.92187500061451644, 3.027376345333611329, 5.243569643749999010 ) ) ;
#12303 = CARTESIAN_POINT ( 'NONE',  ( 7.884375000614517681, -4.541064518000419881, 2.621784821874995952 ) ) ;
#12304 = CARTESIAN_POINT ( 'NONE',  ( 3.021917804904423743, -3.983467431823952687, -3.409840147052992432 ) ) ;
#12305 = CARTESIAN_POINT ( 'NONE',  ( 10.87500000000000000, 6.123233995736764310E-16, -4.999999999999998224 ) ) ;
#12306 = CARTESIAN_POINT ( 'NONE',  ( 8.578125000614518214, 4.541064518000418104, 2.621784821874999949 ) ) ;
#12307 = CARTESIAN_POINT ( 'NONE',  ( 18.25312500061451715, -4.541064518000417216, -2.621784821875001281 ) ) ;
#12308 = EDGE_CURVE ( 'NONE', #49458, #72969, #42188, .T. ) ;
#12309 = EDGE_LOOP ( 'NONE', ( #59894, #58264, #4369, #22558 ) ) ;
#12310 = CARTESIAN_POINT ( 'NONE',  ( 6.037500001229035185, 6.123233995736764310E-16, -4.999999999999998224 ) ) ;
#12311 = CARTESIAN_POINT ( 'NONE',  ( 14.16562500061451679, -6.054752690667223547, -1.112240025338166033E-15 ) ) ;
#12312 = CARTESIAN_POINT ( 'NONE',  ( 12.62812500061451537, 4.541064518000418104, 2.621784821874999949 ) ) ;
#12313 = CARTESIAN_POINT ( 'NONE',  ( 24.12187500061451217, -5.492252693125287522, -1.008910452111647106E-15 ) ) ;
#12314 = CARTESIAN_POINT ( 'NONE',  ( 13.46249999999999858, -5.773502691896255534, -1.060575238724906372E-15 ) ) ;
#12315 = CARTESIAN_POINT ( 'NONE',  ( 7.875000001229034652, 2.886751345948129099, -4.999999999999998224 ) ) ;
#12316 = CARTESIAN_POINT ( 'NONE',  ( 5.803125000614517859, 4.541064518000418104, -2.621784821874998173 ) ) ;
#12317 = CARTESIAN_POINT ( 'NONE',  ( 18.15000000122903501, -2.886751345948125991, -5.000000000000000000 ) ) ;
#12318 = CARTESIAN_POINT ( 'NONE',  ( 25.64999999999999858, -4.330127018922190985, -2.500000000000001332 ) ) ;
#12319 = CARTESIAN_POINT ( 'NONE',  ( -2.121784821874999949, 10.78437500061451715, -33.67503911421598417 ) ) ;
#12320 = CARTESIAN_POINT ( 'NONE',  ( -2.000000000000001776, 14.54374999877096641, 33.46410161513775705 ) ) ;
#12321 = CARTESIAN_POINT ( 'NONE',  ( 2.962500001229034119, 4.330127018922192761, -2.499999999999997780 ) ) ;
#12322 = CARTESIAN_POINT ( 'NONE',  ( 26.17500000000000071, 6.123233995736764310E-16, -4.999999999999998224 ) ) ;
#12323 = CARTESIAN_POINT ( 'NONE',  ( 17.89687500061451431, -3.027376345333610441, -5.243569643749999898 ) ) ;
#12324 = CARTESIAN_POINT ( 'NONE',  ( 21.48750000122903003, 4.330127018922191873, 2.499999999999999556 ) ) ;
#12325 = CARTESIAN_POINT ( 'NONE',  ( 12.96562500061451750, 3.027376345333613106, -5.243569643749998122 ) ) ;
#12326 = CARTESIAN_POINT ( 'NONE',  ( 8.643750001229031810, -2.886751345948125991, -5.000000000000000000 ) ) ;
#12327 = LINE ( 'NONE', #40786, #14107 ) ;
#12328 = CARTESIAN_POINT ( 'NONE',  ( 26.37187500061451217, -6.054752690667223547, -1.112240025338166033E-15 ) ) ;
#12329 = CARTESIAN_POINT ( 'NONE',  ( 17.55937500061451573, 2.746126346562643317, 4.756430356249998326 ) ) ;
#12330 = VECTOR ( 'NONE', #1342, 1000.000000000000000 ) ;
#12331 = CARTESIAN_POINT ( 'NONE',  ( 12.70312500061451821, 0.000000000000000000, 5.243569643749999010 ) ) ;
#12332 = CARTESIAN_POINT ( 'NONE',  ( 11.82187500061451679, 3.027376345333611329, 5.243569643749999010 ) ) ;
#12333 = VERTEX_POINT ( 'NONE', #19894 ) ;
#12334 = CARTESIAN_POINT ( 'NONE',  ( 29.72812500061451502, 4.541064518000418104, 2.621784821874999949 ) ) ;
#12335 = CARTESIAN_POINT ( 'NONE',  ( 20.09062500061451573, -3.027376345333610441, -5.243569643749999898 ) ) ;
#12336 = CARTESIAN_POINT ( 'NONE',  ( 29.35312500061451502, 0.000000000000000000, 5.243569643749999010 ) ) ;
#12337 = CARTESIAN_POINT ( 'NONE',  ( 1.626862140677534273E-15, 10.66249999999999964, 34.00000000000000000 ) ) ;
#12338 = CARTESIAN_POINT ( 'NONE',  ( 9.150000000000002132, 4.330127018922192761, -2.499999999999997780 ) ) ;
#12339 = CARTESIAN_POINT ( 'NONE',  ( 20.28750000122903074, -4.330127018922194537, 2.499999999999995559 ) ) ;
#12340 = CARTESIAN_POINT ( 'NONE',  ( -2.000000000000000000, 10.02500000000000036, 26.53589838486224650 ) ) ;
#12341 = CARTESIAN_POINT ( 'NONE',  ( 11.44687500061451679, -4.119189519843965641, -2.378215178125001383 ) ) ;
#12342 = EDGE_LOOP ( 'NONE', ( #67886, #54651, #60398, #22071 ) ) ;
#12343 = CARTESIAN_POINT ( 'NONE',  ( 17.84999999999999787, 0.000000000000000000, 4.999999999999998224 ) ) ;
#12344 = CARTESIAN_POINT ( 'NONE',  ( 21.63749999999999929, -2.886751345948125991, -5.000000000000000000 ) ) ;
#12345 = CARTESIAN_POINT ( 'NONE',  ( 19.13437500061451857, -4.541064518000419881, 2.621784821874995952 ) ) ;
#12346 = CARTESIAN_POINT ( 'NONE',  ( 24.32812500061451289, 4.541064518000418104, 2.621784821874999949 ) ) ;
#12348 = EDGE_LOOP ( 'NONE', ( #63772, #22123, #30355, #24597 ) ) ;
#12347 = VECTOR ( 'NONE', #41962, 1000.000000000000000 ) ;
#12349 = CARTESIAN_POINT ( 'NONE',  ( -2.000000000000000000, 16.88750000122903572, 26.53589838486224650 ) ) ;
#12350 = CARTESIAN_POINT ( 'NONE',  ( 8.390625000614518214, -3.027376345333610441, -5.243569643749999898 ) ) ;
#12351 = CARTESIAN_POINT ( 'NONE',  ( -4.000000000000000000, 18.96874999877096357, 30.00000000000000000 ) ) ;
#12352 = CARTESIAN_POINT ( 'NONE',  ( 14.28750000000000142, -2.886751345948129988, 4.999999999999997335 ) ) ;
#12353 = CARTESIAN_POINT ( 'NONE',  ( -3.000416591977282496E-16, 18.34062500061451928, 25.09994784771203058 ) ) ;
#12354 = CARTESIAN_POINT ( 'NONE',  ( 3.084375000614519191, 6.421520780324663323E-16, -5.243569643749999010 ) ) ;
#12355 = CARTESIAN_POINT ( 'NONE',  ( 10.76250000000000107, -5.773502691896255534, -1.060575238724906372E-15 ) ) ;
#12356 = VECTOR ( 'NONE', #39967, 1000.000000000000000 ) ;
#12357 = CARTESIAN_POINT ( 'NONE',  ( 3.756430356250000102, 13.99062499938548498, 30.00000000000000000 ) ) ;
#12358 = CARTESIAN_POINT ( 'NONE',  ( 25.47187500061451715, -6.054752690667223547, -1.112240025338166033E-15 ) ) ;
#12359 = ORIENTED_EDGE ( 'NONE', *, *, #63501, .T. ) ;
#12360 = CARTESIAN_POINT ( 'NONE',  ( 24.59062500061451573, -3.027376345333610441, -5.243569643749999898 ) ) ;
#12361 = CARTESIAN_POINT ( 'NONE',  ( 23.33437500061451786, 6.421520780324663323E-16, -5.243569643749999010 ) ) ;
#12362 = CARTESIAN_POINT ( 'NONE',  ( 4.243569643749999010, 16.46562500061459389, -32.45002607614398471 ) ) ;
#12363 = CARTESIAN_POINT ( 'NONE',  ( 10.65000000000000036, 0.000000000000000000, 4.999999999999998224 ) ) ;
#12364 = CARTESIAN_POINT ( 'NONE',  ( 7.978125000614517681, 6.421520780324663323E-16, -5.243569643749999010 ) ) ;
#12365 = CARTESIAN_POINT ( 'NONE',  ( 15.15000000000000036, 0.000000000000000000, 4.999999999999998224 ) ) ;
#12366 = CARTESIAN_POINT ( 'NONE',  ( 28.19062500061451715, -3.027376345333610441, -5.243569643749999898 ) ) ;
#12367 = CARTESIAN_POINT ( 'NONE',  ( 26.61562500061451786, 3.027376345333611329, 5.243569643749999010 ) ) ;
#12368 = CARTESIAN_POINT ( 'NONE',  ( 28.32187500061451502, 4.119189519843966529, 2.378215178124999607 ) ) ;
#12369 = CARTESIAN_POINT ( 'NONE',  ( 13.58437500061451786, 4.119189519843966529, 2.378215178124999607 ) ) ;
#12370 = CARTESIAN_POINT ( 'NONE',  ( 18.87187500061451573, 3.027376345333613106, -5.243569643749998122 ) ) ;
#12371 = CARTESIAN_POINT ( 'NONE',  ( -4.243569643749999898, 11.75937500061451857, 30.00000000000000000 ) ) ;
#12372 = CARTESIAN_POINT ( 'NONE',  ( 18.27187500061451431, -6.054752690667223547, -1.112240025338166033E-15 ) ) ;
#12373 = CARTESIAN_POINT ( 'NONE',  ( 27.00937500061451857, 4.541064518000418104, -2.621784821874998173 ) ) ;
#12374 = CARTESIAN_POINT ( 'NONE',  ( 9.001249775931846008E-16, 17.27187500061451786, 34.90005215228797653 ) ) ;
#12375 = CARTESIAN_POINT ( 'NONE',  ( 8.053125000614516082, 4.541064518000418104, -2.621784821874998173 ) ) ;
#12376 = CARTESIAN_POINT ( 'NONE',  ( -2.000000000000000000, 18.12500000000000355, -33.46410161513775705 ) ) ;
#12377 = CARTESIAN_POINT ( 'NONE',  ( 3.496875000614518836, -3.027376345333610441, -5.243569643749999898 ) ) ;
#12378 = CARTESIAN_POINT ( 'NONE',  ( 6.103125000614515905, -4.541064518000417216, -2.621784821875001281 ) ) ;
#12379 = CARTESIAN_POINT ( 'NONE',  ( 9.459375000614517859, 4.541064518000418104, -2.621784821874998173 ) ) ;
#12380 = PRESENTATION_STYLE_ASSIGNMENT (( #61906 ) ) ;
#12381 = CARTESIAN_POINT ( 'NONE',  ( 17.17500000122903359, -5.773502691896255534, -1.060575238724906372E-15 ) ) ;
#12382 = CARTESIAN_POINT ( 'NONE',  ( 6.346875000614517148, 6.054752690667223547, 3.707466751127219781E-16 ) ) ;
#12383 = CARTESIAN_POINT ( 'NONE',  ( 8.540625000614518569, 6.054752690667223547, 3.707466751127219781E-16 ) ) ;
#12384 = CARTESIAN_POINT ( 'NONE',  ( -3.486133158594716510E-16, 12.61250000000000426, 26.00000000000000355 ) ) ;
#12385 = CARTESIAN_POINT ( 'NONE',  ( 24.13125000122903074, 4.330127018922191873, 2.499999999999999556 ) ) ;
#12386 = CARTESIAN_POINT ( 'NONE',  ( 17.10937500061451999, 4.541064518000418104, -2.621784821874998173 ) ) ;
#12387 = CARTESIAN_POINT ( 'NONE',  ( 2.393811435568372112E-14, 19.08124999877097139, 34.00000000000000000 ) ) ;
#12388 = EDGE_LOOP ( 'NONE', ( #68168, #31151, #10326, #71463 ) ) ;
#12389 = CARTESIAN_POINT ( 'NONE',  ( 23.42812500061451786, 4.541064518000418104, 2.621784821874999949 ) ) ;
#12390 = CARTESIAN_POINT ( 'NONE',  ( 9.665625000614515017, -6.054752690667223547, -1.112240025338166033E-15 ) ) ;
#12391 = CARTESIAN_POINT ( 'NONE',  ( 27.23437500061451644, -4.541064518000419881, 2.621784821874995952 ) ) ;
#12392 = CARTESIAN_POINT ( 'NONE',  ( 10.19062500061451892, -3.027376345333610441, -5.243569643749999898 ) ) ;
#12393 = CARTESIAN_POINT ( 'NONE',  ( 0.000000000000000000, 20.00000000000000000, 30.00000000000000000 ) ) ;
#12394 = CARTESIAN_POINT ( 'NONE',  ( 10.76250000122903572, 0.000000000000000000, 4.999999999999998224 ) ) ;
#12395 = CARTESIAN_POINT ( 'NONE',  ( 26.84062500061451573, -3.027376345333610441, -5.243569643749999898 ) ) ;
#12396 = EDGE_CURVE ( 'NONE', #427, #11359, #46938, .T. ) ;
#12397 = CARTESIAN_POINT ( 'NONE',  ( -4.243569643749999898, 13.95312500061451821, -30.00000000000000000 ) ) ;
#12398 = CARTESIAN_POINT ( 'NONE',  ( 12.37500000122903465, 2.886751345948129099, -4.999999999999998224 ) ) ;
#12399 = CARTESIAN_POINT ( 'NONE',  ( 22.94062500061451715, 6.054752690667223547, 3.707466751127219781E-16 ) ) ;
#12400 = CIRCLE ( 'NONE', #26595, 1.500000000000000222 ) ;
#12401 = CARTESIAN_POINT ( 'NONE',  ( 10.31250000000000355, -5.773502691896255534, -1.060575238724906372E-15 ) ) ;
#12402 = CARTESIAN_POINT ( 'NONE',  ( 21.29062500061451502, -3.027376345333614438, 5.243569643749998122 ) ) ;
#12403 = CARTESIAN_POINT ( 'NONE',  ( 6.234375000614519102, 6.421520780324663323E-16, -5.243569643749999010 ) ) ;
#12404 = CARTESIAN_POINT ( 'NONE',  ( 20.17499999999999716, -4.330127018922194537, 2.499999999999995559 ) ) ;
#12405 = CARTESIAN_POINT ( 'NONE',  ( 7.200000001229035718, -2.886751345948129988, 4.999999999999997335 ) ) ;
#12406 = CARTESIAN_POINT ( 'NONE',  ( 15.71250000122903501, 0.000000000000000000, 4.999999999999998224 ) ) ;
#12407 = VECTOR ( 'NONE', #15591, 1000.000000000000000 ) ;
#12408 = CARTESIAN_POINT ( 'NONE',  ( 12.21562500061451573, 3.027376345333611329, 5.243569643749999010 ) ) ;
#12409 = CARTESIAN_POINT ( 'NONE',  ( 15.44062500061451537, -3.027376345333614438, 5.243569643749998122 ) ) ;
#12410 =( BOUNDED_SURFACE ( )  B_SPLINE_SURFACE ( 1, 2, ( 
 ( #1045, #19088, #40559, #12480, #62358, #30560, #42012, #36097, #54193, #9122, #25750, #13926, #3957, #15019, #9490, #20549, #37557, #32019, #59715, #47548, #36464, #31659, #71176, #36828, #58980, #20186, #48287, #58617, #8753, #70811, #25376, #42741, #65261, #3590, #64900, #26112, #31286, #26480, #47921, #48651, #14290, #43106, #19826, #60079, #14650, #65632, #49021, #8024, #54555, #37191, #8387, #53087, #59342, #2481, #64162, #71551, #41643, #70450, #42378, #13550, #25006, #19452, #70077, #64532, #30916, #53828, #53457, #2847, #3221, #5408, #38284, #55291, #60812, #54921, #10220, #73004, #27215, #32754, #39392, #61911, #11316, #10585, #20925, #44937, #44583, #15382, #32381, #4685, #43477, #33837, #56379, #27945, #5046, #5771, #50837, #38667, #15745, #33112, #49750, #28302, #61191, #55650, #16472, #72278, #66001, #27582, #50478, #21655, #22026, #39030, #67475, #4329, #21290, #10946, #67115, #37924, #50114, #22388, #66745, #26853, #72643, #16838, #44213, #60442, #16115, #9852, #49385, #61544, #33468, #56015, #71916, #43843, #66370, #24188, #23826, #46742, #57082, #29740, #34191, #17912, #52277, #17558, #35640, #46017, #62280, #39763, #12385, #40475, #68554, #57802, #23105, #11675, #69276, #46377, #18638, #6490, #1679, #57448, #45662, #58162, #41202, #63710, #13102, #7566, #30102, #18269, #6127, #68195, #63360, #237, #62990, #40119, #51920, #6852, #67829, #34921, #29386, #29025, #1317, #68911, #40842, #23471, #35280, #12744, #22745, #51561, #7211, #45295, #17202, #961, #56725, #28658, #51197, #600, #62634, #12029, #34554, #24914, #69632, #25281, #18994, #2043, #71087, #65544, #58889, #8299, #48194, #48561, #30470, #20461, #9401, #70717, #30829, #47457, #52999, #13455, #37097, #69990, #13834, #19360, #36003, #41917, #31566, #53362, #64442, #43015, #14931, #37471, #42284, #52637, #3503, #3129, #47100, #64073, #36373, #24554, #59991, #41556, #59622, #36733, #58522, #7932, #70357, #2759, #64808, #47827, #2394, #19734, #14198, #20092, #59255, #8663, #31194, #9036, #53736, #25658, #42649, #26022, #65173, #14564, #54105, #33024, #39306, #16026, #10853, #4597, #26764, #10496, #38574, #26389, #72189, #61098, #15655, #55562, #4958, #72550, #55204, #67026, #21568, #67387, #38194, #21937, #27127, #50025, #10131, #27861, #27491, #16386, #16749, #71460, #50392, #44493, #4237, #48931, #49661, #20836, #54468, #72917, #44851, #60721, #32663, #38941, #22299, #9761, #61819, #31931, #61459, #44122, #49296, #32295, #65913, #33387, #71829, #66277, #21200, #15293, #43752, #55923, #66649, #5319, #3866, #43389, #37832, #60352, #54830, #1231, #45928, #5683, #151, #6039, #11224, #18183, #63267, #6764, #51470, #40752, #33748, #34467, #56644, #28934, #23017, #12659, #56995, #6402, #40383, #507, #56293, #873, #51828, #40032, #62902, #34832, #68826, #17113, #28573, #29298, #12297, #28219, #68460, #35194, #23380, #62192, #17822, #50748, #45575, #22657, #57358, #11588, #34105, #23737, #46285, #45207, #67740, #68106, #51110, #39672, #17472, #62545, #11942, #33604, #61319, #49520, #39524, #50608, #45066, #56148, #12, #67603, #22160, #9988, #72045, #67248, #5542, #72406, #50253, #71690, #66879, #62050, #43980, #28080, #66135, #44712, #4093, #21788, #60951, #32523, #16606, #21062, #15513, #22519, #38803, #26622, #49159, #44354, #55060, #16247, #38055, #21423, #43613, #4461, #26991, #49881, #10716, #10354, #66501, #61677, #33248, #15883, #11076, #16968, #4817, #38428, #55424, #55786, #5177, #39162, #32884, #27713, #60580, #27350, #72776, #11445, #33965, #16057, #44882, #15687, #61489, #50422, #4988, #72948, #22330, #61850, #44525, #56322, #10886, #56672, #27520, #11257, #67058, #39337, #72583, #17145, #67417, #5711, #6070, #60755, #39703, #16779, #66682, #38225, #16417, #10163, #43783, #62221, #34134, #50054, #21967, #33779, #11617, #72221, #28603, #51139, #28247, #38973, #38606, #21599, #55234, #50778, #61131, #55593, #10526, #4629, #33054, #181, #33415, #55954, #21231, #66310, #32697, #5350, #27159, #45237, #22686, #49693, #44153, #27889, #67770, #41499, #13398, #7512, #57748, #64020, #30416, #18213, #68492, #12690, #57389, #35946, #40785, #63298, #69222, #34862, #62577, #904, #68138, #13047, #41148, #35586, #23049, #30043, #45959, #11974, #18583, #23412, #34497, #52583, #7880, #40416, #538, #46684, #17502, #35227, #58467, #62933, #1989, #57025, #63656, #45605, #7155, #6796, #28966, #58105, #40063, #6431, #24500, #29685, #51504, #17856, #68856, #12326, #52222, #29330, #51860, #1262, #23769, #46321, #1626, #24134, #47044, #69578, #18940, #25601, #70303, #59939, #20778, #53678, #47767, #31137, #14510, #54054, #20410, #59200, #59567, #41858, #69935, #24858, #15239, #54413, #26335, #8608, #42594, #14877, #42958, #52944, #25967, #43335, #9346, #70663, #3072, #48508, #8980 ),
 ( #48139, #47405, #31513, #30775, #71035, #65857, #31879, #3814, #71404, #19676, #37416, #8245, #64754, #20039, #48874, #19305, #53306, #64388, #65120, #65487, #14144, #37776, #60296, #9707, #13778, #36320, #37043, #25221, #3449, #2705, #2341, #42229, #58835, #36679, #72863, #55509, #67333, #72492, #67685, #38518, #22246, #4902, #50339, #10439, #28166, #61404, #16693, #17056, #71776, #50693, #5259, #4544, #49242, #27438, #21145, #54774, #95, #45153, #61041, #32969, #27803, #22601, #10077, #39615, #62134, #44800, #49968, #27073, #32608, #66220, #39251, #49604, #66591, #72131, #15598, #21511, #11167, #21877, #44064, #32241, #4179, #26708, #44438, #43699, #56236, #55872, #38140, #60664, #15968, #55146, #66967, #16332, #61763, #38887, #10799, #33334, #33691, #5629, #23684, #68406, #24412, #29244, #51776, #7071, #45873, #18857, #1176, #69138, #40328, #12608, #29600, #35500, #45518, #11887, #1539, #35142, #41418, #68772, #63576, #57306, #68049, #46232, #12963, #28875, #46961, #6711, #449, #51053, #18128, #40694, #63212, #18497, #34412, #22958, #58020, #57665, #7430, #17768, #41062, #52136, #56940, #69497, #29956, #52497, #1907, #11527, #34048, #24049, #17418, #6344, #46596, #56588, #5984, #39977, #51414, #28514, #62489, #816, #23324, #62849, #12243, #34774, #63934, #14789, #14424, #58381, #2260, #53218, #13319, #31793, #3725, #70950, #48056, #54332, #20689, #8522, #58748, #2983, #47677, #26250, #31051, #53588, #59481, #25136, #71313, #25511, #48424, #19587, #65033, #8893, #37330, #24774, #64301, #53965, #36959, #35858, #70581, #42875, #36594, #47318, #19957, #65398, #8158, #48787, #59115, #52860, #30331, #42509, #31425, #3363, #20321, #13690, #69851, #59854, #25884, #9258, #70213, #7793, #19218, #36234, #41772, #30687, #2615, #42143, #64670, #14055, #61316, #49156, #15510, #33245, #72773, #37687, #4090, #38052, #66876, #60210, #10351, #72403, #26988, #21785, #44351, #10713, #66498, #5174, #32881, #5539, #49517, #55783, #15880, #27710, #21420, #39159, #16244, #50250, #28077, #9623, #61674, #38800, #60577, #32155, #38425, #54688, #65768, #11073, #56145, #72042, #43977, #22157, #33601, #21059, #50605, #9, #44709, #60948, #9984, #43610, #26619, #67245, #32520, #4458, #55057, #71687, #55421, #16603, #4814, #27347, #43248, #15150, #66132, #49878, #18410, #68687, #67959, #39521, #68324, #62047, #45063, #40976, #35412, #28786, #51327, #18047, #63491, #360, #12879, #52410, #40605, #729, #17332, #22867, #56501, #6985, #39891, #56852, #62404, #5894, #11803, #1455, #23238, #34320, #57937, #7344, #29874, #12157, #22516, #46509, #46147, #16965, #33962, #6258, #67600, #11442, #28427, #29516, #6629, #50964, #45425, #40245, #45789, #34685, #17684, #62766, #57216, #29158, #63126, #51690, #1094, #23602, #52051, #12522, #35055, #57582, #69048, #23961, #2174, #64944, #2891, #9166, #59026, #53874, #47593, #35773, #19500, #3266, #19132, #37238, #70122, #63844, #41334, #13968, #42057, #64580, #59388, #24687, #13235, #25794, #25422, #48332, #58663, #31333, #8428, #47231, #59759, #70857, #42783, #20231, #65304, #14694, #19870, #7704, #69764, #14336, #31701, #69413, #58296, #41686, #47965, #18768, #36506, #30964, #8071, #53499, #70493, #42423, #25050, #36870, #8798, #1818, #30603, #24325, #46874, #30239, #53131, #52772, #64209, #13598, #36144, #2530, #16071, #72963, #34149, #72599, #17517, #27903, #43156, #20597, #67433, #22345, #50438, #39719, #5003, #66699, #6085, #5727, #28617, #38988, #11633, #39352, #27537, #40078, #51154, #23065, #56686, #555, #45620, #196, #61145, #50069, #45253, #68154, #48696, #38621, #21982, #28262, #71219, #44897, #11273, #61503, #33794, #56337, #22701, #5365, #17160, #16795, #62593, #10900, #67786, #61866, #62237, #33428, #11989, #50793, #54236, #3633, #10540, #26157, #33068, #44541, #55607, #67072, #16430, #55971, #52958, #47419, #40800, #63313, #30060, #30430, #12341, #2355, #64402, #52598, #12704, #6810, #34876, #68508, #18955, #51876, #68870, #1275, #17871, #23784, #13413, #35241, #46336, #24872, #69949, #19319, #24147, #34512, #58483, #58119, #28982, #45974, #18226, #57041, #41873, #6447, #41515, #18598, #51520, #919, #52236, #29344, #46700, #57762, #23428, #1641, #69236, #2004, #7171, #40430, #41162, #64034, #29699, #35600, #24515, #7893, #62947, #57405, #47059, #7527, #63671, #13061, #69593, #35962, #49255, #15252, #60309, #42606, #3461, #48886, #54426, #13795, #59951, #4192, #20792, #31525, #14522, #9358, #20422, #3826, #26721, #37789, #54065, #71789, #8621, #36335, #8259, #58849, #20051, #43349, #26347, #71416, #65871, #25981, #9720, #42243, #8993, #30789, #42970, #64767, #31891, #21158, #32253, #54786, #43711, #31150, #53320, #14157, #25614, #48520, #2719, #25235, #36691, #47781, #71047, #70315, #48150, #19690, #59213 ) ),
 .UNSPECIFIED., .F., .F., .F. ) 
 B_SPLINE_SURFACE_WITH_KNOTS ( ( 2, 2 ),
 ( 3, 2, 2, 2, 2, 2, 2, 2, 2, 2, 2, 2, 2, 2, 2, 2, 2, 2, 2, 2, 2, 2, 2, 2, 2, 2, 2, 2, 2, 2, 2, 2, 2, 2, 2, 2, 2, 2, 2, 2, 2, 2, 2, 2, 2, 2, 2, 2, 2, 2, 2, 2, 2, 2, 2, 2, 2, 2, 2, 2, 2, 2, 2, 2, 2, 2, 2, 2, 2, 2, 2, 2, 2, 2, 2, 2, 2, 2, 2, 2, 2, 2, 2, 2, 2, 2, 2, 2, 2, 2, 2, 2, 2, 2, 2, 2, 2, 2, 2, 2, 2, 2, 2, 2, 2, 2, 2, 2, 2, 2, 2, 2, 2, 2, 2, 2, 2, 2, 2, 2, 2, 2, 2, 2, 2, 2, 2, 2, 2, 2, 2, 2, 2, 2, 2, 2, 2, 2, 2, 2, 2, 2, 2, 2, 2, 2, 2, 2, 2, 2, 2, 2, 2, 2, 2, 2, 2, 2, 2, 2, 2, 2, 2, 2, 2, 2, 2, 2, 2, 2, 2, 2, 2, 2, 2, 2, 2, 2, 2, 2, 2, 2, 2, 2, 2, 2, 2, 2, 2, 2, 2, 2, 2, 2, 2, 2, 2, 2, 2, 2, 2, 2, 2, 2, 2, 2, 2, 2, 2, 2, 2, 2, 2, 2, 2, 2, 2, 2, 2, 2, 2, 2, 2, 2, 2, 2, 2, 2, 2, 2, 2, 2, 2, 2, 2, 2, 2, 2, 2, 2, 2, 2, 2, 2, 2, 2, 2, 2, 2, 2, 2, 2, 2, 2, 2, 2, 2, 2, 2, 2, 2, 2, 2, 2, 2, 2, 2, 2, 2, 2, 2, 2, 2, 2, 2, 2, 2, 2, 2, 2, 2, 2, 2, 2, 2, 2, 2, 2, 2, 2, 2, 2, 2, 2, 2, 2, 2, 2, 2, 2, 3 ),
 ( 0.000000000000000000, 1.000000000000000000 ),
 ( 0.000000000000000000, 0.003333333333333333547, 0.006666666666666667095, 0.01000000000000000021, 0.01333333333333333419, 0.01666666666666666644, 0.02000000000000000042, 0.02333333333333333440, 0.02666666666666666838, 0.02999999999999999889, 0.03333333333333333287, 0.03666666666666666685, 0.04000000000000000083, 0.04333333333333333481, 0.04666666666666666879, 0.05000000000000000278, 0.05333333333333333676, 0.05666666666666666380, 0.05999999999999999778, 0.06333333333333333870, 0.06666666666666666574, 0.07000000000000000666, 0.07333333333333333370, 0.07666666666666666075, 0.08000000000000000167, 0.08333333333333332871, 0.08666666666666666963, 0.08999999999999999667, 0.09333333333333333759, 0.09666666666666666463, 0.1000000000000000056, 0.1033333333333333326, 0.1066666666666666735, 0.1100000000000000006, 0.1133333333333333276, 0.1166666666666666685, 0.1199999999999999956, 0.1233333333333333365, 0.1266666666666666774, 0.1300000000000000044, 0.1333333333333333315, 0.1366666666666666585, 0.1400000000000000133, 0.1433333333333333404, 0.1466666666666666674, 0.1499999999999999944, 0.1533333333333333215, 0.1566666666666666763, 0.1600000000000000033, 0.1633333333333333304, 0.1666666666666666574, 0.1700000000000000122, 0.1733333333333333393, 0.1766666666666666663, 0.1799999999999999933, 0.1833333333333333204, 0.1866666666666666752, 0.1900000000000000022, 0.1933333333333333293, 0.1966666666666666563, 0.2000000000000000111, 0.2033333333333333381, 0.2066666666666666652, 0.2099999999999999922, 0.2133333333333333470, 0.2166666666666666741, 0.2200000000000000011, 0.2233333333333333282, 0.2266666666666666552, 0.2300000000000000100, 0.2333333333333333370, 0.2366666666666666641, 0.2399999999999999911, 0.2433333333333333459, 0.2466666666666666730, 0.2500000000000000000, 0.2533333333333333548, 0.2566666666666666541, 0.2600000000000000089, 0.2633333333333333082, 0.2666666666666666630, 0.2700000000000000178, 0.2733333333333333171, 0.2766666666666666718, 0.2800000000000000266, 0.2833333333333333259, 0.2866666666666666807, 0.2899999999999999800, 0.2933333333333333348, 0.2966666666666666896, 0.2999999999999999889, 0.3033333333333333437, 0.3066666666666666430, 0.3099999999999999978, 0.3133333333333333526, 0.3166666666666666519, 0.3200000000000000067, 0.3233333333333333059, 0.3266666666666666607, 0.3300000000000000155, 0.3333333333333333148, 0.3366666666666666696, 0.3400000000000000244, 0.3433333333333333237, 0.3466666666666666785, 0.3499999999999999778, 0.3533333333333333326, 0.3566666666666666874, 0.3599999999999999867, 0.3633333333333333415, 0.3666666666666666408, 0.3699999999999999956, 0.3733333333333333504, 0.3766666666666666496, 0.3800000000000000044, 0.3833333333333333592, 0.3866666666666666585, 0.3900000000000000133, 0.3933333333333333126, 0.3966666666666666674, 0.4000000000000000222, 0.4033333333333333215, 0.4066666666666666763, 0.4099999999999999756, 0.4133333333333333304, 0.4166666666666666852, 0.4199999999999999845, 0.4233333333333333393, 0.4266666666666666941, 0.4299999999999999933, 0.4333333333333333481, 0.4366666666666666474, 0.4400000000000000022, 0.4433333333333333570, 0.4466666666666666563, 0.4500000000000000111, 0.4533333333333333104, 0.4566666666666666652, 0.4600000000000000200, 0.4633333333333333193, 0.4666666666666666741, 0.4699999999999999734, 0.4733333333333333282, 0.4766666666666666829, 0.4799999999999999822, 0.4833333333333333370, 0.4866666666666666918, 0.4899999999999999911, 0.4933333333333333459, 0.4966666666666666452, 0.5000000000000000000, 0.5033333333333332993, 0.5066666666666667096, 0.5100000000000000089, 0.5133333333333333082, 0.5166666666666667185, 0.5200000000000000178, 0.5233333333333333171, 0.5266666666666666163, 0.5300000000000000266, 0.5333333333333333259, 0.5366666666666666252, 0.5400000000000000355, 0.5433333333333333348, 0.5466666666666666341, 0.5500000000000000444, 0.5533333333333333437, 0.5566666666666666430, 0.5600000000000000533, 0.5633333333333333526, 0.5666666666666666519, 0.5699999999999999512, 0.5733333333333333615, 0.5766666666666666607, 0.5799999999999999600, 0.5833333333333333703, 0.5866666666666666696, 0.5899999999999999689, 0.5933333333333333792, 0.5966666666666666785, 0.5999999999999999778, 0.6033333333333333881, 0.6066666666666666874, 0.6099999999999999867, 0.6133333333333332860, 0.6166666666666666963, 0.6199999999999999956, 0.6233333333333332948, 0.6266666666666667052, 0.6300000000000000044, 0.6333333333333333037, 0.6366666666666667140, 0.6400000000000000133, 0.6433333333333333126, 0.6466666666666666119, 0.6500000000000000222, 0.6533333333333333215, 0.6566666666666666208, 0.6600000000000000311, 0.6633333333333333304, 0.6666666666666666297, 0.6700000000000000400, 0.6733333333333333393, 0.6766666666666666385, 0.6800000000000000488, 0.6833333333333333481, 0.6866666666666666474, 0.6899999999999999467, 0.6933333333333333570, 0.6966666666666666563, 0.6999999999999999556, 0.7033333333333333659, 0.7066666666666666652, 0.7099999999999999645, 0.7133333333333333748, 0.7166666666666666741, 0.7199999999999999734, 0.7233333333333333837, 0.7266666666666666829, 0.7299999999999999822, 0.7333333333333332815, 0.7366666666666666918, 0.7399999999999999911, 0.7433333333333332904, 0.7466666666666667007, 0.7500000000000000000, 0.7533333333333332993, 0.7566666666666667096, 0.7600000000000000089, 0.7633333333333333082, 0.7666666666666667185, 0.7700000000000000178, 0.7733333333333333171, 0.7766666666666666163, 0.7800000000000000266, 0.7833333333333333259, 0.7866666666666666252, 0.7900000000000000355, 0.7933333333333333348, 0.7966666666666666341, 0.8000000000000000444, 0.8033333333333333437, 0.8066666666666666430, 0.8100000000000000533, 0.8133333333333333526, 0.8166666666666666519, 0.8199999999999999512, 0.8233333333333333615, 0.8266666666666666607, 0.8299999999999999600, 0.8333333333333333703, 0.8366666666666666696, 0.8399999999999999689, 0.8433333333333333792, 0.8466666666666666785, 0.8499999999999999778, 0.8533333333333333881, 0.8566666666666666874, 0.8599999999999999867, 0.8633333333333332860, 0.8666666666666666963, 0.8699999999999999956, 0.8733333333333332948, 0.8766666666666667052, 0.8800000000000000044, 0.8833333333333333037, 0.8866666666666667140, 0.8900000000000000133, 0.8933333333333333126, 0.8966666666666666119, 0.9000000000000000222, 0.9033333333333333215, 0.9066666666666666208, 0.9100000000000000311, 0.9133333333333333304, 0.9166666666666666297, 0.9200000000000000400, 0.9233333333333333393, 0.9266666666666666385, 0.9300000000000000488, 0.9333333333333333481, 0.9366666666666666474, 0.9399999999999999467, 0.9433333333333333570, 0.9466666666666666563, 0.9499999999999999556, 0.9533333333333333659, 0.9566666666666666652, 0.9599999999999999645, 0.9633333333333333748, 0.9666666666666666741, 0.9699999999999999734, 0.9733333333333333837, 0.9766666666666666829, 0.9799999999999999822, 0.9833333333333332815, 0.9866666666666666918, 0.9899999999999999911, 0.9933333333333332904, 0.9966666666666667007, 1.000000000000000000 ),
 .UNSPECIFIED. ) 
 GEOMETRIC_REPRESENTATION_ITEM ( )  RATIONAL_B_SPLINE_SURFACE ( (
 ( 1.000000000000000000, 0.8660254037844387076, 1.000000000000000000, 0.8660254037844387076, 1.000000000000000000, 0.8660254037844387076, 1.000000000000000000, 0.8660254037844387076, 1.000000000000000000, 0.8660254037844387076, 1.000000000000000000, 0.8660254037844387076, 1.000000000000000000, 0.8660254037844387076, 1.000000000000000000, 0.8660254037844387076, 1.000000000000000000, 0.8660254037844387076, 1.000000000000000000, 0.8660254037844387076, 1.000000000000000000, 0.8660254037844387076, 1.000000000000000000, 0.8660254037844387076, 1.000000000000000000, 0.8660254037844387076, 1.000000000000000000, 0.8660254037844387076, 1.000000000000000000, 0.8660254037844387076, 1.000000000000000000, 0.8660254037844387076, 1.000000000000000000, 0.8660254037844387076, 1.000000000000000000, 0.8660254037844387076, 1.000000000000000000, 0.8660254037844387076, 1.000000000000000000, 0.8660254037844387076, 1.000000000000000000, 0.8660254037844387076, 1.000000000000000000, 0.8660254037844387076, 1.000000000000000000, 0.8660254037844387076, 1.000000000000000000, 0.8660254037844387076, 1.000000000000000000, 0.8660254037844387076, 1.000000000000000000, 0.8660254037844387076, 1.000000000000000000, 0.8660254037844387076, 1.000000000000000000, 0.8660254037844387076, 1.000000000000000000, 0.8660254037844387076, 1.000000000000000000, 0.8660254037844387076, 1.000000000000000000, 0.8660254037844387076, 1.000000000000000000, 0.8660254037844387076, 1.000000000000000000, 0.8660254037844387076, 1.000000000000000000, 0.8660254037844387076, 1.000000000000000000, 0.8660254037844387076, 1.000000000000000000, 0.8660254037844387076, 1.000000000000000000, 0.8660254037844387076, 1.000000000000000000, 0.8660254037844387076, 1.000000000000000000, 0.8660254037844387076, 1.000000000000000000, 0.8660254037844387076, 1.000000000000000000, 0.8660254037844387076, 1.000000000000000000, 0.8660254037844387076, 1.000000000000000000, 0.8660254037844387076, 1.000000000000000000, 0.8660254037844387076, 1.000000000000000000, 0.8660254037844387076, 1.000000000000000000, 0.8660254037844387076, 1.000000000000000000, 0.8660254037844387076, 1.000000000000000000, 0.8660254037844387076, 1.000000000000000000, 0.8660254037844387076, 1.000000000000000000, 0.8660254037844387076, 1.000000000000000000, 0.8660254037844387076, 1.000000000000000000, 0.8660254037844387076, 1.000000000000000000, 0.8660254037844387076, 1.000000000000000000, 0.8660254037844387076, 1.000000000000000000, 0.8660254037844387076, 1.000000000000000000, 0.8660254037844387076, 1.000000000000000000, 0.8660254037844387076, 1.000000000000000000, 0.8660254037844387076, 1.000000000000000000, 0.8660254037844387076, 1.000000000000000000, 0.8660254037844387076, 1.000000000000000000, 0.8660254037844387076, 1.000000000000000000, 0.8660254037844387076, 1.000000000000000000, 0.8660254037844387076, 1.000000000000000000, 0.8660254037844387076, 1.000000000000000000, 0.8660254037844387076, 1.000000000000000000, 0.8660254037844387076, 1.000000000000000000, 0.8660254037844387076, 1.000000000000000000, 0.8660254037844387076, 1.000000000000000000, 0.8660254037844387076, 1.000000000000000000, 0.8660254037844387076, 1.000000000000000000, 0.8660254037844387076, 1.000000000000000000, 0.8660254037844387076, 1.000000000000000000, 0.8660254037844387076, 1.000000000000000000, 0.8660254037844387076, 1.000000000000000000, 0.8660254037844387076, 1.000000000000000000, 0.8660254037844387076, 1.000000000000000000, 0.8660254037844387076, 1.000000000000000000, 0.8660254037844387076, 1.000000000000000000, 0.8660254037844387076, 1.000000000000000000, 0.8660254037844387076, 1.000000000000000000, 0.8660254037844387076, 1.000000000000000000, 0.8660254037844387076, 1.000000000000000000, 0.8660254037844387076, 1.000000000000000000, 0.8660254037844387076, 1.000000000000000000, 0.8660254037844387076, 1.000000000000000000, 0.8660254037844387076, 1.000000000000000000, 0.8660254037844387076, 1.000000000000000000, 0.8660254037844387076, 1.000000000000000000, 0.8660254037844387076, 1.000000000000000000, 0.8660254037844387076, 1.000000000000000000, 0.8660254037844387076, 1.000000000000000000, 0.8660254037844387076, 1.000000000000000000, 0.8660254037844387076, 1.000000000000000000, 0.8660254037844387076, 1.000000000000000000, 0.8660254037844387076, 1.000000000000000000, 0.8660254037844387076, 1.000000000000000000, 0.8660254037844387076, 1.000000000000000000, 0.8660254037844387076, 1.000000000000000000, 0.8660254037844387076, 1.000000000000000000, 0.8660254037844387076, 1.000000000000000000, 0.8660254037844387076, 1.000000000000000000, 0.8660254037844387076, 1.000000000000000000, 0.8660254037844387076, 1.000000000000000000, 0.8660254037844387076, 1.000000000000000000, 0.8660254037844387076, 1.000000000000000000, 0.8660254037844387076, 1.000000000000000000, 0.8660254037844387076, 1.000000000000000000, 0.8660254037844387076, 1.000000000000000000, 0.8660254037844387076, 1.000000000000000000, 0.8660254037844387076, 1.000000000000000000, 0.8660254037844387076, 1.000000000000000000, 0.8660254037844387076, 1.000000000000000000, 0.8660254037844387076, 1.000000000000000000, 0.8660254037844387076, 1.000000000000000000, 0.8660254037844387076, 1.000000000000000000, 0.8660254037844387076, 1.000000000000000000, 0.8660254037844387076, 1.000000000000000000, 0.8660254037844387076, 1.000000000000000000, 0.8660254037844387076, 1.000000000000000000, 0.8660254037844387076, 1.000000000000000000, 0.8660254037844387076, 1.000000000000000000, 0.8660254037844387076, 1.000000000000000000, 0.8660254037844387076, 1.000000000000000000, 0.8660254037844387076, 1.000000000000000000, 0.8660254037844387076, 1.000000000000000000, 0.8660254037844387076, 1.000000000000000000, 0.8660254037844387076, 1.000000000000000000, 0.8660254037844387076, 1.000000000000000000, 0.8660254037844387076, 1.000000000000000000, 0.8660254037844387076, 1.000000000000000000, 0.8660254037844387076, 1.000000000000000000, 0.8660254037844387076, 1.000000000000000000, 0.8660254037844387076, 1.000000000000000000, 0.8660254037844387076, 1.000000000000000000, 0.8660254037844387076, 1.000000000000000000, 0.8660254037844387076, 1.000000000000000000, 0.8660254037844387076, 1.000000000000000000, 0.8660254037844387076, 1.000000000000000000, 0.8660254037844387076, 1.000000000000000000, 0.8660254037844387076, 1.000000000000000000, 0.8660254037844387076, 1.000000000000000000, 0.8660254037844387076, 1.000000000000000000, 0.8660254037844387076, 1.000000000000000000, 0.8660254037844387076, 1.000000000000000000, 0.8660254037844387076, 1.000000000000000000, 0.8660254037844387076, 1.000000000000000000, 0.8660254037844387076, 1.000000000000000000, 0.8660254037844387076, 1.000000000000000000, 0.8660254037844387076, 1.000000000000000000, 0.8660254037844387076, 1.000000000000000000, 0.8660254037844387076, 1.000000000000000000, 0.8660254037844387076, 1.000000000000000000, 0.8660254037844387076, 1.000000000000000000, 0.8660254037844387076, 1.000000000000000000, 0.8660254037844387076, 1.000000000000000000, 0.8660254037844387076, 1.000000000000000000, 0.8660254037844387076, 1.000000000000000000, 0.8660254037844387076, 1.000000000000000000, 0.8660254037844387076, 1.000000000000000000, 0.8660254037844387076, 1.000000000000000000, 0.8660254037844387076, 1.000000000000000000, 0.8660254037844387076, 1.000000000000000000, 0.8660254037844387076, 1.000000000000000000, 0.8660254037844387076, 1.000000000000000000, 0.8660254037844387076, 1.000000000000000000, 0.8660254037844387076, 1.000000000000000000, 0.8660254037844387076, 1.000000000000000000, 0.8660254037844387076, 1.000000000000000000, 0.8660254037844387076, 1.000000000000000000, 0.8660254037844387076, 1.000000000000000000, 0.8660254037844387076, 1.000000000000000000, 0.8660254037844387076, 1.000000000000000000, 0.8660254037844387076, 1.000000000000000000, 0.8660254037844387076, 1.000000000000000000, 0.8660254037844387076, 1.000000000000000000, 0.8660254037844387076, 1.000000000000000000, 0.8660254037844387076, 1.000000000000000000, 0.8660254037844387076, 1.000000000000000000, 0.8660254037844387076, 1.000000000000000000, 0.8660254037844387076, 1.000000000000000000, 0.8660254037844387076, 1.000000000000000000, 0.8660254037844387076, 1.000000000000000000, 0.8660254037844387076, 1.000000000000000000, 0.8660254037844387076, 1.000000000000000000, 0.8660254037844387076, 1.000000000000000000, 0.8660254037844387076, 1.000000000000000000, 0.8660254037844387076, 1.000000000000000000, 0.8660254037844387076, 1.000000000000000000, 0.8660254037844387076, 1.000000000000000000, 0.8660254037844387076, 1.000000000000000000, 0.8660254037844387076, 1.000000000000000000, 0.8660254037844387076, 1.000000000000000000, 0.8660254037844387076, 1.000000000000000000, 0.8660254037844387076, 1.000000000000000000, 0.8660254037844387076, 1.000000000000000000, 0.8660254037844387076, 1.000000000000000000, 0.8660254037844387076, 1.000000000000000000, 0.8660254037844387076, 1.000000000000000000, 0.8660254037844387076, 1.000000000000000000, 0.8660254037844387076, 1.000000000000000000, 0.8660254037844387076, 1.000000000000000000, 0.8660254037844387076, 1.000000000000000000, 0.8660254037844387076, 1.000000000000000000, 0.8660254037844387076, 1.000000000000000000, 0.8660254037844387076, 1.000000000000000000, 0.8660254037844387076, 1.000000000000000000, 0.8660254037844387076, 1.000000000000000000, 0.8660254037844387076, 1.000000000000000000, 0.8660254037844387076, 1.000000000000000000, 0.8660254037844387076, 1.000000000000000000, 0.8660254037844387076, 1.000000000000000000, 0.8660254037844387076, 1.000000000000000000, 0.8660254037844387076, 1.000000000000000000, 0.8660254037844387076, 1.000000000000000000, 0.8660254037844387076, 1.000000000000000000, 0.8660254037844387076, 1.000000000000000000, 0.8660254037844387076, 1.000000000000000000, 0.8660254037844387076, 1.000000000000000000, 0.8660254037844387076, 1.000000000000000000, 0.8660254037844387076, 1.000000000000000000, 0.8660254037844387076, 1.000000000000000000, 0.8660254037844387076, 1.000000000000000000, 0.8660254037844387076, 1.000000000000000000, 0.8660254037844387076, 1.000000000000000000, 0.8660254037844387076, 1.000000000000000000, 0.8660254037844387076, 1.000000000000000000, 0.8660254037844387076, 1.000000000000000000, 0.8660254037844387076, 1.000000000000000000, 0.8660254037844387076, 1.000000000000000000, 0.8660254037844387076, 1.000000000000000000, 0.8660254037844387076, 1.000000000000000000, 0.8660254037844387076, 1.000000000000000000, 0.8660254037844387076, 1.000000000000000000, 0.8660254037844387076, 1.000000000000000000, 0.8660254037844387076, 1.000000000000000000, 0.8660254037844387076, 1.000000000000000000, 0.8660254037844387076, 1.000000000000000000, 0.8660254037844387076, 1.000000000000000000, 0.8660254037844387076, 1.000000000000000000, 0.8660254037844387076, 1.000000000000000000, 0.8660254037844387076, 1.000000000000000000, 0.8660254037844387076, 1.000000000000000000, 0.8660254037844387076, 1.000000000000000000, 0.8660254037844387076, 1.000000000000000000, 0.8660254037844387076, 1.000000000000000000, 0.8660254037844387076, 1.000000000000000000, 0.8660254037844387076, 1.000000000000000000, 0.8660254037844387076, 1.000000000000000000, 0.8660254037844387076, 1.000000000000000000, 0.8660254037844387076, 1.000000000000000000, 0.8660254037844387076, 1.000000000000000000, 0.8660254037844387076, 1.000000000000000000, 0.8660254037844387076, 1.000000000000000000, 0.8660254037844387076, 1.000000000000000000, 0.8660254037844387076, 1.000000000000000000, 0.8660254037844387076, 1.000000000000000000, 0.8660254037844387076, 1.000000000000000000, 0.8660254037844387076, 1.000000000000000000, 0.8660254037844387076, 1.000000000000000000, 0.8660254037844387076, 1.000000000000000000, 0.8660254037844387076, 1.000000000000000000, 0.8660254037844387076, 1.000000000000000000, 0.8660254037844387076, 1.000000000000000000, 0.8660254037844387076, 1.000000000000000000, 0.8660254037844387076, 1.000000000000000000, 0.8660254037844387076, 1.000000000000000000, 0.8660254037844387076, 1.000000000000000000, 0.8660254037844387076, 1.000000000000000000, 0.8660254037844387076, 1.000000000000000000, 0.8660254037844387076, 1.000000000000000000, 0.8660254037844387076, 1.000000000000000000, 0.8660254037844387076, 1.000000000000000000, 0.8660254037844387076, 1.000000000000000000, 0.8660254037844387076, 1.000000000000000000, 0.8660254037844387076, 1.000000000000000000, 0.8660254037844387076, 1.000000000000000000, 0.8660254037844387076, 1.000000000000000000, 0.8660254037844387076, 1.000000000000000000, 0.8660254037844387076, 1.000000000000000000, 0.8660254037844387076, 1.000000000000000000, 0.8660254037844387076, 1.000000000000000000, 0.8660254037844387076, 1.000000000000000000, 0.8660254037844387076, 1.000000000000000000, 0.8660254037844387076, 1.000000000000000000, 0.8660254037844387076, 1.000000000000000000, 0.8660254037844387076, 1.000000000000000000, 0.8660254037844387076, 1.000000000000000000, 0.8660254037844387076, 1.000000000000000000, 0.8660254037844387076, 1.000000000000000000, 0.8660254037844387076, 1.000000000000000000, 0.8660254037844387076, 1.000000000000000000, 0.8660254037844387076, 1.000000000000000000, 0.8660254037844387076, 1.000000000000000000, 0.8660254037844387076, 1.000000000000000000, 0.8660254037844387076, 1.000000000000000000, 0.8660254037844387076, 1.000000000000000000, 0.8660254037844387076, 1.000000000000000000, 0.8660254037844387076, 1.000000000000000000, 0.8660254037844387076, 1.000000000000000000, 0.8660254037844387076, 1.000000000000000000),
 ( 1.000000000000000000, 0.8660254037844387076, 1.000000000000000000, 0.8660254037844387076, 1.000000000000000000, 0.8660254037844387076, 1.000000000000000000, 0.8660254037844387076, 1.000000000000000000, 0.8660254037844387076, 1.000000000000000000, 0.8660254037844387076, 1.000000000000000000, 0.8660254037844387076, 1.000000000000000000, 0.8660254037844387076, 1.000000000000000000, 0.8660254037844387076, 1.000000000000000000, 0.8660254037844387076, 1.000000000000000000, 0.8660254037844387076, 1.000000000000000000, 0.8660254037844387076, 1.000000000000000000, 0.8660254037844387076, 1.000000000000000000, 0.8660254037844387076, 1.000000000000000000, 0.8660254037844387076, 1.000000000000000000, 0.8660254037844387076, 1.000000000000000000, 0.8660254037844387076, 1.000000000000000000, 0.8660254037844387076, 1.000000000000000000, 0.8660254037844387076, 1.000000000000000000, 0.8660254037844387076, 1.000000000000000000, 0.8660254037844387076, 1.000000000000000000, 0.8660254037844387076, 1.000000000000000000, 0.8660254037844387076, 1.000000000000000000, 0.8660254037844387076, 1.000000000000000000, 0.8660254037844387076, 1.000000000000000000, 0.8660254037844387076, 1.000000000000000000, 0.8660254037844387076, 1.000000000000000000, 0.8660254037844387076, 1.000000000000000000, 0.8660254037844387076, 1.000000000000000000, 0.8660254037844387076, 1.000000000000000000, 0.8660254037844387076, 1.000000000000000000, 0.8660254037844387076, 1.000000000000000000, 0.8660254037844387076, 1.000000000000000000, 0.8660254037844387076, 1.000000000000000000, 0.8660254037844387076, 1.000000000000000000, 0.8660254037844387076, 1.000000000000000000, 0.8660254037844387076, 1.000000000000000000, 0.8660254037844387076, 1.000000000000000000, 0.8660254037844387076, 1.000000000000000000, 0.8660254037844387076, 1.000000000000000000, 0.8660254037844387076, 1.000000000000000000, 0.8660254037844387076, 1.000000000000000000, 0.8660254037844387076, 1.000000000000000000, 0.8660254037844387076, 1.000000000000000000, 0.8660254037844387076, 1.000000000000000000, 0.8660254037844387076, 1.000000000000000000, 0.8660254037844387076, 1.000000000000000000, 0.8660254037844387076, 1.000000000000000000, 0.8660254037844387076, 1.000000000000000000, 0.8660254037844387076, 1.000000000000000000, 0.8660254037844387076, 1.000000000000000000, 0.8660254037844387076, 1.000000000000000000, 0.8660254037844387076, 1.000000000000000000, 0.8660254037844387076, 1.000000000000000000, 0.8660254037844387076, 1.000000000000000000, 0.8660254037844387076, 1.000000000000000000, 0.8660254037844387076, 1.000000000000000000, 0.8660254037844387076, 1.000000000000000000, 0.8660254037844387076, 1.000000000000000000, 0.8660254037844387076, 1.000000000000000000, 0.8660254037844387076, 1.000000000000000000, 0.8660254037844387076, 1.000000000000000000, 0.8660254037844387076, 1.000000000000000000, 0.8660254037844387076, 1.000000000000000000, 0.8660254037844387076, 1.000000000000000000, 0.8660254037844387076, 1.000000000000000000, 0.8660254037844387076, 1.000000000000000000, 0.8660254037844387076, 1.000000000000000000, 0.8660254037844387076, 1.000000000000000000, 0.8660254037844387076, 1.000000000000000000, 0.8660254037844387076, 1.000000000000000000, 0.8660254037844387076, 1.000000000000000000, 0.8660254037844387076, 1.000000000000000000, 0.8660254037844387076, 1.000000000000000000, 0.8660254037844387076, 1.000000000000000000, 0.8660254037844387076, 1.000000000000000000, 0.8660254037844387076, 1.000000000000000000, 0.8660254037844387076, 1.000000000000000000, 0.8660254037844387076, 1.000000000000000000, 0.8660254037844387076, 1.000000000000000000, 0.8660254037844387076, 1.000000000000000000, 0.8660254037844387076, 1.000000000000000000, 0.8660254037844387076, 1.000000000000000000, 0.8660254037844387076, 1.000000000000000000, 0.8660254037844387076, 1.000000000000000000, 0.8660254037844387076, 1.000000000000000000, 0.8660254037844387076, 1.000000000000000000, 0.8660254037844387076, 1.000000000000000000, 0.8660254037844387076, 1.000000000000000000, 0.8660254037844387076, 1.000000000000000000, 0.8660254037844387076, 1.000000000000000000, 0.8660254037844387076, 1.000000000000000000, 0.8660254037844387076, 1.000000000000000000, 0.8660254037844387076, 1.000000000000000000, 0.8660254037844387076, 1.000000000000000000, 0.8660254037844387076, 1.000000000000000000, 0.8660254037844387076, 1.000000000000000000, 0.8660254037844387076, 1.000000000000000000, 0.8660254037844387076, 1.000000000000000000, 0.8660254037844387076, 1.000000000000000000, 0.8660254037844387076, 1.000000000000000000, 0.8660254037844387076, 1.000000000000000000, 0.8660254037844387076, 1.000000000000000000, 0.8660254037844387076, 1.000000000000000000, 0.8660254037844387076, 1.000000000000000000, 0.8660254037844387076, 1.000000000000000000, 0.8660254037844387076, 1.000000000000000000, 0.8660254037844387076, 1.000000000000000000, 0.8660254037844387076, 1.000000000000000000, 0.8660254037844387076, 1.000000000000000000, 0.8660254037844387076, 1.000000000000000000, 0.8660254037844387076, 1.000000000000000000, 0.8660254037844387076, 1.000000000000000000, 0.8660254037844387076, 1.000000000000000000, 0.8660254037844387076, 1.000000000000000000, 0.8660254037844387076, 1.000000000000000000, 0.8660254037844387076, 1.000000000000000000, 0.8660254037844387076, 1.000000000000000000, 0.8660254037844387076, 1.000000000000000000, 0.8660254037844387076, 1.000000000000000000, 0.8660254037844387076, 1.000000000000000000, 0.8660254037844387076, 1.000000000000000000, 0.8660254037844387076, 1.000000000000000000, 0.8660254037844387076, 1.000000000000000000, 0.8660254037844387076, 1.000000000000000000, 0.8660254037844387076, 1.000000000000000000, 0.8660254037844387076, 1.000000000000000000, 0.8660254037844387076, 1.000000000000000000, 0.8660254037844387076, 1.000000000000000000, 0.8660254037844387076, 1.000000000000000000, 0.8660254037844387076, 1.000000000000000000, 0.8660254037844387076, 1.000000000000000000, 0.8660254037844387076, 1.000000000000000000, 0.8660254037844387076, 1.000000000000000000, 0.8660254037844387076, 1.000000000000000000, 0.8660254037844387076, 1.000000000000000000, 0.8660254037844387076, 1.000000000000000000, 0.8660254037844387076, 1.000000000000000000, 0.8660254037844387076, 1.000000000000000000, 0.8660254037844387076, 1.000000000000000000, 0.8660254037844387076, 1.000000000000000000, 0.8660254037844387076, 1.000000000000000000, 0.8660254037844387076, 1.000000000000000000, 0.8660254037844387076, 1.000000000000000000, 0.8660254037844387076, 1.000000000000000000, 0.8660254037844387076, 1.000000000000000000, 0.8660254037844387076, 1.000000000000000000, 0.8660254037844387076, 1.000000000000000000, 0.8660254037844387076, 1.000000000000000000, 0.8660254037844387076, 1.000000000000000000, 0.8660254037844387076, 1.000000000000000000, 0.8660254037844387076, 1.000000000000000000, 0.8660254037844387076, 1.000000000000000000, 0.8660254037844387076, 1.000000000000000000, 0.8660254037844387076, 1.000000000000000000, 0.8660254037844387076, 1.000000000000000000, 0.8660254037844387076, 1.000000000000000000, 0.8660254037844387076, 1.000000000000000000, 0.8660254037844387076, 1.000000000000000000, 0.8660254037844387076, 1.000000000000000000, 0.8660254037844387076, 1.000000000000000000, 0.8660254037844387076, 1.000000000000000000, 0.8660254037844387076, 1.000000000000000000, 0.8660254037844387076, 1.000000000000000000, 0.8660254037844387076, 1.000000000000000000, 0.8660254037844387076, 1.000000000000000000, 0.8660254037844387076, 1.000000000000000000, 0.8660254037844387076, 1.000000000000000000, 0.8660254037844387076, 1.000000000000000000, 0.8660254037844387076, 1.000000000000000000, 0.8660254037844387076, 1.000000000000000000, 0.8660254037844387076, 1.000000000000000000, 0.8660254037844387076, 1.000000000000000000, 0.8660254037844387076, 1.000000000000000000, 0.8660254037844387076, 1.000000000000000000, 0.8660254037844387076, 1.000000000000000000, 0.8660254037844387076, 1.000000000000000000, 0.8660254037844387076, 1.000000000000000000, 0.8660254037844387076, 1.000000000000000000, 0.8660254037844387076, 1.000000000000000000, 0.8660254037844387076, 1.000000000000000000, 0.8660254037844387076, 1.000000000000000000, 0.8660254037844387076, 1.000000000000000000, 0.8660254037844387076, 1.000000000000000000, 0.8660254037844387076, 1.000000000000000000, 0.8660254037844387076, 1.000000000000000000, 0.8660254037844387076, 1.000000000000000000, 0.8660254037844387076, 1.000000000000000000, 0.8660254037844387076, 1.000000000000000000, 0.8660254037844387076, 1.000000000000000000, 0.8660254037844387076, 1.000000000000000000, 0.8660254037844387076, 1.000000000000000000, 0.8660254037844387076, 1.000000000000000000, 0.8660254037844387076, 1.000000000000000000, 0.8660254037844387076, 1.000000000000000000, 0.8660254037844387076, 1.000000000000000000, 0.8660254037844387076, 1.000000000000000000, 0.8660254037844387076, 1.000000000000000000, 0.8660254037844387076, 1.000000000000000000, 0.8660254037844387076, 1.000000000000000000, 0.8660254037844387076, 1.000000000000000000, 0.8660254037844387076, 1.000000000000000000, 0.8660254037844387076, 1.000000000000000000, 0.8660254037844387076, 1.000000000000000000, 0.8660254037844387076, 1.000000000000000000, 0.8660254037844387076, 1.000000000000000000, 0.8660254037844387076, 1.000000000000000000, 0.8660254037844387076, 1.000000000000000000, 0.8660254037844387076, 1.000000000000000000, 0.8660254037844387076, 1.000000000000000000, 0.8660254037844387076, 1.000000000000000000, 0.8660254037844387076, 1.000000000000000000, 0.8660254037844387076, 1.000000000000000000, 0.8660254037844387076, 1.000000000000000000, 0.8660254037844387076, 1.000000000000000000, 0.8660254037844387076, 1.000000000000000000, 0.8660254037844387076, 1.000000000000000000, 0.8660254037844387076, 1.000000000000000000, 0.8660254037844387076, 1.000000000000000000, 0.8660254037844387076, 1.000000000000000000, 0.8660254037844387076, 1.000000000000000000, 0.8660254037844387076, 1.000000000000000000, 0.8660254037844387076, 1.000000000000000000, 0.8660254037844387076, 1.000000000000000000, 0.8660254037844387076, 1.000000000000000000, 0.8660254037844387076, 1.000000000000000000, 0.8660254037844387076, 1.000000000000000000, 0.8660254037844387076, 1.000000000000000000, 0.8660254037844387076, 1.000000000000000000, 0.8660254037844387076, 1.000000000000000000, 0.8660254037844387076, 1.000000000000000000, 0.8660254037844387076, 1.000000000000000000, 0.8660254037844387076, 1.000000000000000000, 0.8660254037844387076, 1.000000000000000000, 0.8660254037844387076, 1.000000000000000000, 0.8660254037844387076, 1.000000000000000000, 0.8660254037844387076, 1.000000000000000000, 0.8660254037844387076, 1.000000000000000000, 0.8660254037844387076, 1.000000000000000000, 0.8660254037844387076, 1.000000000000000000, 0.8660254037844387076, 1.000000000000000000, 0.8660254037844387076, 1.000000000000000000, 0.8660254037844387076, 1.000000000000000000, 0.8660254037844387076, 1.000000000000000000, 0.8660254037844387076, 1.000000000000000000, 0.8660254037844387076, 1.000000000000000000, 0.8660254037844387076, 1.000000000000000000, 0.8660254037844387076, 1.000000000000000000, 0.8660254037844387076, 1.000000000000000000, 0.8660254037844387076, 1.000000000000000000, 0.8660254037844387076, 1.000000000000000000, 0.8660254037844387076, 1.000000000000000000, 0.8660254037844387076, 1.000000000000000000, 0.8660254037844387076, 1.000000000000000000, 0.8660254037844387076, 1.000000000000000000, 0.8660254037844387076, 1.000000000000000000, 0.8660254037844387076, 1.000000000000000000, 0.8660254037844387076, 1.000000000000000000, 0.8660254037844387076, 1.000000000000000000, 0.8660254037844387076, 1.000000000000000000, 0.8660254037844387076, 1.000000000000000000, 0.8660254037844387076, 1.000000000000000000, 0.8660254037844387076, 1.000000000000000000, 0.8660254037844387076, 1.000000000000000000, 0.8660254037844387076, 1.000000000000000000, 0.8660254037844387076, 1.000000000000000000, 0.8660254037844387076, 1.000000000000000000, 0.8660254037844387076, 1.000000000000000000, 0.8660254037844387076, 1.000000000000000000, 0.8660254037844387076, 1.000000000000000000, 0.8660254037844387076, 1.000000000000000000, 0.8660254037844387076, 1.000000000000000000, 0.8660254037844387076, 1.000000000000000000, 0.8660254037844387076, 1.000000000000000000, 0.8660254037844387076, 1.000000000000000000, 0.8660254037844387076, 1.000000000000000000, 0.8660254037844387076, 1.000000000000000000, 0.8660254037844387076, 1.000000000000000000, 0.8660254037844387076, 1.000000000000000000, 0.8660254037844387076, 1.000000000000000000, 0.8660254037844387076, 1.000000000000000000, 0.8660254037844387076, 1.000000000000000000, 0.8660254037844387076, 1.000000000000000000, 0.8660254037844387076, 1.000000000000000000, 0.8660254037844387076, 1.000000000000000000, 0.8660254037844387076, 1.000000000000000000, 0.8660254037844387076, 1.000000000000000000, 0.8660254037844387076, 1.000000000000000000, 0.8660254037844387076, 1.000000000000000000, 0.8660254037844387076, 1.000000000000000000, 0.8660254037844387076, 1.000000000000000000, 0.8660254037844387076, 1.000000000000000000, 0.8660254037844387076, 1.000000000000000000, 0.8660254037844387076, 1.000000000000000000, 0.8660254037844387076, 1.000000000000000000, 0.8660254037844387076, 1.000000000000000000, 0.8660254037844387076, 1.000000000000000000, 0.8660254037844387076, 1.000000000000000000, 0.8660254037844387076, 1.000000000000000000, 0.8660254037844387076, 1.000000000000000000) ) ) 
 REPRESENTATION_ITEM ( '' )  SURFACE ( )  );
#12411 = CARTESIAN_POINT ( 'NONE',  ( 25.76250000122903216, -4.330127018922190985, -2.500000000000001332 ) ) ;
#12412 = CARTESIAN_POINT ( 'NONE',  ( 20.99999999999999645, 0.000000000000000000, 4.999999999999998224 ) ) ;
#12413 = VECTOR ( 'NONE', #53805, 1000.000000000000000 ) ;
#12414 = CARTESIAN_POINT ( 'NONE',  ( 23.22187500061451715, -6.054752690667223547, -1.112240025338166033E-15 ) ) ;
#12415 = CARTESIAN_POINT ( 'NONE',  ( 30.00000000000000000, 0.000000000000000000, 0.000000000000000000 ) ) ;
#12416 = CARTESIAN_POINT ( 'NONE',  ( 11.25000000122903288, -2.886751345948129988, 4.999999999999997335 ) ) ;
#12417 = CARTESIAN_POINT ( 'NONE',  ( 7.884375000614517681, -4.541064518000419881, 2.621784821874995952 ) ) ;
#12418 = CARTESIAN_POINT ( 'NONE',  ( 25.20937500061451431, 4.541064518000418104, -2.621784821874998173 ) ) ;
#12419 = CARTESIAN_POINT ( 'NONE',  ( 3.609375000614516882, 4.541064518000418104, -2.621784821874998173 ) ) ;
#12420 = CARTESIAN_POINT ( 'NONE',  ( 20.61562500061451431, 3.027376345333613106, -5.243569643749998122 ) ) ;
#12421 = CARTESIAN_POINT ( 'NONE',  ( 26.63437500061451857, 4.541064518000418104, 2.621784821874999949 ) ) ;
#12422 = CARTESIAN_POINT ( 'NONE',  ( -3.756430356250000990, 17.51562499938548356, 32.16877607737301048 ) ) ;
#12423 = CARTESIAN_POINT ( 'NONE',  ( 18.52499999999999858, 6.123233995736764310E-16, -4.999999999999998224 ) ) ;
#12424 = CARTESIAN_POINT ( 'NONE',  ( 7.284375000614518036, 4.541064518000418104, 2.621784821874999949 ) ) ;
#12425 = CARTESIAN_POINT ( 'NONE',  ( 18.96562500061451573, 3.027376345333611329, 5.243569643749999010 ) ) ;
#12426 = CARTESIAN_POINT ( 'NONE',  ( 15.97499999999999964, 4.330127018922191873, 2.499999999999999556 ) ) ;
#12427 = CARTESIAN_POINT ( 'NONE',  ( 28.26562500061451289, 3.027376345333613106, -5.243569643749998122 ) ) ;
#12428 = CARTESIAN_POINT ( 'NONE',  ( 4.584375000614516971, 4.541064518000418104, 2.621784821874999949 ) ) ;
#12429 = CARTESIAN_POINT ( 'NONE',  ( 22.83750000122903501, 4.330127018922191873, 2.499999999999999556 ) ) ;
#12430 = DIRECTION ( 'NONE',  ( -0.000000000000000000, -1.000000000000000000, -0.000000000000000000 ) ) ;
#12431 = CARTESIAN_POINT ( 'NONE',  ( 17.51249999999999929, -5.773502691896255534, -1.060575238724906372E-15 ) ) ;
#12432 = ORIENTED_EDGE ( 'NONE', *, *, #5228, .F. ) ;
#12433 = CARTESIAN_POINT ( 'NONE',  ( 24.78750000000000497, -2.886751345948125991, -5.000000000000000000 ) ) ;
#12434 = CARTESIAN_POINT ( 'NONE',  ( 27.19687500061451857, -3.027376345333614438, 5.243569643749998122 ) ) ;
#12435 = ADVANCED_FACE ( 'NONE', ( #59414 ), #31835, .T. ) ;
#12436 = ORIENTED_EDGE ( 'NONE', *, *, #45135, .T. ) ;
#12437 = CARTESIAN_POINT ( 'NONE',  ( 14.65312500061451573, -4.541064518000417216, -2.621784821875001281 ) ) ;
#12438 = CARTESIAN_POINT ( 'NONE',  ( 7.115625000614516082, 3.027376345333613106, -5.243569643749998122 ) ) ;
#12439 = CARTESIAN_POINT ( 'NONE',  ( 18.75937500061451857, 2.746126346562645981, -4.756430356249997438 ) ) ;
#12440 = CARTESIAN_POINT ( 'NONE',  ( 29.20312500061451644, 4.541064518000418104, -2.621784821874998173 ) ) ;
#12441 = EDGE_CURVE ( 'NONE', #39861, #20263, #50628, .T. ) ;
#12442 = CARTESIAN_POINT ( 'NONE',  ( 15.37500000122903465, -5.773502691896255534, -1.060575238724906372E-15 ) ) ;
#12443 = AXIS2_PLACEMENT_3D ( 'NONE', #40121, #34556, #57084 ) ;
#12444 = CARTESIAN_POINT ( 'NONE',  ( 22.31250000000000000, 2.886751345948126879, 4.999999999999999112 ) ) ;
#12445 = CARTESIAN_POINT ( 'NONE',  ( 28.64999999999999858, 0.000000000000000000, 4.999999999999998224 ) ) ;
#12446 = CARTESIAN_POINT ( 'NONE',  ( 3.609375000614516882, 4.541064518000418104, -2.621784821874998173 ) ) ;
#12447 = CARTESIAN_POINT ( 'NONE',  ( 9.421875000614519990, 3.027376345333613106, -5.243569643749998122 ) ) ;
#12448 = CARTESIAN_POINT ( 'NONE',  ( 20.74687500061451573, 6.054752690667223547, 3.707466751127219781E-16 ) ) ;
#12449 = DIRECTION ( 'NONE',  ( -1.000000000000000000, -0.000000000000000000, -0.000000000000000000 ) ) ;
#12450 = ORIENTED_EDGE ( 'NONE', *, *, #45017, .F. ) ;
#12451 = CARTESIAN_POINT ( 'NONE',  ( 3.271875000614519635, 3.027376345333611329, 5.243569643749999010 ) ) ;
#12452 = CARTESIAN_POINT ( 'NONE',  ( 6.000000000000001776, 4.330127018922192761, -2.499999999999997780 ) ) ;
#12453 = VECTOR ( 'NONE', #33625, 1000.000000000000000 ) ;
#12454 = CARTESIAN_POINT ( 'NONE',  ( 7.171875000614517326, 3.027376345333613106, -5.243569643749998122 ) ) ;
#12455 = CARTESIAN_POINT ( 'NONE',  ( 19.38749999999999929, -2.886751345948125991, -5.000000000000000000 ) ) ;
#12456 = CARTESIAN_POINT ( 'NONE',  ( 15.17812500061451608, 6.421520780324663323E-16, -5.243569643749999010 ) ) ;
#12457 = CARTESIAN_POINT ( 'NONE',  ( 2.000000000000000444, 18.87500000000000000, 26.53589838486224650 ) ) ;
#12458 = DIRECTION ( 'NONE',  ( -1.000000000000000000, -0.000000000000000000, -0.000000000000000000 ) ) ;
#12459 = CARTESIAN_POINT ( 'NONE',  ( 21.12187500061451573, 2.746126346562645981, -4.756430356249997438 ) ) ;
#12460 = CARTESIAN_POINT ( 'NONE',  ( 9.178125000614517859, -4.541064518000419881, 2.621784821874995952 ) ) ;
#12461 = CARTESIAN_POINT ( 'NONE',  ( 27.64687500061452141, -3.027376345333614438, 5.243569643749998122 ) ) ;
#12462 = ADVANCED_FACE ( 'NONE', ( #3238 ), #25395, .F. ) ;
#12463 = CARTESIAN_POINT ( 'NONE',  ( -2.121784821874996840, 19.48437500061451644, 33.67503911421598417 ) ) ;
#12464 = CARTESIAN_POINT ( 'NONE',  ( 27.04687500061451644, 6.054752690667223547, 3.707466751127219781E-16 ) ) ;
#12465 = CARTESIAN_POINT ( 'NONE',  ( 7.087499999999999467, -2.886751345948129988, 4.999999999999997335 ) ) ;
#12466 = CARTESIAN_POINT ( 'NONE',  ( 1.999999999999998668, 12.76250000122903394, 26.53589838486224650 ) ) ;
#12467 = CARTESIAN_POINT ( 'NONE',  ( 13.86562500061451431, 3.027376345333613106, -5.243569643749998122 ) ) ;
#12468 = CARTESIAN_POINT ( 'NONE',  ( 6.375000001229031987, -5.773502691896255534, -1.060575238724906372E-15 ) ) ;
#12469 = AXIS2_PLACEMENT_3D ( 'NONE', #34077, #1205, #40724 ) ;
#12470 = CARTESIAN_POINT ( 'NONE',  ( 17.33437500061451431, -4.541064518000419881, 2.621784821874995952 ) ) ;
#12471 = CARTESIAN_POINT ( 'NONE',  ( 11.59687500061451892, -3.027376345333610441, -5.243569643749999898 ) ) ;
#12472 = LINE ( 'NONE', #39837, #31279 ) ;
#12473 = ORIENTED_EDGE ( 'NONE', *, *, #58187, .T. ) ;
#12474 = CARTESIAN_POINT ( 'NONE',  ( 12.62812500061451537, 4.541064518000418104, 2.621784821874999949 ) ) ;
#12475 = CARTESIAN_POINT ( 'NONE',  ( 26.47500000122903074, 2.886751345948126879, 4.999999999999999112 ) ) ;
#12476 = CARTESIAN_POINT ( 'NONE',  ( 12.34687500061452070, -3.027376345333614438, 5.243569643749998122 ) ) ;
#12477 = CARTESIAN_POINT ( 'NONE',  ( 3.038088735723365019, 9.529008066655462628, -35.17764897947208169 ) ) ;
#12478 = CARTESIAN_POINT ( 'NONE',  ( 15.44062500061451537, -3.027376345333614438, 5.243569643749998122 ) ) ;
#12479 = EDGE_CURVE ( 'NONE', #51420, #32936, #67229, .T. ) ;
#12480 = CARTESIAN_POINT ( 'NONE',  ( 29.49375000122902790, 5.773502691896255534, 3.535250795749688894E-16 ) ) ;
#12481 = CARTESIAN_POINT ( 'NONE',  ( 24.68437500061451573, 6.421520780324663323E-16, -5.243569643749999010 ) ) ;
#12482 = CYLINDRICAL_SURFACE ( 'NONE', #67937, 4.999999999999998224 ) ;
#12483 = CARTESIAN_POINT ( 'NONE',  ( 10.80000000122903536, -2.886751345948129988, 4.999999999999997335 ) ) ;
#12484 = CARTESIAN_POINT ( 'NONE',  ( 4.924325218087134637, -0.8666147624583920850, 4.924325218087160394 ) ) ;
#12485 = CYLINDRICAL_SURFACE ( 'NONE', #44287, 4.000000000000000000 ) ;
#12486 = CARTESIAN_POINT ( 'NONE',  ( -2.121784821874996840, 17.68437500061451928, -26.32496088578401583 ) ) ;
#12487 = CARTESIAN_POINT ( 'NONE',  ( 18.04687500061451999, 6.054752690667223547, 3.707466751127219781E-16 ) ) ;
#12488 = CARTESIAN_POINT ( 'NONE',  ( 19.05000000122903359, -2.886751345948125991, -5.000000000000000000 ) ) ;
#12489 = CARTESIAN_POINT ( 'NONE',  ( 13.77187500061451786, -6.054752690667223547, -1.112240025338166033E-15 ) ) ;
#12490 = CARTESIAN_POINT ( 'NONE',  ( -4.243569643749997233, 19.39062500061451999, -27.54997392385601174 ) ) ;
#12491 = CARTESIAN_POINT ( 'NONE',  ( 18.97500000122903074, -5.773502691896255534, -1.060575238724906372E-15 ) ) ;
#12492 = CARTESIAN_POINT ( 'NONE',  ( 14.57812500061451644, -4.541064518000419881, 2.621784821874995952 ) ) ;
#12493 = EDGE_LOOP ( 'NONE', ( #42371, #23182, #6855, #14243 ) ) ;
#12494 = ORIENTED_EDGE ( 'NONE', *, *, #69679, .F. ) ;
#12495 = CARTESIAN_POINT ( 'NONE',  ( 18.48750000000000071, -2.886751345948125991, -5.000000000000000000 ) ) ;
#12496 = LINE ( 'NONE', #13568, #44467 ) ;
#12497 = CARTESIAN_POINT ( 'NONE',  ( 4.000175247584509819, 2.999766337098574098, 30.13334590365527177 ) ) ;
#12498 = CARTESIAN_POINT ( 'NONE',  ( 15.63750000122903216, 4.330127018922191873, 2.499999999999999556 ) ) ;
#12499 = CARTESIAN_POINT ( 'NONE',  ( 26.78437500061451360, -4.541064518000419881, 2.621784821874995952 ) ) ;
#12500 = CARTESIAN_POINT ( 'NONE',  ( 19.75312500061451360, 4.541064518000418104, -2.621784821874998173 ) ) ;
#12501 = CARTESIAN_POINT ( 'NONE',  ( 23.50312500061451360, 0.000000000000000000, 5.243569643749999010 ) ) ;
#12502 = CARTESIAN_POINT ( 'NONE',  ( 2.990625000614519191, -3.027376345333610441, -5.243569643749999898 ) ) ;
#12503 = CARTESIAN_POINT ( 'NONE',  ( 26.84999999999999787, 0.000000000000000000, 4.999999999999998224 ) ) ;
#12504 = CARTESIAN_POINT ( 'NONE',  ( 21.89999999999999858, 0.000000000000000000, 4.999999999999998224 ) ) ;
#12505 = CARTESIAN_POINT ( 'NONE',  ( 8.446875000614518569, -2.746126346562642428, -4.756430356249999214 ) ) ;
#12506 = CARTESIAN_POINT ( 'NONE',  ( 6.375000001229033764, -5.773502691896255534, -1.060575238724906372E-15 ) ) ;
#12507 = CARTESIAN_POINT ( 'NONE',  ( 3.999999999999999112, 14.37500000000000000, -30.00000000000000000 ) ) ;
#12508 = CARTESIAN_POINT ( 'NONE',  ( -4.243569643749997233, 16.74687500061451928, -27.54997392385601174 ) ) ;
#12509 = CARTESIAN_POINT ( 'NONE',  ( 6.375000001229031987, -5.773502691896255534, -1.060575238724906372E-15 ) ) ;
#12510 = CARTESIAN_POINT ( 'NONE',  ( 5.812500000000001776, -5.773502691896255534, -1.060575238724906372E-15 ) ) ;
#12511 = CARTESIAN_POINT ( 'NONE',  ( 3.000000001229032875, 5.773502691896255534, 3.535250795749688894E-16 ) ) ;
#12512 = CARTESIAN_POINT ( 'NONE',  ( 11.03437500061451715, -4.541064518000419881, 2.621784821874995952 ) ) ;
#12513 = CARTESIAN_POINT ( 'NONE',  ( 24.63750000122903216, 4.330127018922191873, 2.499999999999999556 ) ) ;
#12514 = DIRECTION ( 'NONE',  ( -1.000000000000000000, -0.000000000000000000, -0.000000000000000000 ) ) ;
#12515 = CARTESIAN_POINT ( 'NONE',  ( 8.109375000614518214, 4.541064518000418104, -2.621784821874998173 ) ) ;
#12516 = CARTESIAN_POINT ( 'NONE',  ( 14.14687500061451786, -3.027376345333614438, 5.243569643749998122 ) ) ;
#12517 = CARTESIAN_POINT ( 'NONE',  ( 7.500000000000000000, 0.000000000000000000, 4.999999999999998224 ) ) ;
#12518 = CARTESIAN_POINT ( 'NONE',  ( 2.121784821875001281, 13.65312500061459566, 33.67503911421598417 ) ) ;
#12519 = CARTESIAN_POINT ( 'NONE',  ( 20.48437500061451289, -4.541064518000419881, 2.621784821874995952 ) ) ;
#12520 = CARTESIAN_POINT ( 'NONE',  ( 9.562500000000001776, 2.886751345948129099, -4.999999999999997335 ) ) ;
#12521 = CARTESIAN_POINT ( 'NONE',  ( 26.58750000122903145, -4.330127018922194537, 2.499999999999995559 ) ) ;
#12522 = CARTESIAN_POINT ( 'NONE',  ( 16.65937500061451715, 2.746126346562643317, 4.756430356249998326 ) ) ;
#12523 = CARTESIAN_POINT ( 'NONE',  ( 21.77812500061451928, -4.541064518000419881, 2.621784821874995952 ) ) ;
#12524 = CARTESIAN_POINT ( 'NONE',  ( 11.99062500061451608, -3.027376345333610441, -5.243569643749999898 ) ) ;
#12525 = CARTESIAN_POINT ( 'NONE',  ( 26.93437500061451573, 5.492252693125287522, 3.363034840372157021E-16 ) ) ;
#12526 = CARTESIAN_POINT ( 'NONE',  ( 12.34687500061452070, -3.027376345333614438, 5.243569643749998122 ) ) ;
#12527 = CARTESIAN_POINT ( 'NONE',  ( 27.52500000000000213, 6.123233995736764310E-16, -4.999999999999998224 ) ) ;
#12528 = CARTESIAN_POINT ( 'NONE',  ( 22.87500000122903288, 2.886751345948126879, 4.999999999999999112 ) ) ;
#12529 = CARTESIAN_POINT ( 'NONE',  ( -3.999999999999997335, 18.35000000122903074, -27.69059892324149530 ) ) ;
#12530 = CARTESIAN_POINT ( 'NONE',  ( 11.48437500061451644, -4.541064518000419881, 2.621784821874995952 ) ) ;
#12531 = CARTESIAN_POINT ( 'NONE',  ( 28.05937500061451573, 0.000000000000000000, 5.243569643749999010 ) ) ;
#12532 = CARTESIAN_POINT ( 'NONE',  ( -3.137519842735245283E-14, 11.22500000122903430, 34.00000000000000000 ) ) ;
#12533 = CARTESIAN_POINT ( 'NONE',  ( -1.999999999999997113, 14.67500000000000071, 33.46410161513775705 ) ) ;
#12534 = CARTESIAN_POINT ( 'NONE',  ( 22.95937500061451431, 4.541064518000418104, -2.621784821874998173 ) ) ;
#12535 = CARTESIAN_POINT ( 'NONE',  ( 13.77187500061451786, -6.054752690667223547, -1.112240025338166033E-15 ) ) ;
#12536 = CARTESIAN_POINT ( 'NONE',  ( 3.756430356249998770, 18.56562499938548427, 32.16877607737302469 ) ) ;
#12537 = CARTESIAN_POINT ( 'NONE',  ( 26.13749999999999929, -2.886751345948125991, -5.000000000000000000 ) ) ;
#12538 = CARTESIAN_POINT ( 'NONE',  ( 1.878215178124997609, 19.76562499938548356, 33.25316411605952993 ) ) ;
#12539 = CARTESIAN_POINT ( 'NONE',  ( 26.10937500061451644, 4.119189519843966529, -2.378215178124998275 ) ) ;
#12540 = CARTESIAN_POINT ( 'NONE',  ( 17.84062500061451573, -3.027376345333610441, -5.243569643749999898 ) ) ;
#12541 = CARTESIAN_POINT ( 'NONE',  ( 8.137500000000002842, -2.886751345948125991, -5.000000000000000000 ) ) ;
#12542 = ADVANCED_FACE ( 'NONE', ( #58997 ), #13570, .T. ) ;
#12543 = CARTESIAN_POINT ( 'NONE',  ( 15.78749999999999964, -2.886751345948125991, -5.000000000000000000 ) ) ;
#12544 = CARTESIAN_POINT ( 'NONE',  ( -4.243569643749997233, 10.84062500061451395, 32.45002607614398471 ) ) ;
#12545 = CARTESIAN_POINT ( 'NONE',  ( 0.000000000000000000, 27.50000000000000000, 26.00000000000000000 ) ) ;
#12546 = CARTESIAN_POINT ( 'NONE',  ( 24.42187500061451999, 3.027376345333611329, 5.243569643749999010 ) ) ;
#12547 = ORIENTED_EDGE ( 'NONE', *, *, #8453, .T. ) ;
#12548 = CARTESIAN_POINT ( 'NONE',  ( 21.32812500061451644, -4.541064518000419881, 2.621784821874995952 ) ) ;
#12549 = CARTESIAN_POINT ( 'NONE',  ( 21.00937500061451857, -4.541064518000417216, -2.621784821875001281 ) ) ;
#12550 = CARTESIAN_POINT ( 'NONE',  ( 4.012500000000001954, -5.773502691896255534, -1.060575238724906372E-15 ) ) ;
#12551 = CARTESIAN_POINT ( 'NONE',  ( 6.665625000614515905, 3.027376345333613106, -5.243569643749998122 ) ) ;
#12552 = CARTESIAN_POINT ( 'NONE',  ( 22.56562500061451715, 3.027376345333611329, 5.243569643749999010 ) ) ;
#12553 = CARTESIAN_POINT ( 'NONE',  ( 12.38437500061451857, -4.541064518000419881, 2.621784821874995952 ) ) ;
#12554 = CARTESIAN_POINT ( 'NONE',  ( 17.93437500061451928, 6.421520780324663323E-16, -5.243569643749999010 ) ) ;
#12555 = CARTESIAN_POINT ( 'NONE',  ( -3.000416591977282496E-16, 18.79062500061451857, 25.09994784771203058 ) ) ;
#12556 = CARTESIAN_POINT ( 'NONE',  ( 18.37500000122903288, 2.886751345948126879, 4.999999999999999112 ) ) ;
#12557 = CARTESIAN_POINT ( 'NONE',  ( 14.85937500061451644, 4.119189519843966529, -2.378215178124998275 ) ) ;
#12558 = CARTESIAN_POINT ( 'NONE',  ( 8.840625000614517504, -3.027376345333610441, -5.243569643749999898 ) ) ;
#12559 = CARTESIAN_POINT ( 'NONE',  ( 5.184375000614516615, -4.541064518000419881, 2.621784821874995952 ) ) ;
#12560 = CARTESIAN_POINT ( 'NONE',  ( 5.221875000614519813, -6.054752690667223547, -1.112240025338166033E-15 ) ) ;
#12561 =( BOUNDED_CURVE ( )  B_SPLINE_CURVE ( 3, ( #35577, #7504, #7147, #18207 ),
 .UNSPECIFIED., .F., .F. ) 
 B_SPLINE_CURVE_WITH_KNOTS ( ( 4, 4 ),
 ( 5.667042959702281557, 5.708255309384981047 ),
 .UNSPECIFIED. ) 
 CURVE ( )  GEOMETRIC_REPRESENTATION_ITEM ( )  RATIONAL_B_SPLINE_CURVE ( ( 1.000000000000000000, 0.9998584668609933335, 0.9998584668609933335, 1.000000000000000000 ) ) 
 REPRESENTATION_ITEM ( '' )  );
#12562 = CARTESIAN_POINT ( 'NONE',  ( 25.28437500061451715, 4.541064518000418104, 2.621784821874999949 ) ) ;
#12563 = CARTESIAN_POINT ( 'NONE',  ( 17.27812500061451217, -4.541064518000419881, 2.621784821874995952 ) ) ;
#12564 = CARTESIAN_POINT ( 'NONE',  ( 27.56250000122902932, -4.330127018922190985, -2.500000000000001332 ) ) ;
#12565 = CARTESIAN_POINT ( 'NONE',  ( 26.54062500061451146, 6.054752690667223547, 3.707466751127219781E-16 ) ) ;
#12566 = CARTESIAN_POINT ( 'NONE',  ( 22.77187500061451786, -6.054752690667223547, -1.112240025338166033E-15 ) ) ;
#12567 = CARTESIAN_POINT ( 'NONE',  ( 17.27812500061451217, -4.541064518000419881, 2.621784821874995952 ) ) ;
#12568 = CARTESIAN_POINT ( 'NONE',  ( 4.243569643749999898, 17.38437500061451502, 30.00000000000000000 ) ) ;
#12569 = CARTESIAN_POINT ( 'NONE',  ( 22.37812500061451360, 6.421520780324663323E-16, -5.243569643749999010 ) ) ;
#12570 = CARTESIAN_POINT ( 'NONE',  ( 29.26875000122903003, -5.773502691896255534, -1.060575238724906372E-15 ) ) ;
#12571 = ORIENTED_EDGE ( 'NONE', *, *, #58478, .T. ) ;
#12572 = CARTESIAN_POINT ( 'NONE',  ( 25.08749999999999858, -2.886751345948129988, 4.999999999999997335 ) ) ;
#12573 = CARTESIAN_POINT ( 'NONE',  ( -2.000000000000000000, 13.62500000000000178, -33.46410161513775705 ) ) ;
#12574 = CARTESIAN_POINT ( 'NONE',  ( 11.10000000000000142, 0.000000000000000000, 4.999999999999998224 ) ) ;
#12575 = CARTESIAN_POINT ( 'NONE',  ( 28.11562500061451431, -6.054752690667223547, -1.112240025338166033E-15 ) ) ;
#12576 = CARTESIAN_POINT ( 'NONE',  ( 9.815625000614518925, 3.027376345333613106, -5.243569643749998122 ) ) ;
#12577 = CARTESIAN_POINT ( 'NONE',  ( 23.10000000122903074, -2.886751345948125991, -5.000000000000000000 ) ) ;
#12578 = ADVANCED_FACE ( 'NONE', ( #64550 ), #58635, .F. ) ;
#12579 = CARTESIAN_POINT ( 'NONE',  ( 26.72812500061451502, -4.541064518000419881, 2.621784821874995952 ) ) ;
#12580 = CARTESIAN_POINT ( 'NONE',  ( 28.80000000000000071, -4.330127018922190985, -2.500000000000001332 ) ) ;
#12581 = CARTESIAN_POINT ( 'NONE',  ( -2.828200636599751609E-16, 16.85000000122903430, -34.61880215351700230 ) ) ;
#12582 = CARTESIAN_POINT ( 'NONE',  ( -3.999999999999999112, 15.57500000122903216, -32.30940107675850470 ) ) ;
#12583 = CARTESIAN_POINT ( 'NONE',  ( 9.965625000614517504, 3.027376345333611329, 5.243569643749999010 ) ) ;
#12584 = VERTEX_POINT ( 'NONE', #63464 ) ;
#12585 = CARTESIAN_POINT ( 'NONE',  ( 26.27812500061451573, -4.541064518000419881, 2.621784821874995952 ) ) ;
#12586 = CARTESIAN_POINT ( 'NONE',  ( 8.690625000614515372, -3.027376345333614438, 5.243569643749998122 ) ) ;
#12587 = CARTESIAN_POINT ( 'NONE',  ( 5.878125000614517148, 4.541064518000418104, 2.621784821874999949 ) ) ;
#12588 = VECTOR ( 'NONE', #61286, 1000.000000000000000 ) ;
#12589 = CARTESIAN_POINT ( 'NONE',  ( 15.79687500061451821, 5.492252693125287522, 3.363034840372157021E-16 ) ) ;
#12590 = ADVANCED_FACE ( 'NONE', ( #58268 ), #18742, .T. ) ;
#12591 = DIRECTION ( 'NONE',  ( -1.000000000000000000, -0.000000000000000000, -0.000000000000000000 ) ) ;
#12592 = CARTESIAN_POINT ( 'NONE',  ( 13.38750000000000107, -2.886751345948129988, 4.999999999999997335 ) ) ;
#12593 = CARTESIAN_POINT ( 'NONE',  ( 13.88437500061451679, 6.421520780324663323E-16, -5.243569643749999010 ) ) ;
#12594 = CARTESIAN_POINT ( 'NONE',  ( 10.57500000122903572, 2.886751345948129099, -4.999999999999998224 ) ) ;
#12595 = CARTESIAN_POINT ( 'NONE',  ( 17.82187500061451502, -6.054752690667223547, -1.112240025338166033E-15 ) ) ;
#12596 = CARTESIAN_POINT ( 'NONE',  ( 17.84999999999999787, 0.000000000000000000, 4.999999999999998224 ) ) ;
#12597 = AXIS2_PLACEMENT_3D ( 'NONE', #54500, #43423, #3901 ) ;
#12598 = CARTESIAN_POINT ( 'NONE',  ( 8.371875000614515727, -6.054752690667223547, -1.112240025338166033E-15 ) ) ;
#12599 = CARTESIAN_POINT ( 'NONE',  ( 4.243569643749999010, 12.41562500061451857, -32.45002607614398471 ) ) ;
#12600 = FACE_OUTER_BOUND ( 'NONE', #34654, .T. ) ;
#12601 = CARTESIAN_POINT ( 'NONE',  ( 24.34687500061451715, 0.000000000000000000, 4.756430356249998326 ) ) ;
#12602 = CARTESIAN_POINT ( 'NONE',  ( 24.44062500061451715, -3.027376345333614438, 5.243569643749998122 ) ) ;
#12603 = PLANE ( 'NONE',  #60851 ) ;
#12604 = CARTESIAN_POINT ( 'NONE',  ( 27.75937500061451502, -4.541064518000417216, -2.621784821875001281 ) ) ;
#12605 =( BOUNDED_SURFACE ( )  B_SPLINE_SURFACE ( 1, 2, ( 
 ( #28436, #16612, #68333, #34695, #369, #738, #56154, #11082, #39168, #29525, #22525, #57224, #40615, #17341, #22877, #17693, #62413, #18056, #6638, #51336, #45072, #33610, #5548, #39531, #62056, #18, #11451, #56510, #46156, #28086, #50614, #23970, #45798, #67968, #50973, #1464, #5903, #52060, #45435, #56861, #63136, #34329, #40254, #6267, #28795, #29167, #68696, #51699, #12531, #23247, #35064, #6994, #62775, #1103, #57591, #67254, #53140, #52420, #30975, #12888, #1826, #64589, #42066, #58305, #30248, #2539, #57946, #47240, #18777, #19141, #13244, #14347, #69422, #25059, #46883, #40985, #59037, #13977, #18419, #2903, #47602, #47976, #53510, #36515, #8439, #36881, #63500, #52781, #70132, #41343, #35421, #25434, #70504, #7353, #19881, #19510, #42434, #64955, #59399, #8809, #31346, #29882, #2183, #53886, #3278, #46518, #24334, #36153, #69058, #58672, #24696, #63853, #69773, #35781, #7715, #41695, #64219, #13608, #8080, #30611, #4738, #55343, #26538, #54609, #43533, #48344, #65316, #59771, #20610, #20243, #26168, #48708, #71605, #43900, #27272, #38722, #14706, #26911, #37250, #10274, #44268, #33167, #42795, #60134, #70869, #49437, #66424, #32077, #32441, #9178, #31713, #54248, #61243, #3645, #15802, #72330, #49078, #4014, #71971, #20980, #49805, #38343, #9904, #71231, #43168, #65687, #15075, #37612, #9543, #66054, #15432, #21710, #37977, #60498, #55705, #4382, #54977, #21345, #25806, #60871, #10636, #32806, #66800, #16171, #33520, #6183, #61599, #44989, #23162, #34609, #68250, #57139, #61966, #6548, #17970, #33887, #11000, #45716, #51251, #11728, #56070, #62692, #44639, #5462, #17613, #654, #16891, #11369, #34244, #16529, #5821, #50531, #50889, #67526, #46074, #28002, #67168, #50169, #28352, #34979, #289, #56431, #39445, #45350, #22797, #51617, #73059, #67884, #17256, #40173, #22080, #12088, #28712, #22440, #39816, #29082, #62332, #1018, #56777, #23524, #68609, #40531, #63047, #12448, #5099, #27635, #72698, #39081, #53427, #46799, #6910, #25345, #70419, #7270, #24612, #40903, #47890, #46434, #53057, #19795, #42346, #30530, #64869, #63416, #2817, #18694, #14257, #47159, #41981, #57508, #58948, #19056, #13519, #58587, #36067, #64133, #29441, #23887, #51978, #7994, #12802, #1377, #68973, #41258, #35338, #57861, #29799, #2451, #63770, #69691, #41614, #30162, #64502, #13158, #36434, #18330, #52335, #24974, #47519, #1737, #7625, #35700, #24251, #70048, #19421, #8356, #69336, #58220, #13894, #52695, #2101, #30885, #32352, #3927, #14620, #42709, #26450, #37159, #3559, #14990, #26081, #59685, #65230, #9092, #31629, #3191, #4297, #48620, #60782, #37892, #37528, #71145, #71886, #54890, #20518, #60049, #9820, #31254, #48990, #43076, #26822, #54163, #71520, #59311, #65602, #9460, #31990, #49356, #70779, #54524, #20895, #43449, #53796, #15351, #65971, #20155, #60411, #21259, #43812, #66337, #15715, #38253, #36796, #8721, #25718, #48256, #29674, #59186, #70291, #20025, #25588, #18928, #52210, #70651, #42581, #52571, #69922, #13036, #65107, #18570, #25208, #14497, #37031, #2693, #59555, #35573, #48127, #64007, #1612, #19292, #14131, #24122, #31125, #64374, #58822, #30761, #8232, #36307, #46672, #69212, #41136, #53293, #58093, #63645, #7500, #13388, #30030, #1979, #24488, #47755, #35932, #41846, #13766, #2328, #36667, #58455, #8596, #47032, #69567, #19663, #42217, #41488, #52931, #7867, #30403, #64741, #53666, #3057, #24846, #47392, #32145, #25504, #53580, #8513, #72036, #65025, #54678, #9975, #59845, #42866, #37680, #9250, #60568, #26610, #20681, #14415, #59106, #31042, #8884, #31417, #42502, #36952, #59472, #66123, #2976, #48049, #66489, #15142, #37322, #20313, #43969, #70574, #21412, #19950, #26242, #32512, #53957, #60202, #3354, #25876, #4081, #9614, #48415, #70942, #55048, #71303, #49148, #65389, #31785, #14780, #4450, #26978, #48779, #36586, #15502, #71676, #49508, #54324, #3715, #43239, #65760, #21051, #43602, #38043, #72395, #6250, #4807, #11434, #51318, #722, #62040, #28777, #21776, #34311, #50242, #23228, #5531, #354, #56844, #17324, #50597, #45056, #16959, #67593, #22507, #11794, #55411, #38417, #39512, #44340, #60939, #45781, #72764, #66868, #16238, #38791, #33953, #22149, #28068, #56137, #61666, #22861, #44702, #67952, #15870, #10342, #56494, #1, #61309, #39148, #67236, #32874, #5888, #28419, #39883, #50956, #27339, #16595, #10703, #33237, #45416, #62396, #49870, #55774, #5166, #27701, #11065, #33592, #12872, #52043, #18040, #40597, #35046, #63119, #57206, #69758, #1447, #25044, #7696, #35404, #23952, #13590, #47226, #18402, #57930, #2168, #62758, #24319, #46502, #19126, #12515, #69407, #40235, #34677, #12150, #40969, #68316, #69040, #63484, #57574, #7337, #6977, #41680, #1087, #29508, #29866, #63837, #6621, #58289, #24679, #46867, #64203, #36137, #30233, #52765, #58656, #29149, #52403, #18762, #1811, #41328, #51683, #13228, #30597, #35767, #8063, #53124, #2523, #17676, #68679, #23594, #46140, #71212, #53868, #47959, #26521, #3994, #48325, #3259, #65297, #70116, #13962, #8421, #42417, #42050, #70487, #19864, #20223, #65668, #49059, #60479, #36499, #48688, #59020, #32058, #66038, #54959, #64573, #8792, #19493, #71587, #37959, #9887, #43146, #30957, #53493, #2885, #32422, #25415, #15057, #20960, #70850, #25788, #20589, #42777, #43515, #37595, #31694, #64937, #14328, #36863, #59381, #31325, #14687, #37229, #59752, #15416, #9159, #54229, #4364, #26148, #3626, #60116, #47587, #9526, #54592, #10257, #16511, #22778, #55326, #27983, #32789, #66781, #44969, #56411, #16872, #5802, #10619, #28332, #39797, #55686, #4720, #67507, #73039, #33502, #27254, #11350, #66407, #49787, #39426, #22422, #38705, #33149, #56051, #38325, #27617, #72312, #72681, #16153, #67865, #21693 ),
 ( #50513, #44250, #49419, #56758, #5082, #61225, #50151, #22063, #5443, #44621, #39064, #67151, #61578, #33868, #10981, #50870, #17237, #62313, #61946, #268, #45329, #11709, #34225, #26893, #71952, #21328, #43881, #15783, #60853, #40513, #12067, #51599, #69315, #35678, #35319, #29063, #57118, #57841, #999, #63028, #23867, #12427, #23506, #46055, #68589, #17951, #68230, #7605, #34961, #36045, #18676, #46415, #57488, #24591, #58201, #29423, #68952, #13139, #635, #7250, #6892, #30143, #51958, #29779, #51231, #45697, #23142, #1358, #6163, #18310, #40881, #63397, #12782, #52315, #52674, #34590, #1718, #24230, #46780, #17594, #41238, #63750, #6530, #2082, #47139, #69670, #19036, #41594, #64112, #13498, #28692, #40153, #62672, #58566, #14971, #26062, #48971, #54506, #47868, #7973, #26430, #71500, #8336, #25698, #41959, #20877, #47497, #54145, #43430, #65952, #31608, #15331, #64481, #3908, #19400, #53404, #53036, #58928, #30866, #31234, #3539, #60029, #30509, #24954, #59665, #70028, #43056, #2431, #13874, #36413, #19773, #2796, #9441, #25323, #70397, #48601, #42324, #64849, #14237, #36775, #59291, #71126, #31969, #8701, #53775, #9073, #3171, #48234, #20499, #42689, #70759, #20134, #65211, #14601, #37137, #65581, #37509, #43792, #67426, #32333, #60392, #67780, #16424, #38615, #21608, #45246, #54871, #190, #21240, #27529, #33788, #66319, #38982, #15696, #4638, #55964, #16788, #27897, #39346, #44163, #61859, #50787, #66692, #38235, #5359, #10895, #44535, #60765, #22339, #4277, #10171, #50431, #33423, #49702, #16066, #67067, #49336, #61138, #32706, #10534, #27168, #5720, #55243, #61498, #72229, #26802, #72957, #44891, #9800, #11265, #56331, #28256, #22695, #37873, #71868, #33063, #55601, #4997, #50063, #72593, #21975, #11626, #6804, #52592, #29338, #45968, #69230, #40424, #63307, #17511, #6441, #18591, #40794, #23421, #40072, #41156, #46693, #17865, #68501, #34870, #39712, #56681, #46329, #23777, #13055, #6079, #62230, #12698, #548, #34142, #47053, #913, #23059, #68147, #45614, #68864, #62941, #51868, #57398, #12335, #1634, #51514, #63665, #7521, #30052, #18220, #1270, #62586, #35235, #57756, #1999, #7164, #29693, #35594, #52230, #58113, #24141, #11983, #34506, #24509, #17154, #28611, #57034, #28976, #51148, #41866, #30783, #15151, #53314, #19313, #64396, #36328, #13786, #58476, #72044, #2713, #27349, #9987, #37688, #25229, #15882, #49519, #20690, #60211, #4460, #64028, #26621, #47775, #21422, #58843, #71689, #41508, #35955, #13407, #43249, #69587, #71314, #65769, #8253, #9624, #32157, #43979, #2350, #54690, #4092, #66134, #7888, #60579, #21061, #24866, #47413, #66500, #49158, #32522, #43612, #15512, #38054, #38427, #60950, #55059, #18949, #26990, #10353, #32883, #55423, #4816, #30424, #52952, #69943, #72775, #16967, #33247, #40247, #38802, #45427, #12159, #34687, #22869, #62768, #55785, #68326, #11075, #57218, #39523, #34322, #17686, #51329, #11444, #5896, #50966, #16246, #72405, #362, #5176, #21787, #6631, #33603, #27712, #50252, #22159, #28429, #56147, #62049, #33964, #22518, #56854, #5541, #28788, #49880, #44353, #67961, #56503, #44711, #11, #28079, #66878, #17334, #39893, #731, #62406, #45791, #50607, #67247, #16605, #11805, #6260, #23240, #39161, #61676, #61318, #45065, #67602, #10715, #12881, #52053, #1457, #69050, #23963, #18049, #30605, #35414, #59028, #41688, #46876, #57939, #47595, #8073, #52412, #69415, #36146, #23604, #58298, #7346, #53133, #46511, #30241, #1096, #68689, #46149, #1820, #29160, #29876, #24327, #18412, #18770, #40978, #2532, #35057, #63493, #41336, #24689, #40607, #19134, #52774, #57584, #6987, #25052, #63846, #64211, #13237, #35775, #7707, #70124, #19502, #2176, #51692, #58665, #69766, #42059, #64582, #47233, #63128, #13970, #36508, #13600, #12524, #29518, #71964, #70495, #4006, #43893, #66417, #54601, #21338, #14338, #26904, #42786, #15795, #71222, #66047, #49430, #9896, #43159, #37604, #9535, #60126, #15067, #4375, #48335, #26529, #37969, #71597, #60490, #65307, #32432, #38335, #37241, #36872, #49069, #20972, #32069, #59390, #15425, #47967, #8800, #43525, #54969, #20234, #14697, #8430, #19872, #9169, #53877, #54239, #70860, #30966, #31336, #53501, #3269, #2893, #25424, #42425, #64946, #25797, #59762, #31704, #3636, #26160, #48699, #20600, #65679, #44632, #61957, #67518, #33879, #55336, #50523, #23154, #73051, #16522, #39808, #10992, #56424, #61236, #50161, #62324, #11361, #67161, #10630, #11720, #17248, #61591, #39074, #5454, #10267, #27265, #21703, #55698, #4731, #33160, #5092, #33512, #5813, #34236, #646, #49798, #28344, #72323, #45342, #6174, #68242, #44260, #22073, #32800, #56770, #51243, #45708, #50881, #66793, #16164, #38716, #17605, #27628, #281, #28704, #56061, #27994, #22789, #22433, #60864, #67876, #44981, #72691, #16883, #39437, #12438, #34971, #46066, #40523, #68601, #69683, #34601, #62684, #70040, #18686, #40894, #23879, #47511, #57130, #2443, #23516, #29791, #36058, #17962, #41250, #63039, #19048, #7617, #30522, #58578, #29433, #12080, #7986, #53049, #57500, #7262, #6902, #24966, #29074, #35692, #40165, #6540, #13150, #51609, #51970, #1009, #1369, #46426, #52327, #24603, #68964, #41606, #1729, #69327, #63761, #58212, #46791, #18321, #63408, #12794, #30153, #35330, #57853, #24242, #52687, #2093, #47151, #64125, #13511, #3183, #31622, #59677, #65223, #3920, #53787, #71512, #9813, #32345, #71138, #9085, #42338, #42701, #70771, #54883, #43068, #14983, #20888, #37521, #15344, #25710, #25337, #64861, #9453, #48983, #48613, #14249, #70411, #20511, #36788, #48247, #37152, #20147, #59303, #8714, #31246, #14613, #8348, #43442, #54156, #49349, #31983, #3552, #26074, #37884, #65964, #65594, #60042, #26443, #13886, #54517, #60404 ) ),
 .UNSPECIFIED., .F., .F., .F. ) 
 B_SPLINE_SURFACE_WITH_KNOTS ( ( 2, 2 ),
 ( 3, 2, 2, 2, 2, 2, 2, 2, 2, 2, 2, 2, 2, 2, 2, 2, 2, 2, 2, 2, 2, 2, 2, 2, 2, 2, 2, 2, 2, 2, 2, 2, 2, 2, 2, 2, 2, 2, 2, 2, 2, 2, 2, 2, 2, 2, 2, 2, 2, 2, 2, 2, 2, 2, 2, 2, 2, 2, 2, 2, 2, 2, 2, 2, 2, 2, 2, 2, 2, 2, 2, 2, 2, 2, 2, 2, 2, 2, 2, 2, 2, 2, 2, 2, 2, 2, 2, 2, 2, 2, 2, 2, 2, 2, 2, 2, 2, 2, 2, 2, 2, 2, 2, 2, 2, 2, 2, 2, 2, 2, 2, 2, 2, 2, 2, 2, 2, 2, 2, 2, 2, 2, 2, 2, 2, 2, 2, 2, 2, 2, 2, 2, 2, 2, 2, 2, 2, 2, 2, 2, 2, 2, 2, 2, 2, 2, 2, 2, 2, 2, 2, 2, 2, 2, 2, 2, 2, 2, 2, 2, 2, 2, 2, 2, 2, 2, 2, 2, 2, 2, 2, 2, 2, 2, 2, 2, 2, 2, 2, 2, 2, 2, 2, 2, 2, 2, 2, 2, 2, 2, 2, 2, 2, 2, 2, 2, 2, 2, 2, 2, 2, 2, 2, 2, 2, 2, 2, 2, 2, 2, 2, 2, 2, 2, 2, 2, 2, 2, 2, 2, 2, 2, 2, 2, 2, 2, 2, 2, 2, 2, 2, 2, 2, 2, 2, 2, 2, 2, 2, 2, 2, 2, 2, 2, 2, 2, 2, 2, 2, 2, 2, 2, 2, 2, 2, 2, 2, 2, 2, 2, 2, 2, 2, 2, 2, 2, 2, 2, 2, 2, 2, 2, 2, 2, 2, 2, 2, 2, 2, 2, 2, 2, 2, 2, 2, 2, 2, 2, 2, 2, 2, 2, 2, 2, 2, 2, 2, 2, 2, 2, 2, 2, 2, 2, 2, 2, 2, 2, 2, 2, 2, 2, 2, 2, 2, 2, 2, 2, 2, 2, 2, 2, 2, 2, 2, 2, 2, 2, 2, 2, 2, 2, 2, 2, 2, 2, 2, 2, 2, 2, 2, 2, 2, 2, 2, 2, 2, 2, 2, 2, 2, 2, 2, 2, 2, 2, 2, 2, 2, 2, 3 ),
 ( 0.000000000000000000, 1.000000000000000000 ),
 ( 0.000000000000000000, 0.002777777777777777884, 0.005555555555555555768, 0.008333333333333333218, 0.01111111111111111154, 0.01388888888888888812, 0.01666666666666666644, 0.01944444444444444475, 0.02222222222222222307, 0.02500000000000000139, 0.02777777777777777624, 0.03055555555555555455, 0.03333333333333333287, 0.03611111111111110772, 0.03888888888888888951, 0.04166666666666666435, 0.04444444444444444614, 0.04722222222222222099, 0.05000000000000000278, 0.05277777777777777762, 0.05555555555555555247, 0.05833333333333333426, 0.06111111111111110911, 0.06388888888888888395, 0.06666666666666666574, 0.06944444444444444753, 0.07222222222222221544, 0.07499999999999999722, 0.07777777777777777901, 0.08055555555555556080, 0.08333333333333332871, 0.08611111111111111049, 0.08888888888888889228, 0.09166666666666666019, 0.09444444444444444198, 0.09722222222222222376, 0.1000000000000000056, 0.1027777777777777735, 0.1055555555555555552, 0.1083333333333333370, 0.1111111111111111049, 0.1138888888888888867, 0.1166666666666666685, 0.1194444444444444503, 0.1222222222222222182, 0.1250000000000000000, 0.1277777777777777679, 0.1305555555555555636, 0.1333333333333333315, 0.1361111111111110994, 0.1388888888888888951, 0.1416666666666666630, 0.1444444444444444309, 0.1472222222222222265, 0.1499999999999999944, 0.1527777777777777901, 0.1555555555555555580, 0.1583333333333333259, 0.1611111111111111216, 0.1638888888888888895, 0.1666666666666666574, 0.1694444444444444531, 0.1722222222222222210, 0.1749999999999999889, 0.1777777777777777846, 0.1805555555555555525, 0.1833333333333333204, 0.1861111111111111160, 0.1888888888888888840, 0.1916666666666666796, 0.1944444444444444475, 0.1972222222222222154, 0.2000000000000000111, 0.2027777777777777790, 0.2055555555555555469, 0.2083333333333333426, 0.2111111111111111105, 0.2138888888888888784, 0.2166666666666666741, 0.2194444444444444420, 0.2222222222222222099, 0.2250000000000000056, 0.2277777777777777735, 0.2305555555555555691, 0.2333333333333333370, 0.2361111111111111049, 0.2388888888888889006, 0.2416666666666666685, 0.2444444444444444364, 0.2472222222222222321, 0.2500000000000000000, 0.2527777777777777679, 0.2555555555555555358, 0.2583333333333333592, 0.2611111111111111271, 0.2638888888888888951, 0.2666666666666666630, 0.2694444444444444309, 0.2722222222222221988, 0.2750000000000000222, 0.2777777777777777901, 0.2805555555555555580, 0.2833333333333333259, 0.2861111111111110938, 0.2888888888888888618, 0.2916666666666666852, 0.2944444444444444531, 0.2972222222222222210, 0.2999999999999999889, 0.3027777777777777568, 0.3055555555555555802, 0.3083333333333333481, 0.3111111111111111160, 0.3138888888888888840, 0.3166666666666666519, 0.3194444444444444198, 0.3222222222222222432, 0.3250000000000000111, 0.3277777777777777790, 0.3305555555555555469, 0.3333333333333333148, 0.3361111111111111382, 0.3388888888888889062, 0.3416666666666666741, 0.3444444444444444420, 0.3472222222222222099, 0.3499999999999999778, 0.3527777777777778012, 0.3555555555555555691, 0.3583333333333333370, 0.3611111111111111049, 0.3638888888888888729, 0.3666666666666666408, 0.3694444444444444642, 0.3722222222222222321, 0.3750000000000000000, 0.3777777777777777679, 0.3805555555555555358, 0.3833333333333333592, 0.3861111111111111271, 0.3888888888888888951, 0.3916666666666666630, 0.3944444444444444309, 0.3972222222222221988, 0.4000000000000000222, 0.4027777777777777901, 0.4055555555555555580, 0.4083333333333333259, 0.4111111111111110938, 0.4138888888888888618, 0.4166666666666666852, 0.4194444444444444531, 0.4222222222222222210, 0.4249999999999999889, 0.4277777777777777568, 0.4305555555555555802, 0.4333333333333333481, 0.4361111111111111160, 0.4388888888888888840, 0.4416666666666666519, 0.4444444444444444198, 0.4472222222222222432, 0.4500000000000000111, 0.4527777777777777790, 0.4555555555555555469, 0.4583333333333333148, 0.4611111111111111382, 0.4638888888888889062, 0.4666666666666666741, 0.4694444444444444420, 0.4722222222222222099, 0.4749999999999999778, 0.4777777777777778012, 0.4805555555555555691, 0.4833333333333333370, 0.4861111111111111049, 0.4888888888888888729, 0.4916666666666666408, 0.4944444444444444642, 0.4972222222222222321, 0.5000000000000000000, 0.5027777777777777679, 0.5055555555555555358, 0.5083333333333333037, 0.5111111111111110716, 0.5138888888888888395, 0.5166666666666667185, 0.5194444444444444864, 0.5222222222222222543, 0.5250000000000000222, 0.5277777777777777901, 0.5305555555555555580, 0.5333333333333333259, 0.5361111111111110938, 0.5388888888888888618, 0.5416666666666666297, 0.5444444444444443976, 0.5472222222222222765, 0.5500000000000000444, 0.5527777777777778123, 0.5555555555555555802, 0.5583333333333333481, 0.5611111111111111160, 0.5638888888888888840, 0.5666666666666666519, 0.5694444444444444198, 0.5722222222222221877, 0.5749999999999999556, 0.5777777777777777235, 0.5805555555555556024, 0.5833333333333333703, 0.5861111111111111382, 0.5888888888888889062, 0.5916666666666666741, 0.5944444444444444420, 0.5972222222222222099, 0.5999999999999999778, 0.6027777777777777457, 0.6055555555555555136, 0.6083333333333332815, 0.6111111111111111605, 0.6138888888888889284, 0.6166666666666666963, 0.6194444444444444642, 0.6222222222222222321, 0.6250000000000000000, 0.6277777777777777679, 0.6305555555555555358, 0.6333333333333333037, 0.6361111111111110716, 0.6388888888888888395, 0.6416666666666667185, 0.6444444444444444864, 0.6472222222222222543, 0.6500000000000000222, 0.6527777777777777901, 0.6555555555555555580, 0.6583333333333333259, 0.6611111111111110938, 0.6638888888888888618, 0.6666666666666666297, 0.6694444444444443976, 0.6722222222222222765, 0.6750000000000000444, 0.6777777777777778123, 0.6805555555555555802, 0.6833333333333333481, 0.6861111111111111160, 0.6888888888888888840, 0.6916666666666666519, 0.6944444444444444198, 0.6972222222222221877, 0.6999999999999999556, 0.7027777777777777235, 0.7055555555555556024, 0.7083333333333333703, 0.7111111111111111382, 0.7138888888888889062, 0.7166666666666666741, 0.7194444444444444420, 0.7222222222222222099, 0.7249999999999999778, 0.7277777777777777457, 0.7305555555555555136, 0.7333333333333332815, 0.7361111111111111605, 0.7388888888888889284, 0.7416666666666666963, 0.7444444444444444642, 0.7472222222222222321, 0.7500000000000000000, 0.7527777777777777679, 0.7555555555555555358, 0.7583333333333333037, 0.7611111111111110716, 0.7638888888888888395, 0.7666666666666667185, 0.7694444444444444864, 0.7722222222222222543, 0.7750000000000000222, 0.7777777777777777901, 0.7805555555555555580, 0.7833333333333333259, 0.7861111111111110938, 0.7888888888888888618, 0.7916666666666666297, 0.7944444444444443976, 0.7972222222222222765, 0.8000000000000000444, 0.8027777777777778123, 0.8055555555555555802, 0.8083333333333333481, 0.8111111111111111160, 0.8138888888888888840, 0.8166666666666666519, 0.8194444444444444198, 0.8222222222222221877, 0.8249999999999999556, 0.8277777777777777235, 0.8305555555555556024, 0.8333333333333333703, 0.8361111111111111382, 0.8388888888888889062, 0.8416666666666666741, 0.8444444444444444420, 0.8472222222222222099, 0.8499999999999999778, 0.8527777777777777457, 0.8555555555555555136, 0.8583333333333332815, 0.8611111111111111605, 0.8638888888888889284, 0.8666666666666666963, 0.8694444444444444642, 0.8722222222222222321, 0.8750000000000000000, 0.8777777777777777679, 0.8805555555555555358, 0.8833333333333333037, 0.8861111111111110716, 0.8888888888888888395, 0.8916666666666667185, 0.8944444444444444864, 0.8972222222222222543, 0.9000000000000000222, 0.9027777777777777901, 0.9055555555555555580, 0.9083333333333333259, 0.9111111111111110938, 0.9138888888888888618, 0.9166666666666666297, 0.9194444444444443976, 0.9222222222222222765, 0.9250000000000000444, 0.9277777777777778123, 0.9305555555555555802, 0.9333333333333333481, 0.9361111111111111160, 0.9388888888888888840, 0.9416666666666666519, 0.9444444444444444198, 0.9472222222222221877, 0.9499999999999999556, 0.9527777777777777235, 0.9555555555555556024, 0.9583333333333333703, 0.9611111111111111382, 0.9638888888888889062, 0.9666666666666666741, 0.9694444444444444420, 0.9722222222222222099, 0.9749999999999999778, 0.9777777777777777457, 0.9805555555555555136, 0.9833333333333332815, 0.9861111111111111605, 0.9888888888888889284, 0.9916666666666666963, 0.9944444444444444642, 0.9972222222222222321, 1.000000000000000000 ),
 .UNSPECIFIED. ) 
 GEOMETRIC_REPRESENTATION_ITEM ( )  RATIONAL_B_SPLINE_SURFACE ( (
 ( 1.000000000000000000, 0.8660254037844387076, 1.000000000000000000, 0.8660254037844387076, 1.000000000000000000, 0.8660254037844387076, 1.000000000000000000, 0.8660254037844387076, 1.000000000000000000, 0.8660254037844387076, 1.000000000000000000, 0.8660254037844387076, 1.000000000000000000, 0.8660254037844387076, 1.000000000000000000, 0.8660254037844387076, 1.000000000000000000, 0.8660254037844387076, 1.000000000000000000, 0.8660254037844387076, 1.000000000000000000, 0.8660254037844387076, 1.000000000000000000, 0.8660254037844387076, 1.000000000000000000, 0.8660254037844387076, 1.000000000000000000, 0.8660254037844387076, 1.000000000000000000, 0.8660254037844387076, 1.000000000000000000, 0.8660254037844387076, 1.000000000000000000, 0.8660254037844387076, 1.000000000000000000, 0.8660254037844387076, 1.000000000000000000, 0.8660254037844387076, 1.000000000000000000, 0.8660254037844387076, 1.000000000000000000, 0.8660254037844387076, 1.000000000000000000, 0.8660254037844387076, 1.000000000000000000, 0.8660254037844387076, 1.000000000000000000, 0.8660254037844387076, 1.000000000000000000, 0.8660254037844387076, 1.000000000000000000, 0.8660254037844387076, 1.000000000000000000, 0.8660254037844387076, 1.000000000000000000, 0.8660254037844387076, 1.000000000000000000, 0.8660254037844387076, 1.000000000000000000, 0.8660254037844387076, 1.000000000000000000, 0.8660254037844387076, 1.000000000000000000, 0.8660254037844387076, 1.000000000000000000, 0.8660254037844387076, 1.000000000000000000, 0.8660254037844387076, 1.000000000000000000, 0.8660254037844387076, 1.000000000000000000, 0.8660254037844387076, 1.000000000000000000, 0.8660254037844387076, 1.000000000000000000, 0.8660254037844387076, 1.000000000000000000, 0.8660254037844387076, 1.000000000000000000, 0.8660254037844387076, 1.000000000000000000, 0.8660254037844387076, 1.000000000000000000, 0.8660254037844387076, 1.000000000000000000, 0.8660254037844387076, 1.000000000000000000, 0.8660254037844387076, 1.000000000000000000, 0.8660254037844387076, 1.000000000000000000, 0.8660254037844387076, 1.000000000000000000, 0.8660254037844387076, 1.000000000000000000, 0.8660254037844387076, 1.000000000000000000, 0.8660254037844387076, 1.000000000000000000, 0.8660254037844387076, 1.000000000000000000, 0.8660254037844387076, 1.000000000000000000, 0.8660254037844387076, 1.000000000000000000, 0.8660254037844387076, 1.000000000000000000, 0.8660254037844387076, 1.000000000000000000, 0.8660254037844387076, 1.000000000000000000, 0.8660254037844387076, 1.000000000000000000, 0.8660254037844387076, 1.000000000000000000, 0.8660254037844387076, 1.000000000000000000, 0.8660254037844387076, 1.000000000000000000, 0.8660254037844387076, 1.000000000000000000, 0.8660254037844387076, 1.000000000000000000, 0.8660254037844387076, 1.000000000000000000, 0.8660254037844387076, 1.000000000000000000, 0.8660254037844387076, 1.000000000000000000, 0.8660254037844387076, 1.000000000000000000, 0.8660254037844387076, 1.000000000000000000, 0.8660254037844387076, 1.000000000000000000, 0.8660254037844387076, 1.000000000000000000, 0.8660254037844387076, 1.000000000000000000, 0.8660254037844387076, 1.000000000000000000, 0.8660254037844387076, 1.000000000000000000, 0.8660254037844387076, 1.000000000000000000, 0.8660254037844387076, 1.000000000000000000, 0.8660254037844387076, 1.000000000000000000, 0.8660254037844387076, 1.000000000000000000, 0.8660254037844387076, 1.000000000000000000, 0.8660254037844387076, 1.000000000000000000, 0.8660254037844387076, 1.000000000000000000, 0.8660254037844387076, 1.000000000000000000, 0.8660254037844387076, 1.000000000000000000, 0.8660254037844387076, 1.000000000000000000, 0.8660254037844387076, 1.000000000000000000, 0.8660254037844387076, 1.000000000000000000, 0.8660254037844387076, 1.000000000000000000, 0.8660254037844387076, 1.000000000000000000, 0.8660254037844387076, 1.000000000000000000, 0.8660254037844387076, 1.000000000000000000, 0.8660254037844387076, 1.000000000000000000, 0.8660254037844387076, 1.000000000000000000, 0.8660254037844387076, 1.000000000000000000, 0.8660254037844387076, 1.000000000000000000, 0.8660254037844387076, 1.000000000000000000, 0.8660254037844387076, 1.000000000000000000, 0.8660254037844387076, 1.000000000000000000, 0.8660254037844387076, 1.000000000000000000, 0.8660254037844387076, 1.000000000000000000, 0.8660254037844387076, 1.000000000000000000, 0.8660254037844387076, 1.000000000000000000, 0.8660254037844387076, 1.000000000000000000, 0.8660254037844387076, 1.000000000000000000, 0.8660254037844387076, 1.000000000000000000, 0.8660254037844387076, 1.000000000000000000, 0.8660254037844387076, 1.000000000000000000, 0.8660254037844387076, 1.000000000000000000, 0.8660254037844387076, 1.000000000000000000, 0.8660254037844387076, 1.000000000000000000, 0.8660254037844387076, 1.000000000000000000, 0.8660254037844387076, 1.000000000000000000, 0.8660254037844387076, 1.000000000000000000, 0.8660254037844387076, 1.000000000000000000, 0.8660254037844387076, 1.000000000000000000, 0.8660254037844387076, 1.000000000000000000, 0.8660254037844387076, 1.000000000000000000, 0.8660254037844387076, 1.000000000000000000, 0.8660254037844387076, 1.000000000000000000, 0.8660254037844387076, 1.000000000000000000, 0.8660254037844387076, 1.000000000000000000, 0.8660254037844387076, 1.000000000000000000, 0.8660254037844387076, 1.000000000000000000, 0.8660254037844387076, 1.000000000000000000, 0.8660254037844387076, 1.000000000000000000, 0.8660254037844387076, 1.000000000000000000, 0.8660254037844387076, 1.000000000000000000, 0.8660254037844387076, 1.000000000000000000, 0.8660254037844387076, 1.000000000000000000, 0.8660254037844387076, 1.000000000000000000, 0.8660254037844387076, 1.000000000000000000, 0.8660254037844387076, 1.000000000000000000, 0.8660254037844387076, 1.000000000000000000, 0.8660254037844387076, 1.000000000000000000, 0.8660254037844387076, 1.000000000000000000, 0.8660254037844387076, 1.000000000000000000, 0.8660254037844387076, 1.000000000000000000, 0.8660254037844387076, 1.000000000000000000, 0.8660254037844387076, 1.000000000000000000, 0.8660254037844387076, 1.000000000000000000, 0.8660254037844387076, 1.000000000000000000, 0.8660254037844387076, 1.000000000000000000, 0.8660254037844387076, 1.000000000000000000, 0.8660254037844387076, 1.000000000000000000, 0.8660254037844387076, 1.000000000000000000, 0.8660254037844387076, 1.000000000000000000, 0.8660254037844387076, 1.000000000000000000, 0.8660254037844387076, 1.000000000000000000, 0.8660254037844387076, 1.000000000000000000, 0.8660254037844387076, 1.000000000000000000, 0.8660254037844387076, 1.000000000000000000, 0.8660254037844387076, 1.000000000000000000, 0.8660254037844387076, 1.000000000000000000, 0.8660254037844387076, 1.000000000000000000, 0.8660254037844387076, 1.000000000000000000, 0.8660254037844387076, 1.000000000000000000, 0.8660254037844387076, 1.000000000000000000, 0.8660254037844387076, 1.000000000000000000, 0.8660254037844387076, 1.000000000000000000, 0.8660254037844387076, 1.000000000000000000, 0.8660254037844387076, 1.000000000000000000, 0.8660254037844387076, 1.000000000000000000, 0.8660254037844387076, 1.000000000000000000, 0.8660254037844387076, 1.000000000000000000, 0.8660254037844387076, 1.000000000000000000, 0.8660254037844387076, 1.000000000000000000, 0.8660254037844387076, 1.000000000000000000, 0.8660254037844387076, 1.000000000000000000, 0.8660254037844387076, 1.000000000000000000, 0.8660254037844387076, 1.000000000000000000, 0.8660254037844387076, 1.000000000000000000, 0.8660254037844387076, 1.000000000000000000, 0.8660254037844387076, 1.000000000000000000, 0.8660254037844387076, 1.000000000000000000, 0.8660254037844387076, 1.000000000000000000, 0.8660254037844387076, 1.000000000000000000, 0.8660254037844387076, 1.000000000000000000, 0.8660254037844387076, 1.000000000000000000, 0.8660254037844387076, 1.000000000000000000, 0.8660254037844387076, 1.000000000000000000, 0.8660254037844387076, 1.000000000000000000, 0.8660254037844387076, 1.000000000000000000, 0.8660254037844387076, 1.000000000000000000, 0.8660254037844387076, 1.000000000000000000, 0.8660254037844387076, 1.000000000000000000, 0.8660254037844387076, 1.000000000000000000, 0.8660254037844387076, 1.000000000000000000, 0.8660254037844387076, 1.000000000000000000, 0.8660254037844387076, 1.000000000000000000, 0.8660254037844387076, 1.000000000000000000, 0.8660254037844387076, 1.000000000000000000, 0.8660254037844387076, 1.000000000000000000, 0.8660254037844387076, 1.000000000000000000, 0.8660254037844387076, 1.000000000000000000, 0.8660254037844387076, 1.000000000000000000, 0.8660254037844387076, 1.000000000000000000, 0.8660254037844387076, 1.000000000000000000, 0.8660254037844387076, 1.000000000000000000, 0.8660254037844387076, 1.000000000000000000, 0.8660254037844387076, 1.000000000000000000, 0.8660254037844387076, 1.000000000000000000, 0.8660254037844387076, 1.000000000000000000, 0.8660254037844387076, 1.000000000000000000, 0.8660254037844387076, 1.000000000000000000, 0.8660254037844387076, 1.000000000000000000, 0.8660254037844387076, 1.000000000000000000, 0.8660254037844387076, 1.000000000000000000, 0.8660254037844387076, 1.000000000000000000, 0.8660254037844387076, 1.000000000000000000, 0.8660254037844387076, 1.000000000000000000, 0.8660254037844387076, 1.000000000000000000, 0.8660254037844387076, 1.000000000000000000, 0.8660254037844387076, 1.000000000000000000, 0.8660254037844387076, 1.000000000000000000, 0.8660254037844387076, 1.000000000000000000, 0.8660254037844387076, 1.000000000000000000, 0.8660254037844387076, 1.000000000000000000, 0.8660254037844387076, 1.000000000000000000, 0.8660254037844387076, 1.000000000000000000, 0.8660254037844387076, 1.000000000000000000, 0.8660254037844387076, 1.000000000000000000, 0.8660254037844387076, 1.000000000000000000, 0.8660254037844387076, 1.000000000000000000, 0.8660254037844387076, 1.000000000000000000, 0.8660254037844387076, 1.000000000000000000, 0.8660254037844387076, 1.000000000000000000, 0.8660254037844387076, 1.000000000000000000, 0.8660254037844387076, 1.000000000000000000, 0.8660254037844387076, 1.000000000000000000, 0.8660254037844387076, 1.000000000000000000, 0.8660254037844387076, 1.000000000000000000, 0.8660254037844387076, 1.000000000000000000, 0.8660254037844387076, 1.000000000000000000, 0.8660254037844387076, 1.000000000000000000, 0.8660254037844387076, 1.000000000000000000, 0.8660254037844387076, 1.000000000000000000, 0.8660254037844387076, 1.000000000000000000, 0.8660254037844387076, 1.000000000000000000, 0.8660254037844387076, 1.000000000000000000, 0.8660254037844387076, 1.000000000000000000, 0.8660254037844387076, 1.000000000000000000, 0.8660254037844387076, 1.000000000000000000, 0.8660254037844387076, 1.000000000000000000, 0.8660254037844387076, 1.000000000000000000, 0.8660254037844387076, 1.000000000000000000, 0.8660254037844387076, 1.000000000000000000, 0.8660254037844387076, 1.000000000000000000, 0.8660254037844387076, 1.000000000000000000, 0.8660254037844387076, 1.000000000000000000, 0.8660254037844387076, 1.000000000000000000, 0.8660254037844387076, 1.000000000000000000, 0.8660254037844387076, 1.000000000000000000, 0.8660254037844387076, 1.000000000000000000, 0.8660254037844387076, 1.000000000000000000, 0.8660254037844387076, 1.000000000000000000, 0.8660254037844387076, 1.000000000000000000, 0.8660254037844387076, 1.000000000000000000, 0.8660254037844387076, 1.000000000000000000, 0.8660254037844387076, 1.000000000000000000, 0.8660254037844387076, 1.000000000000000000, 0.8660254037844387076, 1.000000000000000000, 0.8660254037844387076, 1.000000000000000000, 0.8660254037844387076, 1.000000000000000000, 0.8660254037844387076, 1.000000000000000000, 0.8660254037844387076, 1.000000000000000000, 0.8660254037844387076, 1.000000000000000000, 0.8660254037844387076, 1.000000000000000000, 0.8660254037844387076, 1.000000000000000000, 0.8660254037844387076, 1.000000000000000000, 0.8660254037844387076, 1.000000000000000000, 0.8660254037844387076, 1.000000000000000000, 0.8660254037844387076, 1.000000000000000000, 0.8660254037844387076, 1.000000000000000000, 0.8660254037844387076, 1.000000000000000000, 0.8660254037844387076, 1.000000000000000000, 0.8660254037844387076, 1.000000000000000000, 0.8660254037844387076, 1.000000000000000000, 0.8660254037844387076, 1.000000000000000000, 0.8660254037844387076, 1.000000000000000000, 0.8660254037844387076, 1.000000000000000000, 0.8660254037844387076, 1.000000000000000000, 0.8660254037844387076, 1.000000000000000000, 0.8660254037844387076, 1.000000000000000000, 0.8660254037844387076, 1.000000000000000000, 0.8660254037844387076, 1.000000000000000000, 0.8660254037844387076, 1.000000000000000000, 0.8660254037844387076, 1.000000000000000000, 0.8660254037844387076, 1.000000000000000000, 0.8660254037844387076, 1.000000000000000000, 0.8660254037844387076, 1.000000000000000000, 0.8660254037844387076, 1.000000000000000000, 0.8660254037844387076, 1.000000000000000000, 0.8660254037844387076, 1.000000000000000000, 0.8660254037844387076, 1.000000000000000000, 0.8660254037844387076, 1.000000000000000000, 0.8660254037844387076, 1.000000000000000000, 0.8660254037844387076, 1.000000000000000000, 0.8660254037844387076, 1.000000000000000000, 0.8660254037844387076, 1.000000000000000000, 0.8660254037844387076, 1.000000000000000000, 0.8660254037844387076, 1.000000000000000000, 0.8660254037844387076, 1.000000000000000000, 0.8660254037844387076, 1.000000000000000000, 0.8660254037844387076, 1.000000000000000000, 0.8660254037844387076, 1.000000000000000000, 0.8660254037844387076, 1.000000000000000000, 0.8660254037844387076, 1.000000000000000000, 0.8660254037844387076, 1.000000000000000000, 0.8660254037844387076, 1.000000000000000000, 0.8660254037844387076, 1.000000000000000000, 0.8660254037844387076, 1.000000000000000000, 0.8660254037844387076, 1.000000000000000000, 0.8660254037844387076, 1.000000000000000000, 0.8660254037844387076, 1.000000000000000000, 0.8660254037844387076, 1.000000000000000000, 0.8660254037844387076, 1.000000000000000000, 0.8660254037844387076, 1.000000000000000000, 0.8660254037844387076, 1.000000000000000000, 0.8660254037844387076, 1.000000000000000000, 0.8660254037844387076, 1.000000000000000000, 0.8660254037844387076, 1.000000000000000000, 0.8660254037844387076, 1.000000000000000000, 0.8660254037844387076, 1.000000000000000000, 0.8660254037844387076, 1.000000000000000000, 0.8660254037844387076, 1.000000000000000000, 0.8660254037844387076, 1.000000000000000000, 0.8660254037844387076, 1.000000000000000000, 0.8660254037844387076, 1.000000000000000000, 0.8660254037844387076, 1.000000000000000000, 0.8660254037844387076, 1.000000000000000000, 0.8660254037844387076, 1.000000000000000000, 0.8660254037844387076, 1.000000000000000000, 0.8660254037844387076, 1.000000000000000000, 0.8660254037844387076, 1.000000000000000000, 0.8660254037844387076, 1.000000000000000000, 0.8660254037844387076, 1.000000000000000000, 0.8660254037844387076, 1.000000000000000000, 0.8660254037844387076, 1.000000000000000000, 0.8660254037844387076, 1.000000000000000000, 0.8660254037844387076, 1.000000000000000000, 0.8660254037844387076, 1.000000000000000000, 0.8660254037844387076, 1.000000000000000000, 0.8660254037844387076, 1.000000000000000000, 0.8660254037844387076, 1.000000000000000000, 0.8660254037844387076, 1.000000000000000000, 0.8660254037844387076, 1.000000000000000000, 0.8660254037844387076, 1.000000000000000000, 0.8660254037844387076, 1.000000000000000000, 0.8660254037844387076, 1.000000000000000000, 0.8660254037844387076, 1.000000000000000000, 0.8660254037844387076, 1.000000000000000000, 0.8660254037844387076, 1.000000000000000000, 0.8660254037844387076, 1.000000000000000000, 0.8660254037844387076, 1.000000000000000000, 0.8660254037844387076, 1.000000000000000000, 0.8660254037844387076, 1.000000000000000000, 0.8660254037844387076, 1.000000000000000000, 0.8660254037844387076, 1.000000000000000000, 0.8660254037844387076, 1.000000000000000000, 0.8660254037844387076, 1.000000000000000000, 0.8660254037844387076, 1.000000000000000000, 0.8660254037844387076, 1.000000000000000000, 0.8660254037844387076, 1.000000000000000000, 0.8660254037844387076, 1.000000000000000000),
 ( 1.000000000000000000, 0.8660254037844387076, 1.000000000000000000, 0.8660254037844387076, 1.000000000000000000, 0.8660254037844387076, 1.000000000000000000, 0.8660254037844387076, 1.000000000000000000, 0.8660254037844387076, 1.000000000000000000, 0.8660254037844387076, 1.000000000000000000, 0.8660254037844387076, 1.000000000000000000, 0.8660254037844387076, 1.000000000000000000, 0.8660254037844387076, 1.000000000000000000, 0.8660254037844387076, 1.000000000000000000, 0.8660254037844387076, 1.000000000000000000, 0.8660254037844387076, 1.000000000000000000, 0.8660254037844387076, 1.000000000000000000, 0.8660254037844387076, 1.000000000000000000, 0.8660254037844387076, 1.000000000000000000, 0.8660254037844387076, 1.000000000000000000, 0.8660254037844387076, 1.000000000000000000, 0.8660254037844387076, 1.000000000000000000, 0.8660254037844387076, 1.000000000000000000, 0.8660254037844387076, 1.000000000000000000, 0.8660254037844387076, 1.000000000000000000, 0.8660254037844387076, 1.000000000000000000, 0.8660254037844387076, 1.000000000000000000, 0.8660254037844387076, 1.000000000000000000, 0.8660254037844387076, 1.000000000000000000, 0.8660254037844387076, 1.000000000000000000, 0.8660254037844387076, 1.000000000000000000, 0.8660254037844387076, 1.000000000000000000, 0.8660254037844387076, 1.000000000000000000, 0.8660254037844387076, 1.000000000000000000, 0.8660254037844387076, 1.000000000000000000, 0.8660254037844387076, 1.000000000000000000, 0.8660254037844387076, 1.000000000000000000, 0.8660254037844387076, 1.000000000000000000, 0.8660254037844387076, 1.000000000000000000, 0.8660254037844387076, 1.000000000000000000, 0.8660254037844387076, 1.000000000000000000, 0.8660254037844387076, 1.000000000000000000, 0.8660254037844387076, 1.000000000000000000, 0.8660254037844387076, 1.000000000000000000, 0.8660254037844387076, 1.000000000000000000, 0.8660254037844387076, 1.000000000000000000, 0.8660254037844387076, 1.000000000000000000, 0.8660254037844387076, 1.000000000000000000, 0.8660254037844387076, 1.000000000000000000, 0.8660254037844387076, 1.000000000000000000, 0.8660254037844387076, 1.000000000000000000, 0.8660254037844387076, 1.000000000000000000, 0.8660254037844387076, 1.000000000000000000, 0.8660254037844387076, 1.000000000000000000, 0.8660254037844387076, 1.000000000000000000, 0.8660254037844387076, 1.000000000000000000, 0.8660254037844387076, 1.000000000000000000, 0.8660254037844387076, 1.000000000000000000, 0.8660254037844387076, 1.000000000000000000, 0.8660254037844387076, 1.000000000000000000, 0.8660254037844387076, 1.000000000000000000, 0.8660254037844387076, 1.000000000000000000, 0.8660254037844387076, 1.000000000000000000, 0.8660254037844387076, 1.000000000000000000, 0.8660254037844387076, 1.000000000000000000, 0.8660254037844387076, 1.000000000000000000, 0.8660254037844387076, 1.000000000000000000, 0.8660254037844387076, 1.000000000000000000, 0.8660254037844387076, 1.000000000000000000, 0.8660254037844387076, 1.000000000000000000, 0.8660254037844387076, 1.000000000000000000, 0.8660254037844387076, 1.000000000000000000, 0.8660254037844387076, 1.000000000000000000, 0.8660254037844387076, 1.000000000000000000, 0.8660254037844387076, 1.000000000000000000, 0.8660254037844387076, 1.000000000000000000, 0.8660254037844387076, 1.000000000000000000, 0.8660254037844387076, 1.000000000000000000, 0.8660254037844387076, 1.000000000000000000, 0.8660254037844387076, 1.000000000000000000, 0.8660254037844387076, 1.000000000000000000, 0.8660254037844387076, 1.000000000000000000, 0.8660254037844387076, 1.000000000000000000, 0.8660254037844387076, 1.000000000000000000, 0.8660254037844387076, 1.000000000000000000, 0.8660254037844387076, 1.000000000000000000, 0.8660254037844387076, 1.000000000000000000, 0.8660254037844387076, 1.000000000000000000, 0.8660254037844387076, 1.000000000000000000, 0.8660254037844387076, 1.000000000000000000, 0.8660254037844387076, 1.000000000000000000, 0.8660254037844387076, 1.000000000000000000, 0.8660254037844387076, 1.000000000000000000, 0.8660254037844387076, 1.000000000000000000, 0.8660254037844387076, 1.000000000000000000, 0.8660254037844387076, 1.000000000000000000, 0.8660254037844387076, 1.000000000000000000, 0.8660254037844387076, 1.000000000000000000, 0.8660254037844387076, 1.000000000000000000, 0.8660254037844387076, 1.000000000000000000, 0.8660254037844387076, 1.000000000000000000, 0.8660254037844387076, 1.000000000000000000, 0.8660254037844387076, 1.000000000000000000, 0.8660254037844387076, 1.000000000000000000, 0.8660254037844387076, 1.000000000000000000, 0.8660254037844387076, 1.000000000000000000, 0.8660254037844387076, 1.000000000000000000, 0.8660254037844387076, 1.000000000000000000, 0.8660254037844387076, 1.000000000000000000, 0.8660254037844387076, 1.000000000000000000, 0.8660254037844387076, 1.000000000000000000, 0.8660254037844387076, 1.000000000000000000, 0.8660254037844387076, 1.000000000000000000, 0.8660254037844387076, 1.000000000000000000, 0.8660254037844387076, 1.000000000000000000, 0.8660254037844387076, 1.000000000000000000, 0.8660254037844387076, 1.000000000000000000, 0.8660254037844387076, 1.000000000000000000, 0.8660254037844387076, 1.000000000000000000, 0.8660254037844387076, 1.000000000000000000, 0.8660254037844387076, 1.000000000000000000, 0.8660254037844387076, 1.000000000000000000, 0.8660254037844387076, 1.000000000000000000, 0.8660254037844387076, 1.000000000000000000, 0.8660254037844387076, 1.000000000000000000, 0.8660254037844387076, 1.000000000000000000, 0.8660254037844387076, 1.000000000000000000, 0.8660254037844387076, 1.000000000000000000, 0.8660254037844387076, 1.000000000000000000, 0.8660254037844387076, 1.000000000000000000, 0.8660254037844387076, 1.000000000000000000, 0.8660254037844387076, 1.000000000000000000, 0.8660254037844387076, 1.000000000000000000, 0.8660254037844387076, 1.000000000000000000, 0.8660254037844387076, 1.000000000000000000, 0.8660254037844387076, 1.000000000000000000, 0.8660254037844387076, 1.000000000000000000, 0.8660254037844387076, 1.000000000000000000, 0.8660254037844387076, 1.000000000000000000, 0.8660254037844387076, 1.000000000000000000, 0.8660254037844387076, 1.000000000000000000, 0.8660254037844387076, 1.000000000000000000, 0.8660254037844387076, 1.000000000000000000, 0.8660254037844387076, 1.000000000000000000, 0.8660254037844387076, 1.000000000000000000, 0.8660254037844387076, 1.000000000000000000, 0.8660254037844387076, 1.000000000000000000, 0.8660254037844387076, 1.000000000000000000, 0.8660254037844387076, 1.000000000000000000, 0.8660254037844387076, 1.000000000000000000, 0.8660254037844387076, 1.000000000000000000, 0.8660254037844387076, 1.000000000000000000, 0.8660254037844387076, 1.000000000000000000, 0.8660254037844387076, 1.000000000000000000, 0.8660254037844387076, 1.000000000000000000, 0.8660254037844387076, 1.000000000000000000, 0.8660254037844387076, 1.000000000000000000, 0.8660254037844387076, 1.000000000000000000, 0.8660254037844387076, 1.000000000000000000, 0.8660254037844387076, 1.000000000000000000, 0.8660254037844387076, 1.000000000000000000, 0.8660254037844387076, 1.000000000000000000, 0.8660254037844387076, 1.000000000000000000, 0.8660254037844387076, 1.000000000000000000, 0.8660254037844387076, 1.000000000000000000, 0.8660254037844387076, 1.000000000000000000, 0.8660254037844387076, 1.000000000000000000, 0.8660254037844387076, 1.000000000000000000, 0.8660254037844387076, 1.000000000000000000, 0.8660254037844387076, 1.000000000000000000, 0.8660254037844387076, 1.000000000000000000, 0.8660254037844387076, 1.000000000000000000, 0.8660254037844387076, 1.000000000000000000, 0.8660254037844387076, 1.000000000000000000, 0.8660254037844387076, 1.000000000000000000, 0.8660254037844387076, 1.000000000000000000, 0.8660254037844387076, 1.000000000000000000, 0.8660254037844387076, 1.000000000000000000, 0.8660254037844387076, 1.000000000000000000, 0.8660254037844387076, 1.000000000000000000, 0.8660254037844387076, 1.000000000000000000, 0.8660254037844387076, 1.000000000000000000, 0.8660254037844387076, 1.000000000000000000, 0.8660254037844387076, 1.000000000000000000, 0.8660254037844387076, 1.000000000000000000, 0.8660254037844387076, 1.000000000000000000, 0.8660254037844387076, 1.000000000000000000, 0.8660254037844387076, 1.000000000000000000, 0.8660254037844387076, 1.000000000000000000, 0.8660254037844387076, 1.000000000000000000, 0.8660254037844387076, 1.000000000000000000, 0.8660254037844387076, 1.000000000000000000, 0.8660254037844387076, 1.000000000000000000, 0.8660254037844387076, 1.000000000000000000, 0.8660254037844387076, 1.000000000000000000, 0.8660254037844387076, 1.000000000000000000, 0.8660254037844387076, 1.000000000000000000, 0.8660254037844387076, 1.000000000000000000, 0.8660254037844387076, 1.000000000000000000, 0.8660254037844387076, 1.000000000000000000, 0.8660254037844387076, 1.000000000000000000, 0.8660254037844387076, 1.000000000000000000, 0.8660254037844387076, 1.000000000000000000, 0.8660254037844387076, 1.000000000000000000, 0.8660254037844387076, 1.000000000000000000, 0.8660254037844387076, 1.000000000000000000, 0.8660254037844387076, 1.000000000000000000, 0.8660254037844387076, 1.000000000000000000, 0.8660254037844387076, 1.000000000000000000, 0.8660254037844387076, 1.000000000000000000, 0.8660254037844387076, 1.000000000000000000, 0.8660254037844387076, 1.000000000000000000, 0.8660254037844387076, 1.000000000000000000, 0.8660254037844387076, 1.000000000000000000, 0.8660254037844387076, 1.000000000000000000, 0.8660254037844387076, 1.000000000000000000, 0.8660254037844387076, 1.000000000000000000, 0.8660254037844387076, 1.000000000000000000, 0.8660254037844387076, 1.000000000000000000, 0.8660254037844387076, 1.000000000000000000, 0.8660254037844387076, 1.000000000000000000, 0.8660254037844387076, 1.000000000000000000, 0.8660254037844387076, 1.000000000000000000, 0.8660254037844387076, 1.000000000000000000, 0.8660254037844387076, 1.000000000000000000, 0.8660254037844387076, 1.000000000000000000, 0.8660254037844387076, 1.000000000000000000, 0.8660254037844387076, 1.000000000000000000, 0.8660254037844387076, 1.000000000000000000, 0.8660254037844387076, 1.000000000000000000, 0.8660254037844387076, 1.000000000000000000, 0.8660254037844387076, 1.000000000000000000, 0.8660254037844387076, 1.000000000000000000, 0.8660254037844387076, 1.000000000000000000, 0.8660254037844387076, 1.000000000000000000, 0.8660254037844387076, 1.000000000000000000, 0.8660254037844387076, 1.000000000000000000, 0.8660254037844387076, 1.000000000000000000, 0.8660254037844387076, 1.000000000000000000, 0.8660254037844387076, 1.000000000000000000, 0.8660254037844387076, 1.000000000000000000, 0.8660254037844387076, 1.000000000000000000, 0.8660254037844387076, 1.000000000000000000, 0.8660254037844387076, 1.000000000000000000, 0.8660254037844387076, 1.000000000000000000, 0.8660254037844387076, 1.000000000000000000, 0.8660254037844387076, 1.000000000000000000, 0.8660254037844387076, 1.000000000000000000, 0.8660254037844387076, 1.000000000000000000, 0.8660254037844387076, 1.000000000000000000, 0.8660254037844387076, 1.000000000000000000, 0.8660254037844387076, 1.000000000000000000, 0.8660254037844387076, 1.000000000000000000, 0.8660254037844387076, 1.000000000000000000, 0.8660254037844387076, 1.000000000000000000, 0.8660254037844387076, 1.000000000000000000, 0.8660254037844387076, 1.000000000000000000, 0.8660254037844387076, 1.000000000000000000, 0.8660254037844387076, 1.000000000000000000, 0.8660254037844387076, 1.000000000000000000, 0.8660254037844387076, 1.000000000000000000, 0.8660254037844387076, 1.000000000000000000, 0.8660254037844387076, 1.000000000000000000, 0.8660254037844387076, 1.000000000000000000, 0.8660254037844387076, 1.000000000000000000, 0.8660254037844387076, 1.000000000000000000, 0.8660254037844387076, 1.000000000000000000, 0.8660254037844387076, 1.000000000000000000, 0.8660254037844387076, 1.000000000000000000, 0.8660254037844387076, 1.000000000000000000, 0.8660254037844387076, 1.000000000000000000, 0.8660254037844387076, 1.000000000000000000, 0.8660254037844387076, 1.000000000000000000, 0.8660254037844387076, 1.000000000000000000, 0.8660254037844387076, 1.000000000000000000, 0.8660254037844387076, 1.000000000000000000, 0.8660254037844387076, 1.000000000000000000, 0.8660254037844387076, 1.000000000000000000, 0.8660254037844387076, 1.000000000000000000, 0.8660254037844387076, 1.000000000000000000, 0.8660254037844387076, 1.000000000000000000, 0.8660254037844387076, 1.000000000000000000, 0.8660254037844387076, 1.000000000000000000, 0.8660254037844387076, 1.000000000000000000, 0.8660254037844387076, 1.000000000000000000, 0.8660254037844387076, 1.000000000000000000, 0.8660254037844387076, 1.000000000000000000, 0.8660254037844387076, 1.000000000000000000, 0.8660254037844387076, 1.000000000000000000, 0.8660254037844387076, 1.000000000000000000, 0.8660254037844387076, 1.000000000000000000, 0.8660254037844387076, 1.000000000000000000, 0.8660254037844387076, 1.000000000000000000, 0.8660254037844387076, 1.000000000000000000, 0.8660254037844387076, 1.000000000000000000, 0.8660254037844387076, 1.000000000000000000, 0.8660254037844387076, 1.000000000000000000, 0.8660254037844387076, 1.000000000000000000, 0.8660254037844387076, 1.000000000000000000, 0.8660254037844387076, 1.000000000000000000, 0.8660254037844387076, 1.000000000000000000, 0.8660254037844387076, 1.000000000000000000, 0.8660254037844387076, 1.000000000000000000, 0.8660254037844387076, 1.000000000000000000, 0.8660254037844387076, 1.000000000000000000, 0.8660254037844387076, 1.000000000000000000, 0.8660254037844387076, 1.000000000000000000, 0.8660254037844387076, 1.000000000000000000, 0.8660254037844387076, 1.000000000000000000, 0.8660254037844387076, 1.000000000000000000, 0.8660254037844387076, 1.000000000000000000, 0.8660254037844387076, 1.000000000000000000, 0.8660254037844387076, 1.000000000000000000, 0.8660254037844387076, 1.000000000000000000, 0.8660254037844387076, 1.000000000000000000, 0.8660254037844387076, 1.000000000000000000, 0.8660254037844387076, 1.000000000000000000, 0.8660254037844387076, 1.000000000000000000, 0.8660254037844387076, 1.000000000000000000, 0.8660254037844387076, 1.000000000000000000, 0.8660254037844387076, 1.000000000000000000, 0.8660254037844387076, 1.000000000000000000, 0.8660254037844387076, 1.000000000000000000, 0.8660254037844387076, 1.000000000000000000, 0.8660254037844387076, 1.000000000000000000, 0.8660254037844387076, 1.000000000000000000, 0.8660254037844387076, 1.000000000000000000, 0.8660254037844387076, 1.000000000000000000, 0.8660254037844387076, 1.000000000000000000, 0.8660254037844387076, 1.000000000000000000, 0.8660254037844387076, 1.000000000000000000, 0.8660254037844387076, 1.000000000000000000, 0.8660254037844387076, 1.000000000000000000, 0.8660254037844387076, 1.000000000000000000, 0.8660254037844387076, 1.000000000000000000, 0.8660254037844387076, 1.000000000000000000, 0.8660254037844387076, 1.000000000000000000, 0.8660254037844387076, 1.000000000000000000, 0.8660254037844387076, 1.000000000000000000, 0.8660254037844387076, 1.000000000000000000, 0.8660254037844387076, 1.000000000000000000, 0.8660254037844387076, 1.000000000000000000, 0.8660254037844387076, 1.000000000000000000, 0.8660254037844387076, 1.000000000000000000, 0.8660254037844387076, 1.000000000000000000, 0.8660254037844387076, 1.000000000000000000, 0.8660254037844387076, 1.000000000000000000, 0.8660254037844387076, 1.000000000000000000, 0.8660254037844387076, 1.000000000000000000, 0.8660254037844387076, 1.000000000000000000, 0.8660254037844387076, 1.000000000000000000, 0.8660254037844387076, 1.000000000000000000, 0.8660254037844387076, 1.000000000000000000, 0.8660254037844387076, 1.000000000000000000, 0.8660254037844387076, 1.000000000000000000, 0.8660254037844387076, 1.000000000000000000, 0.8660254037844387076, 1.000000000000000000, 0.8660254037844387076, 1.000000000000000000, 0.8660254037844387076, 1.000000000000000000, 0.8660254037844387076, 1.000000000000000000, 0.8660254037844387076, 1.000000000000000000, 0.8660254037844387076, 1.000000000000000000, 0.8660254037844387076, 1.000000000000000000, 0.8660254037844387076, 1.000000000000000000) ) ) 
 REPRESENTATION_ITEM ( '' )  SURFACE ( )  );
#12606 = CARTESIAN_POINT ( 'NONE',  ( 23.88749999999999929, -2.886751345948125991, -5.000000000000000000 ) ) ;
#12607 = CARTESIAN_POINT ( 'NONE',  ( 5.728125000614515905, 6.421520780324663323E-16, -5.243569643749999010 ) ) ;
#12608 = CARTESIAN_POINT ( 'NONE',  ( 25.65937500061451360, 2.746126346562643317, 4.756430356249998326 ) ) ;
#12609 = CARTESIAN_POINT ( 'NONE',  ( 18.23437500061451999, -4.541064518000419881, 2.621784821874995952 ) ) ;
#12610 = CARTESIAN_POINT ( 'NONE',  ( 11.29687500061451644, 0.000000000000000000, 4.756430356249998326 ) ) ;
#12611 = CARTESIAN_POINT ( 'NONE',  ( 28.65000000122903145, 5.773502691896255534, 3.535250795749688894E-16 ) ) ;
#12612 = CARTESIAN_POINT ( 'NONE',  ( 8.521875000614516082, 3.027376345333613106, -5.243569643749998122 ) ) ;
#12613 = EDGE_LOOP ( 'NONE', ( #39256, #69680, #8711, #65709 ) ) ;
#12614 = CARTESIAN_POINT ( 'NONE',  ( 18.49687500061452283, 6.054752690667223547, 3.707466751127219781E-16 ) ) ;
#12615 = FACE_OUTER_BOUND ( 'NONE', #37835, .T. ) ;
#12616 = CARTESIAN_POINT ( 'NONE',  ( 27.00000000000000000, -4.330127018922190985, -2.500000000000001332 ) ) ;
#12617 = CARTESIAN_POINT ( 'NONE',  ( 3.525000000000000355, -4.330127018922194537, 2.499999999999995559 ) ) ;
#12618 = CARTESIAN_POINT ( 'NONE',  ( 12.46875000122903288, 2.886751345948126879, 4.999999999999998224 ) ) ;
#12619 = ORIENTED_EDGE ( 'NONE', *, *, #72365, .T. ) ;
#12620 = CARTESIAN_POINT ( 'NONE',  ( 9.487500000000000711, -2.886751345948125991, -5.000000000000000000 ) ) ;
#12621 = CARTESIAN_POINT ( 'NONE',  ( 12.49687500061451573, 4.119189519843966529, -2.378215178124998275 ) ) ;
#12622 = CARTESIAN_POINT ( 'NONE',  ( 25.52812500061451573, 6.421520780324663323E-16, -5.243569643749999010 ) ) ;
#12623 = CARTESIAN_POINT ( 'NONE',  ( 15.33750000000000036, -2.886751345948125991, -5.000000000000000000 ) ) ;
#12624 = CARTESIAN_POINT ( 'NONE',  ( 10.91250000122903252, -4.330127018922190985, -2.500000000000001332 ) ) ;
#12625 = CARTESIAN_POINT ( 'NONE',  ( 8.315625000614515372, -6.054752690667223547, -1.112240025338166033E-15 ) ) ;
#12626 = CARTESIAN_POINT ( 'NONE',  ( 22.38749999999999929, -2.886751345948129988, 4.999999999999997335 ) ) ;
#12627 = CARTESIAN_POINT ( 'NONE',  ( 20.46562500061451928, -6.054752690667223547, -1.112240025338166033E-15 ) ) ;
#12628 = DIRECTION ( 'NONE',  ( -1.000000000000000000, -0.000000000000000000, -0.000000000000000000 ) ) ;
#12629 = CARTESIAN_POINT ( 'NONE',  ( 26.55000000122902648, -2.886751345948129988, 4.999999999999997335 ) ) ;
#12630 = CARTESIAN_POINT ( 'NONE',  ( 3.756430356249998770, 17.55312499938548498, 32.16877607737301759 ) ) ;
#12631 = CARTESIAN_POINT ( 'NONE',  ( 5.587500000000003020, 5.773502691896255534, 3.535250795749688894E-16 ) ) ;
#12632 = VERTEX_POINT ( 'NONE', #47938 ) ;
#12633 = CARTESIAN_POINT ( 'NONE',  ( 21.62812500061451360, 4.541064518000418104, 2.621784821874999949 ) ) ;
#12634 = CARTESIAN_POINT ( 'NONE',  ( 29.35312500061451502, 0.000000000000000000, 5.243569643749999010 ) ) ;
#12635 = CARTESIAN_POINT ( 'NONE',  ( 28.39687500061452141, 6.054752690667223547, 3.707466751127219781E-16 ) ) ;
#12636 = CARTESIAN_POINT ( 'NONE',  ( 19.43437500061451928, 4.541064518000418104, 2.621784821874999949 ) ) ;
#12637 = CARTESIAN_POINT ( 'NONE',  ( 15.36562500061451608, 3.027376345333611329, 5.243569643749999010 ) ) ;
#12638 = CARTESIAN_POINT ( 'NONE',  ( -1.473776270879187500, 9.816672227264625405, -34.04916702557058983 ) ) ;
#12639 = CARTESIAN_POINT ( 'NONE',  ( 25.38750000122903216, 6.123233995736764310E-16, -4.999999999999998224 ) ) ;
#12640 = CARTESIAN_POINT ( 'NONE',  ( 22.09687500061451715, 5.492252693125287522, 3.363034840372157021E-16 ) ) ;
#12641 = CARTESIAN_POINT ( 'NONE',  ( 17.46562500061451217, 3.027376345333612662, -5.243569643749998122 ) ) ;
#12642 = CARTESIAN_POINT ( 'NONE',  ( 4.537500001229034297, -4.330127018922194537, 2.499999999999995559 ) ) ;
#12643 = CARTESIAN_POINT ( 'NONE',  ( 12.15937500061451892, 4.541064518000418104, -2.621784821874998173 ) ) ;
#12644 = CARTESIAN_POINT ( 'NONE',  ( 12.49687500061451573, -3.027376345333610441, -5.243569643749999898 ) ) ;
#12645 = CARTESIAN_POINT ( 'NONE',  ( 20.82187500061451857, 3.027376345333611329, 5.243569643749999010 ) ) ;
#12646 = ORIENTED_EDGE ( 'NONE', *, *, #54952, .F. ) ;
#12647 = CARTESIAN_POINT ( 'NONE',  ( 24.03750000122903430, 6.123233995736764310E-16, -4.999999999999998224 ) ) ;
#12648 = CARTESIAN_POINT ( 'NONE',  ( 23.35312500061451857, 4.541064518000418104, -2.621784821874998173 ) ) ;
#12649 = CARTESIAN_POINT ( 'NONE',  ( 19.13437500061451857, -4.541064518000419881, 2.621784821874995952 ) ) ;
#12650 = CARTESIAN_POINT ( 'NONE',  ( 25.00312500061451715, -4.541064518000417216, -2.621784821875001281 ) ) ;
#12651 = LINE ( 'NONE', #24458, #26226 ) ;
#12652 = CARTESIAN_POINT ( 'NONE',  ( 4.000000000000000000, 15.23750000000000071, 32.30940107675849049 ) ) ;
#12653 = CARTESIAN_POINT ( 'NONE',  ( 3.421875000614516882, -6.054752690667223547, -1.112240025338166033E-15 ) ) ;
#12654 = CARTESIAN_POINT ( 'NONE',  ( 8.775000001229033231, 2.886751345948129099, -4.999999999999998224 ) ) ;
#12655 = CARTESIAN_POINT ( 'NONE',  ( 4.800000001229032698, 5.773502691896255534, 3.535250795749688894E-16 ) ) ;
#12656 = CARTESIAN_POINT ( 'NONE',  ( -5.810221930991193690E-16, 11.90000000122903501, -34.00000000000000000 ) ) ;
#12657 = CARTESIAN_POINT ( 'NONE',  ( 27.90000000122903145, -2.886751345948129988, 4.999999999999997335 ) ) ;
#12658 = CARTESIAN_POINT ( 'NONE',  ( 3.756430356250000102, 13.65312499938548285, 30.00000000000000000 ) ) ;
#12659 = CARTESIAN_POINT ( 'NONE',  ( 16.81875000122903430, 2.886751345948129099, -4.999999999999998224 ) ) ;
#12660 = CARTESIAN_POINT ( 'NONE',  ( 10.50937500061451679, 0.000000000000000000, 5.243569643749999010 ) ) ;
#12661 = CARTESIAN_POINT ( 'NONE',  ( 10.25625000122903252, 0.000000000000000000, 4.999999999999998224 ) ) ;
#12662 = CARTESIAN_POINT ( 'NONE',  ( 16.82812500061451644, -4.541064518000419881, 2.621784821874995952 ) ) ;
#12663 = CARTESIAN_POINT ( 'NONE',  ( 10.99687500061451750, -3.027376345333614438, 5.243569643749998122 ) ) ;
#12664 = CARTESIAN_POINT ( 'NONE',  ( 2.915625000614516793, -6.054752690667223547, -1.112240025338166033E-15 ) ) ;
#12665 = CARTESIAN_POINT ( 'NONE',  ( 19.02187500061451786, 3.027376345333611329, 5.243569643749999010 ) ) ;
#12666 = CARTESIAN_POINT ( 'NONE',  ( 7.659375000614518036, 4.541064518000418104, -2.621784821874998173 ) ) ;
#12667 = CARTESIAN_POINT ( 'NONE',  ( 3.440625000614518036, -3.027376345333610441, -5.243569643749999898 ) ) ;
#12668 = CARTESIAN_POINT ( 'NONE',  ( -1.071796769724488563, 17.84240381056766367, 34.00000000000000000 ) ) ;
#12669 = CARTESIAN_POINT ( 'NONE',  ( 7.003125000614518036, -4.541064518000417216, -2.621784821875001281 ) ) ;
#12670 = CARTESIAN_POINT ( 'NONE',  ( 17.57812500061451644, 4.541064518000418104, 2.621784821874999949 ) ) ;
#12671 = ORIENTED_EDGE ( 'NONE', *, *, #24843, .F. ) ;
#12672 = CARTESIAN_POINT ( 'NONE',  ( 5.437500001229035540, -4.330127018922194537, 2.499999999999995559 ) ) ;
#12673 = CARTESIAN_POINT ( 'NONE',  ( 15.32812500061451644, 4.541064518000418104, 2.621784821874999949 ) ) ;
#12674 = CARTESIAN_POINT ( 'NONE',  ( 13.71562500061451750, -6.054752690667223547, -1.112240025338166033E-15 ) ) ;
#12675 = CARTESIAN_POINT ( 'NONE',  ( 22.73437500061451644, -4.119189519843968306, 2.378215178124996054 ) ) ;
#12676 = CARTESIAN_POINT ( 'NONE',  ( 12.97499999999999964, -4.330127018922194537, 2.499999999999995559 ) ) ;
#12677 = EDGE_CURVE ( 'NONE', #32974, #71417, #5616, .T. ) ;
#12678 = CARTESIAN_POINT ( 'NONE',  ( 7.462500001229035007, 4.330127018922192761, -2.499999999999997780 ) ) ;
#12679 = CARTESIAN_POINT ( 'NONE',  ( 3.965625000614515727, 3.027376345333613106, -5.243569643749998122 ) ) ;
#12680 = CARTESIAN_POINT ( 'NONE',  ( 18.63750000122903216, 6.123233995736764310E-16, -4.999999999999998224 ) ) ;
#12681 = CARTESIAN_POINT ( 'NONE',  ( 25.31250000000000000, 2.886751345948129099, -4.999999999999998224 ) ) ;
#12682 = CARTESIAN_POINT ( 'NONE',  ( 2.121784821874999061, 12.05937500061451750, -33.67503911421598417 ) ) ;
#12683 = CARTESIAN_POINT ( 'NONE',  ( -4.000000000000000888, 14.50624999877096499, 32.30940107675850470 ) ) ;
#12684 = CARTESIAN_POINT ( 'NONE',  ( 28.93125000122903145, 6.123233995736764310E-16, -4.999999999999998224 ) ) ;
#12685 = CARTESIAN_POINT ( 'NONE',  ( 6.524999999999999467, 4.330127018922191873, 2.499999999999999556 ) ) ;
#12686 = CARTESIAN_POINT ( 'NONE',  ( -3.999999999999997335, 13.28749999999999964, 32.30940107675850470 ) ) ;
#12687 = CARTESIAN_POINT ( 'NONE',  ( 17.55937500061451573, 4.541064518000418104, -2.621784821874998173 ) ) ;
#12688 = AXIS2_PLACEMENT_3D ( 'NONE', #49599, #54408, #43693 ) ;
#12689 = CARTESIAN_POINT ( 'NONE',  ( 14.87812500061451537, 4.541064518000418104, 2.621784821874999949 ) ) ;
#12690 = CARTESIAN_POINT ( 'NONE',  ( 10.29375000122903216, -2.886751345948129988, 4.999999999999997335 ) ) ;
#12691 = CARTESIAN_POINT ( 'NONE',  ( -1.071796769724491005, 14.62009619066136779, 26.00000000000000355 ) ) ;
#12692 = CARTESIAN_POINT ( 'NONE',  ( 26.55937500061451573, 4.541064518000418104, -2.621784821874998173 ) ) ;
#12693 = CARTESIAN_POINT ( 'NONE',  ( 18.30937500061451573, 2.746126346562645981, -4.756430356249997438 ) ) ;
#12694 = CARTESIAN_POINT ( 'NONE',  ( 12.21562500061451573, 3.027376345333611329, 5.243569643749999010 ) ) ;
#12695 = CARTESIAN_POINT ( 'NONE',  ( 15.23437500061451644, 6.421520780324663323E-16, -5.243569643749999010 ) ) ;
#12696 = ORIENTED_EDGE ( 'NONE', *, *, #31768, .T. ) ;
#12697 = CARTESIAN_POINT ( 'NONE',  ( 27.21562500061451928, -6.054752690667223547, -1.112240025338166033E-15 ) ) ;
#12698 = CARTESIAN_POINT ( 'NONE',  ( 20.54062500061451502, -3.027376345333610441, -5.243569643749999898 ) ) ;
#12699 = CARTESIAN_POINT ( 'NONE',  ( 3.132876461932173395, 3.896812063161361195, -3.508551012645405365 ) ) ;
#12700 = CARTESIAN_POINT ( 'NONE',  ( -3.137519842735245283E-14, 14.37500000122903288, -26.00000000000000711 ) ) ;
#12701 = CARTESIAN_POINT ( 'NONE',  ( 9.037499999999999645, -2.886751345948125991, -5.000000000000000000 ) ) ;
#12702 = CARTESIAN_POINT ( 'NONE',  ( 18.33750000122903501, 4.330127018922191873, 2.499999999999999556 ) ) ;
#12703 = CYLINDRICAL_SURFACE ( 'NONE', #54933, 10.00000000000000000 ) ;
#12704 = CARTESIAN_POINT ( 'NONE',  ( 11.29687500061451644, 0.000000000000000000, 4.756430356249998326 ) ) ;
#12705 = ORIENTED_EDGE ( 'NONE', *, *, #54021, .F. ) ;
#12706 = CARTESIAN_POINT ( 'NONE',  ( 18.63749999999999929, 5.773502691896255534, 3.535250795749688894E-16 ) ) ;
#12707 = CARTESIAN_POINT ( 'NONE',  ( 22.42500000000000071, -4.330127018922194537, 2.499999999999995559 ) ) ;
#12708 = CARTESIAN_POINT ( 'NONE',  ( 19.99687500061451573, -3.027376345333614438, 5.243569643749998122 ) ) ;
#12709 = CARTESIAN_POINT ( 'NONE',  ( 24.40312500061451573, 0.000000000000000000, 5.243569643749999010 ) ) ;
#12710 = EDGE_CURVE ( 'NONE', #32129, #48891, #57907, .T. ) ;
#12711 = EDGE_LOOP ( 'NONE', ( #15487, #48728, #57141, #62009 ) ) ;
#12712 = CARTESIAN_POINT ( 'NONE',  ( 8.775000001229031454, 2.886751345948062486, -5.000000000000113687 ) ) ;
#12713 = CARTESIAN_POINT ( 'NONE',  ( 5.615625000614517859, -6.054752690667223547, -1.112240025338166033E-15 ) ) ;
#12714 = CARTESIAN_POINT ( 'NONE',  ( 13.91249999999999964, -5.773502691896255534, -1.060575238724906372E-15 ) ) ;
#12715 = CARTESIAN_POINT ( 'NONE',  ( -3.000416591977282496E-16, 16.54062500061451857, 25.09994784771203058 ) ) ;
#12716 = CARTESIAN_POINT ( 'NONE',  ( 29.16562500061451502, 3.027376345333613106, -5.243569643749998122 ) ) ;
#12717 = CARTESIAN_POINT ( 'NONE',  ( 11.73750000000000249, -2.886751345948125991, -5.000000000000000000 ) ) ;
#12718 = CARTESIAN_POINT ( 'NONE',  ( 3.756430356250000102, 18.49062499938548143, 30.00000000000000000 ) ) ;
#12719 = CARTESIAN_POINT ( 'NONE',  ( 25.20937500061451431, 4.541064518000418104, -2.621784821874998173 ) ) ;
#12720 = ORIENTED_EDGE ( 'NONE', *, *, #12941, .T. ) ;
#12721 = CARTESIAN_POINT ( 'NONE',  ( 20.87812500061451715, -4.541064518000419881, 2.621784821874995952 ) ) ;
#12722 = CARTESIAN_POINT ( 'NONE',  ( 22.47187500061451715, 3.027376345333613106, -5.243569643749998122 ) ) ;
#12723 = CARTESIAN_POINT ( 'NONE',  ( -2.121784821874999949, 17.02812500061459744, -33.67503911421598417 ) ) ;
#12724 = CARTESIAN_POINT ( 'NONE',  ( 7.153125000614518392, 4.541064518000418104, -2.621784821874998173 ) ) ;
#12725 = CARTESIAN_POINT ( 'NONE',  ( 29.03437500061451715, -4.119189519843968306, 2.378215178124996054 ) ) ;
#12726 = CARTESIAN_POINT ( 'NONE',  ( 22.86562500061451431, 3.027376345333612662, -5.243569643749998122 ) ) ;
#12727 = CARTESIAN_POINT ( 'NONE',  ( 28.02187500061451431, -4.119189519843968306, 2.378215178124996054 ) ) ;
#12728 = CARTESIAN_POINT ( 'NONE',  ( 12.30937500061451573, 0.000000000000000000, 4.756430356249998326 ) ) ;
#12729 = CARTESIAN_POINT ( 'NONE',  ( 16.28437500061452070, 4.541064518000418104, 2.621784821874999949 ) ) ;
#12730 = CARTESIAN_POINT ( 'NONE',  ( 20.07187500061451857, -6.054752690667223547, -1.112240025338166033E-15 ) ) ;
#12731 = CARTESIAN_POINT ( 'NONE',  ( 26.97187500061451360, 3.027376345333613106, -5.243569643749998122 ) ) ;
#12732 = CARTESIAN_POINT ( 'NONE',  ( 4.243569643749999898, 15.58437500061451786, 30.00000000000000000 ) ) ;
#12733 = CARTESIAN_POINT ( 'NONE',  ( 7.865625000614516971, -6.054752690667223547, -1.112240025338166033E-15 ) ) ;
#12734 = CARTESIAN_POINT ( 'NONE',  ( -1.999999999999997113, 19.17500000000000071, 33.46410161513775705 ) ) ;
#12735 = CARTESIAN_POINT ( 'NONE',  ( 5.746875000614517504, -3.027376345333610441, -5.243569643749999898 ) ) ;
#12736 = DIRECTION ( 'NONE',  ( -1.000000000000000000, -0.000000000000000000, -0.000000000000000000 ) ) ;
#12737 = CARTESIAN_POINT ( 'NONE',  ( 5.203125000614518214, -4.541064518000417216, -2.621784821875001281 ) ) ;
#12738 = CARTESIAN_POINT ( 'NONE',  ( 8.671875000614518214, 3.027376345333611329, 5.243569643749999010 ) ) ;
#12739 =( LENGTH_UNIT ( ) NAMED_UNIT ( * ) SI_UNIT ( .MILLI., .METRE. ) );
#12740 = CARTESIAN_POINT ( 'NONE',  ( 16.83750000122903145, 6.123233995736764310E-16, -4.999999999999998224 ) ) ;
#12741 = CARTESIAN_POINT ( 'NONE',  ( 4.921875000614518214, 3.027376345333613106, -5.243569643749998122 ) ) ;
#12742 = CARTESIAN_POINT ( 'NONE',  ( 7.003125000614518036, -4.541064518000417216, -2.621784821875001281 ) ) ;
#12743 = CARTESIAN_POINT ( 'NONE',  ( -8.484601909799255319E-16, 13.23124999877096641, 34.61880215351700940 ) ) ;
#12744 = CARTESIAN_POINT ( 'NONE',  ( 22.74375000122903145, 5.773502691896255534, 3.535250795749688894E-16 ) ) ;
#12745 = CARTESIAN_POINT ( 'NONE',  ( 16.13437500061451502, 6.421520780324663323E-16, -5.243569643749999010 ) ) ;
#12746 = CARTESIAN_POINT ( 'NONE',  ( 22.57499999999999929, 6.123233995736764310E-16, -4.999999999999998224 ) ) ;
#12747 = VERTEX_POINT ( 'NONE', #52382 ) ;
#12748 = CARTESIAN_POINT ( 'NONE',  ( 25.30312500061451431, 0.000000000000000000, 5.243569643749999010 ) ) ;
#12749 = CARTESIAN_POINT ( 'NONE',  ( 8.765625000614518214, -6.054752690667223547, -1.112240025338166033E-15 ) ) ;
#12750 = AXIS2_PLACEMENT_3D ( 'NONE', #56498, #6627, #16601 ) ;
#12751 = CARTESIAN_POINT ( 'NONE',  ( 28.13437500061451502, -4.541064518000419881, 2.621784821874995952 ) ) ;
#12752 = CARTESIAN_POINT ( 'NONE',  ( 9.815625000614518925, 3.027376345333613106, -5.243569643749998122 ) ) ;
#12753 = CARTESIAN_POINT ( 'NONE',  ( 4.243569643749999898, 10.18437500061451750, -30.00000000000000000 ) ) ;
#12754 = CARTESIAN_POINT ( 'NONE',  ( 11.55000000122903181, 5.773502691896255534, 3.535250795749688894E-16 ) ) ;
#12755 = CARTESIAN_POINT ( 'NONE',  ( 25.79062500061451502, -3.027376345333614438, 5.243569643749998122 ) ) ;
#12756 = CARTESIAN_POINT ( 'NONE',  ( 4.243569643749999898, 12.82812500061451821, -30.00000000000000000 ) ) ;
#12757 = CARTESIAN_POINT ( 'NONE',  ( 11.85000000122903430, -2.886751345948125991, -5.000000000000000000 ) ) ;
#12758 = CARTESIAN_POINT ( 'NONE',  ( 22.71562500061451573, -6.054752690667223547, -1.112240025338166033E-15 ) ) ;
#12759 = CARTESIAN_POINT ( 'NONE',  ( 11.36250000000000071, 2.886751345948129099, -4.999999999999998224 ) ) ;
#12760 = CARTESIAN_POINT ( 'NONE',  ( 21.44062500061452070, -3.027376345333610441, -5.243569643749999898 ) ) ;
#12761 = CARTESIAN_POINT ( 'NONE',  ( 5.484375000614518214, 4.541064518000418104, 2.621784821874999949 ) ) ;
#12762 = CARTESIAN_POINT ( 'NONE',  ( 20.96250000000000213, 2.886751345948126879, 4.999999999999999112 ) ) ;
#12763 = CARTESIAN_POINT ( 'NONE',  ( 16.68750000122903288, -4.330127018922194537, 2.499999999999995559 ) ) ;
#12764 = CARTESIAN_POINT ( 'NONE',  ( 13.15312500061451750, 0.000000000000000000, 5.243569643749999010 ) ) ;
#12765 =( BOUNDED_CURVE ( )  B_SPLINE_CURVE ( 2, ( #60075, #65997, #26849, #43839, #3953, #43102, #60808 ),
 .UNSPECIFIED., .F., .F. ) 
 B_SPLINE_CURVE_WITH_KNOTS ( ( 3, 2, 2, 3 ),
 ( 0.2200000000000000011, 0.2233333333333333282, 0.2266666666666666552, 0.2300000000000000100 ),
 .UNSPECIFIED. ) 
 CURVE ( )  GEOMETRIC_REPRESENTATION_ITEM ( )  RATIONAL_B_SPLINE_CURVE ( ( 1.000000000000000000, 0.8660254037844387076, 1.000000000000000000, 0.8660254037844387076, 1.000000000000000000, 0.8660254037844387076, 1.000000000000000000 ) ) 
 REPRESENTATION_ITEM ( '' )  );
#12766 = CARTESIAN_POINT ( 'NONE',  ( 14.69062500061451537, -3.027376345333610441, -5.243569643749999898 ) ) ;
#12767 = CARTESIAN_POINT ( 'NONE',  ( 25.16250000122903074, 0.000000000000000000, 4.999999999999998224 ) ) ;
#12768 = CARTESIAN_POINT ( 'NONE',  ( 19.31250000000000000, -5.773502691896255534, -1.060575238724906372E-15 ) ) ;
#12769 = CARTESIAN_POINT ( 'NONE',  ( 22.62187500061451573, 3.027376345333611329, 5.243569643749999010 ) ) ;
#12770 = DIRECTION ( 'NONE',  ( 0.000000000000000000, 0.000000000000000000, 1.000000000000000000 ) ) ;
#12771 = CARTESIAN_POINT ( 'NONE',  ( 7.462500001229035007, 4.330127018922192761, -2.499999999999997780 ) ) ;
#12772 = CARTESIAN_POINT ( 'NONE',  ( 9.571875000614518569, 3.027376345333611329, 5.243569643749999010 ) ) ;
#12773 = CARTESIAN_POINT ( 'NONE',  ( 26.48437500061451644, 6.421520780324663323E-16, -5.243569643749999010 ) ) ;
#12774 = CARTESIAN_POINT ( 'NONE',  ( 15.41250000122903252, -4.330127018922190985, -2.500000000000001332 ) ) ;
#12775 = CARTESIAN_POINT ( 'NONE',  ( 20.27812500061451573, 4.541064518000418104, 2.621784821874999949 ) ) ;
#12776 = CARTESIAN_POINT ( 'NONE',  ( 27.12187500061451573, 3.027376345333611329, 5.243569643749999010 ) ) ;
#12777 = CARTESIAN_POINT ( 'NONE',  ( -1.878215178124999163, 16.95312499938548356, 26.74683588394047007 ) ) ;
#12778 = CARTESIAN_POINT ( 'NONE',  ( 9.046875000614518214, 6.054752690667223547, 3.707466751127219781E-16 ) ) ;
#12779 = CARTESIAN_POINT ( 'NONE',  ( 18.59062500061451573, -3.027376345333614438, 5.243569643749998122 ) ) ;
#12780 = ORIENTED_EDGE ( 'NONE', *, *, #26740, .F. ) ;
#12781 = CYLINDRICAL_SURFACE ( 'NONE', #18295, 4.000000000000000000 ) ;
#12782 = CARTESIAN_POINT ( 'NONE',  ( 27.10312500061451502, 0.000000000000000000, 5.243569643749999010 ) ) ;
#12783 = CARTESIAN_POINT ( 'NONE',  ( 3.196875000614516793, 6.054752690667223547, 3.707466751127219781E-16 ) ) ;
#12784 = DIRECTION ( 'NONE',  ( 1.000000000000000000, -0.000000000000000000, -0.000000000000000000 ) ) ;
#12785 = CYLINDRICAL_SURFACE ( 'NONE', #25312, 4.999999999999998224 ) ;
#12786 = CARTESIAN_POINT ( 'NONE',  ( 16.01249999999999929, 2.886751345948126879, 4.999999999999999112 ) ) ;
#12787 = CARTESIAN_POINT ( 'NONE',  ( 21.77812500061451928, -4.541064518000419881, 2.621784821874995952 ) ) ;
#12788 = EDGE_LOOP ( 'NONE', ( #14894, #48364 ) ) ;
#12789 = CARTESIAN_POINT ( 'NONE',  ( 24.93750000000000355, 5.773502691896255534, 3.535250795749688894E-16 ) ) ;
#12790 = CARTESIAN_POINT ( 'NONE',  ( 26.37187500061451217, -6.054752690667223547, -1.112240025338166033E-15 ) ) ;
#12791 = EDGE_CURVE ( 'NONE', #68292, #17100, #7429, .T. ) ;
#12792 = VERTEX_POINT ( 'NONE', #20941 ) ;
#12793 = CARTESIAN_POINT ( 'NONE',  ( 15.21562500061451750, 3.027376345333613106, -5.243569643749998122 ) ) ;
#12794 = CARTESIAN_POINT ( 'NONE',  ( 5.090625000614516615, -3.027376345333614438, 5.243569643749998122 ) ) ;
#12795 = CARTESIAN_POINT ( 'NONE',  ( 19.92187500061451289, -4.119189519843968306, 2.378215178124996054 ) ) ;
#12796 = CARTESIAN_POINT ( 'NONE',  ( 2.971875000614517592, -6.054752690667223547, -1.112240025338166033E-15 ) ) ;
#12797 = CARTESIAN_POINT ( 'NONE',  ( 14.17500000122903536, 2.886751345948129099, -4.999999999999998224 ) ) ;
#12798 = CARTESIAN_POINT ( 'NONE',  ( 20.73750000000000071, -2.886751345948125991, -5.000000000000000000 ) ) ;
#12799 = CARTESIAN_POINT ( 'NONE',  ( 28.61249999999999716, 2.886751345948126879, 4.999999999999999112 ) ) ;
#12800 = CARTESIAN_POINT ( 'NONE',  ( 3.721875000614518036, 3.027376345333611329, 5.243569643749999010 ) ) ;
#12801 = CARTESIAN_POINT ( 'NONE',  ( 10.43437500061451750, 4.541064518000418104, 2.621784821874999949 ) ) ;
#12802 = CARTESIAN_POINT ( 'NONE',  ( 19.35937500061451644, 4.541064518000418104, -2.621784821874998173 ) ) ;
#12803 = CARTESIAN_POINT ( 'NONE',  ( 11.41875000122903216, 2.886751345948129099, -4.999999999999997335 ) ) ;
#12804 = ORIENTED_EDGE ( 'NONE', *, *, #68955, .T. ) ;
#12805 = CARTESIAN_POINT ( 'NONE',  ( 28.71562500061451573, 3.027376345333613106, -5.243569643749998122 ) ) ;
#12806 = CARTESIAN_POINT ( 'NONE',  ( 3.149999999999999911, -4.330127018922190985, -2.500000000000001332 ) ) ;
#12807 =( BOUNDED_CURVE ( )  B_SPLINE_CURVE ( 2, ( #61417, #39262, #21521, #10810, #50704, #49979, #16343, #68060, #55883 ),
 .UNSPECIFIED., .F., .F. ) 
 B_SPLINE_CURVE_WITH_KNOTS ( ( 3, 2, 2, 2, 3 ),
 ( 0.4456521739130435145, 0.4492753623188405765, 0.4565217391304347561, 0.4637681159420289911, 0.4673913043478261087 ),
 .UNSPECIFIED. ) 
 CURVE ( )  GEOMETRIC_REPRESENTATION_ITEM ( )  RATIONAL_B_SPLINE_CURVE ( ( 0.9330127018922194093, 0.9330127018922198534, 1.000000000000000000, 0.8660254037844387076, 1.000000000000000000, 0.8660254037844387076, 1.000000000000000000, 0.9330127018922188542, 0.9330127018922194093 ) ) 
 REPRESENTATION_ITEM ( '' )  );
#12808 = CARTESIAN_POINT ( 'NONE',  ( 5.484375000614518214, 4.541064518000418104, 2.621784821874999949 ) ) ;
#12809 = CARTESIAN_POINT ( 'NONE',  ( 19.16250000000000142, 2.886751345948126879, 4.999999999999999112 ) ) ;
#12810 = CARTESIAN_POINT ( 'NONE',  ( 12.92812500061451786, 6.421520780324663323E-16, -5.243569643749999010 ) ) ;
#12811 = CARTESIAN_POINT ( 'NONE',  ( 5.163760131380204399, 20.58432050246338108, 33.15120568351349561 ) ) ;
#12812 = CARTESIAN_POINT ( 'NONE',  ( 4.080569135018654592, -2.889455923578380769, -4.080569135022440896 ) ) ;
#12813 = CARTESIAN_POINT ( 'NONE',  ( 11.15625000122903288, 0.000000000000000000, 4.999999999999998224 ) ) ;
#12814 = CARTESIAN_POINT ( 'NONE',  ( 19.92187500061451644, 2.746126346562643317, 4.756430356249998326 ) ) ;
#12815 = CARTESIAN_POINT ( 'NONE',  ( 8.465625000614515727, 3.027376345333613106, -5.243569643749998122 ) ) ;
#12816 = CARTESIAN_POINT ( 'NONE',  ( 25.17187500061451644, 3.027376345333613106, -5.243569643749998122 ) ) ;
#12817 = CARTESIAN_POINT ( 'NONE',  ( -4.243569643749997233, 18.54687500061451289, 32.45002607614398471 ) ) ;
#12818 = CARTESIAN_POINT ( 'NONE',  ( 25.99687500061451928, -3.027376345333610441, -5.243569643749999898 ) ) ;
#12819 = CARTESIAN_POINT ( 'NONE',  ( 6.862500000000002487, 2.886751345948129099, -4.999999999999998224 ) ) ;
#12820 = CARTESIAN_POINT ( 'NONE',  ( -2.000000000000000000, 13.73750000122903359, 26.53589838486224650 ) ) ;
#12821 = CARTESIAN_POINT ( 'NONE',  ( 14.12812500061451715, -4.541064518000419881, 2.621784821874995952 ) ) ;
#12822 = CARTESIAN_POINT ( 'NONE',  ( 6.525000001229033231, 2.886751345948129099, -4.999999999999998224 ) ) ;
#12823 = CARTESIAN_POINT ( 'NONE',  ( 16.99687500061451573, -3.027376345333610441, -5.243569643749999898 ) ) ;
#12824 = CARTESIAN_POINT ( 'NONE',  ( 12.83437500061451786, -4.541064518000419881, 2.621784821874995952 ) ) ;
#12825 = CARTESIAN_POINT ( 'NONE',  ( 45.00000000000000000, 0.000000000000000000, 4.999999999999998224 ) ) ;
#12826 = ORIENTED_EDGE ( 'NONE', *, *, #63077, .T. ) ;
#12827 = CARTESIAN_POINT ( 'NONE',  ( 11.91562500061451857, -6.054752690667223547, -1.112240025338166033E-15 ) ) ;
#12828 = CARTESIAN_POINT ( 'NONE',  ( 13.83749999999999858, -2.886751345948130876, 4.999999999999996447 ) ) ;
#12829 = CARTESIAN_POINT ( 'NONE',  ( 23.81250000122903288, 0.000000000000000000, 4.999999999999998224 ) ) ;
#12830 = CARTESIAN_POINT ( 'NONE',  ( 12.60937500061451821, 4.541064518000418104, -2.621784821874998173 ) ) ;
#12831 = CARTESIAN_POINT ( 'NONE',  ( 3.300000000000000711, 4.330127018922192761, -2.499999999999997780 ) ) ;
#12832 = CARTESIAN_POINT ( 'NONE',  ( 14.61562500061451608, -6.054752690667223547, -1.112240025338166033E-15 ) ) ;
#12833 = CARTESIAN_POINT ( 'NONE',  ( -5.810221930991193690E-16, 18.98750000000000071, -34.00000000000000000 ) ) ;
#12834 = CARTESIAN_POINT ( 'NONE',  ( 24.08437500061451786, -4.541064518000419881, 2.621784821874995952 ) ) ;
#12835 = CARTESIAN_POINT ( 'NONE',  ( 8.400000000000000355, 0.000000000000000000, 4.999999999999998224 ) ) ;
#12836 = CARTESIAN_POINT ( 'NONE',  ( 12.82500000122903394, 2.886751345948129099, -4.999999999999998224 ) ) ;
#12837 = CARTESIAN_POINT ( 'NONE',  ( 4.428044609675158227, 2.322158679919935409, 4.428044609675073850 ) ) ;
#12838 = CARTESIAN_POINT ( 'NONE',  ( 22.85625000122903216, 0.000000000000000000, 4.999999999999998224 ) ) ;
#12839 = CARTESIAN_POINT ( 'NONE',  ( 9.001249775931846008E-16, 17.72187500061451715, -25.09994784771203058 ) ) ;
#12840 = CARTESIAN_POINT ( 'NONE',  ( 18.90937500061451360, 4.541064518000418104, -2.621784821874998173 ) ) ;
#12841 = CARTESIAN_POINT ( 'NONE',  ( 17.58750000122903145, -4.330127018922194537, 2.499999999999995559 ) ) ;
#12842 =( BOUNDED_CURVE ( )  B_SPLINE_CURVE ( 2, ( #37620, #15811, #9913, #60142, #60880, #32815, #9186, #32451, #4747 ),
 .UNSPECIFIED., .F., .F. ) 
 B_SPLINE_CURVE_WITH_KNOTS ( ( 3, 2, 2, 2, 3 ),
 ( 0.5694444444444444198, 0.5740740740740740700, 0.5833333333333333703, 0.5925925925925925597, 0.5972222222222222099 ),
 .UNSPECIFIED. ) 
 CURVE ( )  GEOMETRIC_REPRESENTATION_ITEM ( )  RATIONAL_B_SPLINE_CURVE ( ( 0.9330127018922194093, 0.9330127018922194093, 1.000000000000000000, 0.8660254037844387076, 1.000000000000000000, 0.8660254037844387076, 1.000000000000000000, 0.9330127018922194093, 0.9330127018922194093 ) ) 
 REPRESENTATION_ITEM ( '' )  );
#12843 = CARTESIAN_POINT ( 'NONE',  ( 15.60937500061451644, -4.541064518000417216, -2.621784821875001281 ) ) ;
#12844 = CARTESIAN_POINT ( 'NONE',  ( 9.001249775931846008E-16, 10.97187500061451715, 34.90005215228797653 ) ) ;
#12845 = CARTESIAN_POINT ( 'NONE',  ( 19.95000000122903572, -2.886751345948125991, -5.000000000000000000 ) ) ;
#12846 = CARTESIAN_POINT ( 'NONE',  ( 14.01562500061451644, 3.027376345333611329, 5.243569643749999010 ) ) ;
#12847 = VERTEX_POINT ( 'NONE', #20202 ) ;
#12848 = EDGE_LOOP ( 'NONE', ( #65125, #11411, #25924, #67209 ) ) ;
#12849 = CARTESIAN_POINT ( 'NONE',  ( 17.77499999999999858, 4.330127018922191873, 2.499999999999999556 ) ) ;
#12850 = CARTESIAN_POINT ( 'NONE',  ( 27.37500000000000000, -4.330127018922194537, 2.499999999999995559 ) ) ;
#12851 = CARTESIAN_POINT ( 'NONE',  ( 4.010363759615468204, 2.986131697625305836, 4.103404943945538896 ) ) ;
#12852 = CARTESIAN_POINT ( 'NONE',  ( 14.43750000122903288, -4.330127018922194537, 2.499999999999995559 ) ) ;
#12853 = CARTESIAN_POINT ( 'NONE',  ( 26.22187500061451715, 3.027376345333611329, 5.243569643749999010 ) ) ;
#12854 = CARTESIAN_POINT ( 'NONE',  ( 19.26562500061451644, 3.027376345333613106, -5.243569643749998122 ) ) ;
#12855 = CARTESIAN_POINT ( 'NONE',  ( 22.79062500061451502, -3.027376345333610441, -5.243569643749999898 ) ) ;
#12856 = CARTESIAN_POINT ( 'NONE',  ( 3.290625000614516793, -3.027376345333614438, 5.243569643749998122 ) ) ;
#12857 = CARTESIAN_POINT ( 'NONE',  ( 28.49999999999999645, 4.330127018922192761, -2.499999999999997780 ) ) ;
#12858 = FACE_OUTER_BOUND ( 'NONE', #50572, .T. ) ;
#12859 =( BOUNDED_CURVE ( )  B_SPLINE_CURVE ( 2, ( #51112, #49663, #44495, #67028, #50750, #67389, #22301, #33389, #17474 ),
 .UNSPECIFIED., .F., .F. ) 
 B_SPLINE_CURVE_WITH_KNOTS ( ( 3, 2, 2, 2, 3 ),
 ( 0.04166666666666667129, 0.04629629629629629373, 0.05555555555555555247, 0.06481481481481481122, 0.06944444444444444753 ),
 .UNSPECIFIED. ) 
 CURVE ( )  GEOMETRIC_REPRESENTATION_ITEM ( )  RATIONAL_B_SPLINE_CURVE ( ( 0.9330127018922192983, 0.9330127018922194093, 1.000000000000000000, 0.8660254037844387076, 1.000000000000000000, 0.8660254037844387076, 1.000000000000000000, 0.9330127018922191873, 0.9330127018922192983 ) ) 
 REPRESENTATION_ITEM ( '' )  );
#12860 = CARTESIAN_POINT ( 'NONE',  ( 7.996875000614519280, -2.746126346562642428, -4.756430356249999214 ) ) ;
#12861 = CARTESIAN_POINT ( 'NONE',  ( -0.6945863667395647534, 9.663023495605401081, -33.93923213064925193 ) ) ;
#12862 = DIRECTION ( 'NONE',  ( -1.000000000000000000, -0.000000000000000000, -0.000000000000000000 ) ) ;
#12863 = CARTESIAN_POINT ( 'NONE',  ( 2.121784821874999061, 16.10937500061451644, -33.67503911421598417 ) ) ;
#12864 = CARTESIAN_POINT ( 'NONE',  ( 7.050000001229036251, 5.773502691896255534, 3.535250795749688894E-16 ) ) ;
#12865 = CARTESIAN_POINT ( 'NONE',  ( 6.825000000000001066, 6.123233995736764310E-16, -4.999999999999998224 ) ) ;
#12866 = CARTESIAN_POINT ( 'NONE',  ( 11.77500000000000036, 6.123233995736764310E-16, -4.999999999999998224 ) ) ;
#12867 = CARTESIAN_POINT ( 'NONE',  ( 8.671875000614518214, 3.027376345333611329, 5.243569643749999010 ) ) ;
#12868 = CARTESIAN_POINT ( 'NONE',  ( 27.96562500061451928, 3.027376345333611329, 5.243569643749999010 ) ) ;
#12869 = CARTESIAN_POINT ( 'NONE',  ( 27.45000000122903216, -2.886751345948155301, 4.999999999999952927 ) ) ;
#12870 = CARTESIAN_POINT ( 'NONE',  ( -5.840105773466370387, 8.117609419225257028, -28.60964832515872658 ) ) ;
#12871 = EDGE_CURVE ( 'NONE', #49855, #12248, #55306, .T. ) ;
#12872 = CARTESIAN_POINT ( 'NONE',  ( 8.934375000614517504, 6.421520780324663323E-16, -5.243569643749999010 ) ) ;
#12873 = CARTESIAN_POINT ( 'NONE',  ( 12.34687500061452070, -3.027376345333614438, 5.243569643749998122 ) ) ;
#12874 = CARTESIAN_POINT ( 'NONE',  ( 7.050000000000000711, 0.000000000000000000, 4.999999999999998224 ) ) ;
#12875 = CARTESIAN_POINT ( 'NONE',  ( -4.243569643749999898, 14.85312500061459495, 30.00000000000000000 ) ) ;
#12876 = CARTESIAN_POINT ( 'NONE',  ( 0.5264921881209824184, 25.53585038844605037, 26.02618720140712227 ) ) ;
#12877 = CARTESIAN_POINT ( 'NONE',  ( 7.012500000000001066, 2.886751345948126879, 4.999999999999999112 ) ) ;
#12878 = CARTESIAN_POINT ( 'NONE',  ( 26.43750000122903288, 4.330127018922191873, 2.499999999999999556 ) ) ;
#12879 = CARTESIAN_POINT ( 'NONE',  ( 18.34687500061451360, 4.119189519843966529, -2.378215178124998275 ) ) ;
#12880 = CARTESIAN_POINT ( 'NONE',  ( 22.37812500061451360, 6.421520780324663323E-16, -5.243569643749999010 ) ) ;
#12881 = CARTESIAN_POINT ( 'NONE',  ( 14.31562500061451537, 3.027376345333613106, -5.243569643749998122 ) ) ;
#12882 = CARTESIAN_POINT ( 'NONE',  ( 25.50937500061451502, 2.746126346562645981, -4.756430356249997438 ) ) ;
#12883 = CARTESIAN_POINT ( 'NONE',  ( 9.459375000614517859, 4.541064518000418104, -2.621784821874998173 ) ) ;
#12884 = CARTESIAN_POINT ( 'NONE',  ( 27.18750000000000000, 5.773502691896255534, 3.535250795749688894E-16 ) ) ;
#12885 = CARTESIAN_POINT ( 'NONE',  ( 22.46250000122903501, 0.000000000000000000, 4.999999999999998224 ) ) ;
#12886 = CARTESIAN_POINT ( 'NONE',  ( -1.071796769724488563, 18.40490381179670365, -26.00000000000000000 ) ) ;
#12887 = CARTESIAN_POINT ( 'NONE',  ( 11.67187500061451821, 3.027376345333613106, -5.243569643749998122 ) ) ;
#12888 = CARTESIAN_POINT ( 'NONE',  ( 27.64687500061452141, -3.027376345333614438, 5.243569643749998122 ) ) ;
#12889 = CARTESIAN_POINT ( 'NONE',  ( 21.84375000122903288, 5.773502691896255534, 3.535250795749688401E-16 ) ) ;
#12890 = FACE_OUTER_BOUND ( 'NONE', #72920, .T. ) ;
#12891 = CARTESIAN_POINT ( 'NONE',  ( 22.54687500061451999, 6.054752690667223547, 3.707466751127219781E-16 ) ) ;
#12892 = CARTESIAN_POINT ( 'NONE',  ( 12.83437500061451786, -4.541064518000419881, 2.621784821874995952 ) ) ;
#12893 = CARTESIAN_POINT ( 'NONE',  ( -3.756430356250001434, 19.31562499938548427, 32.16877607737301048 ) ) ;
#12894 = CARTESIAN_POINT ( 'NONE',  ( 26.17500000000000071, 6.123233995736764310E-16, -4.999999999999998224 ) ) ;
#12895 = CARTESIAN_POINT ( 'NONE',  ( 2.828200636599751609E-16, 12.61249999999999893, 25.38119784648299415 ) ) ;
#12896 = CARTESIAN_POINT ( 'NONE',  ( 2.121784821875001281, 11.90937500061451892, -26.32496088578401938 ) ) ;
#12897 = CARTESIAN_POINT ( 'NONE',  ( 27.45937500061451786, 4.119189519843966529, -2.378215178124998275 ) ) ;
#12898 = CARTESIAN_POINT ( 'NONE',  ( 17.57812500061451644, 4.541064518000418104, 2.621784821874999949 ) ) ;
#12899 = CARTESIAN_POINT ( 'NONE',  ( 6.450000000000001066, 4.330127018922192761, -2.499999999999997780 ) ) ;
#12900 = CARTESIAN_POINT ( 'NONE',  ( 0.000000000000000000, 20.00000000000000000, -33.99999999999999289 ) ) ;
#12901 = CARTESIAN_POINT ( 'NONE',  ( 14.32500000000000107, -4.330127018922194537, 2.499999999999995559 ) ) ;
#12902 = CARTESIAN_POINT ( 'NONE',  ( -3.000416591977282496E-16, 10.69062500061451715, 25.09994784771203058 ) ) ;
#12903 = CARTESIAN_POINT ( 'NONE',  ( 13.53750000122903430, -4.330127018922194537, 2.499999999999995559 ) ) ;
#12904 = CARTESIAN_POINT ( 'NONE',  ( 24.98437500061451644, -4.541064518000419881, 2.621784821874995952 ) ) ;
#12905 = EDGE_LOOP ( 'NONE', ( #10276, #4789, #19737 ) ) ;
#12906 = CARTESIAN_POINT ( 'NONE',  ( 19.86562500061451786, 3.027376345333611329, 5.243569643749999010 ) ) ;
#12907 = CARTESIAN_POINT ( 'NONE',  ( 19.84687500061451360, 6.054752690667223547, 3.707466751127219781E-16 ) ) ;
#12908 = CARTESIAN_POINT ( 'NONE',  ( 4.800000000000002487, 0.000000000000000000, 4.999999999999998224 ) ) ;
#12909 = CARTESIAN_POINT ( 'NONE',  ( 7.940625000614518036, -3.027376345333610441, -5.243569643749999898 ) ) ;
#12910 = CARTESIAN_POINT ( 'NONE',  ( 20.76562500061451644, 3.027376345333611329, 5.243569643749999010 ) ) ;
#12911 = CARTESIAN_POINT ( 'NONE',  ( 12.08437500061451608, 6.421520780324663323E-16, -5.243569643749999010 ) ) ;
#12912 = CARTESIAN_POINT ( 'NONE',  ( 17.70937500061451431, 0.000000000000000000, 5.243569643749999010 ) ) ;
#12913 = CARTESIAN_POINT ( 'NONE',  ( 4.243569643749999898, 15.52812500061451750, 30.00000000000000000 ) ) ;
#12914 = CARTESIAN_POINT ( 'NONE',  ( 19.35000000122903430, -2.886751345948129988, 4.999999999999997335 ) ) ;
#12915 = CARTESIAN_POINT ( 'NONE',  ( 11.74687500061451573, 5.492252693125287522, 3.363034840372157021E-16 ) ) ;
#12916 = CARTESIAN_POINT ( 'NONE',  ( 8.503125000614515372, 4.541064518000418104, -2.621784821874998173 ) ) ;
#12917 = CARTESIAN_POINT ( 'NONE',  ( 3.271875000614519635, 3.027376345333611329, 5.243569643749999010 ) ) ;
#12918 = CARTESIAN_POINT ( 'NONE',  ( 28.52812500061451573, -4.541064518000419881, 2.621784821874995952 ) ) ;
#12919 = CARTESIAN_POINT ( 'NONE',  ( 26.10937500061451644, 4.541064518000418104, -2.621784821874998173 ) ) ;
#12920 = CARTESIAN_POINT ( 'NONE',  ( 16.52812500061451573, 6.421520780324663323E-16, -5.243569643749999010 ) ) ;
#12921 = CARTESIAN_POINT ( 'NONE',  ( 25.95000000122903216, 5.773502691896255534, 3.535250795749688894E-16 ) ) ;
#12922 = CARTESIAN_POINT ( 'NONE',  ( 26.05312500061451431, 4.541064518000418104, -2.621784821874998173 ) ) ;
#12923 = CARTESIAN_POINT ( 'NONE',  ( 22.99687500061451573, 6.054752690667223547, 3.707466751127219781E-16 ) ) ;
#12924 = CARTESIAN_POINT ( 'NONE',  ( 14.24062500061451608, -3.027376345333610441, -5.243569643749999898 ) ) ;
#12925 = CARTESIAN_POINT ( 'NONE',  ( -2.121784821874996840, 16.78437500061452070, 33.67503911421598417 ) ) ;
#12926 = CARTESIAN_POINT ( 'NONE',  ( 22.26562500061451644, -6.054752690667223547, -1.112240025338166033E-15 ) ) ;
#12927 = CARTESIAN_POINT ( 'NONE',  ( 23.53125000122902932, 6.123233995736764310E-16, -4.999999999999998224 ) ) ;
#12928 = ORIENTED_EDGE ( 'NONE', *, *, #64752, .F. ) ;
#12929 = CARTESIAN_POINT ( 'NONE',  ( 25.53750000000000142, -2.886751345948129988, 4.999999999999997335 ) ) ;
#12930 = CARTESIAN_POINT ( 'NONE',  ( 3.999999999999998668, 12.16250000000000142, -32.30940107675850470 ) ) ;
#12931 = CARTESIAN_POINT ( 'NONE',  ( 3.999999999999998668, 18.12500000122903288, 27.69059892324149530 ) ) ;
#12932 = CARTESIAN_POINT ( 'NONE',  ( 29.05312500061451431, -4.541064518000417216, -2.621784821875001281 ) ) ;
#12933 = CARTESIAN_POINT ( 'NONE',  ( 9.628125000614517148, -4.541064518000419881, 2.621784821874995952 ) ) ;
#12934 = CARTESIAN_POINT ( 'NONE',  ( 21.90000000122903145, 5.773502691896255534, 3.535250795749688894E-16 ) ) ;
#12935 = CARTESIAN_POINT ( 'NONE',  ( 26.35312500061451857, -4.541064518000417216, -2.621784821875001281 ) ) ;
#12936 = CARTESIAN_POINT ( 'NONE',  ( 25.23749999999999716, -2.886751345948125991, -5.000000000000000000 ) ) ;
#12937 = CARTESIAN_POINT ( 'NONE',  ( -3.999999999999997335, 15.20000000122903572, -27.69059892324149175 ) ) ;
#12938 = CARTESIAN_POINT ( 'NONE',  ( 29.12812500061451715, 6.421520780324663323E-16, -5.243569643749999010 ) ) ;
#12939 = CARTESIAN_POINT ( 'NONE',  ( 10.49062500061451431, -3.027376345333614438, 5.243569643749998122 ) ) ;
#12940 = ORIENTED_EDGE ( 'NONE', *, *, #15134, .F. ) ;
#12941 = EDGE_CURVE ( 'NONE', #58137, #15201, #49400, .T. ) ;
#12942 = CARTESIAN_POINT ( 'NONE',  ( 25.94062500061451715, -3.027376345333610441, -5.243569643749999898 ) ) ;
#12943 = CARTESIAN_POINT ( 'NONE',  ( 8.278125000614515727, -4.541064518000419881, 2.621784821874995952 ) ) ;
#12944 = CARTESIAN_POINT ( 'NONE',  ( 4.528125000614516615, 4.541064518000418104, 2.621784821874999949 ) ) ;
#12945 = CARTESIAN_POINT ( 'NONE',  ( 15.19687500061451857, -2.746126346562642428, -4.756430356249999214 ) ) ;
#12946 = LINE ( 'NONE', #46215, #46775 ) ;
#12947 = CARTESIAN_POINT ( 'NONE',  ( 13.98750000000000249, -2.886751345948125991, -5.000000000000000000 ) ) ;
#12948 = EDGE_CURVE ( 'NONE', #10190, #55745, #4443, .T. ) ;
#12949 = CARTESIAN_POINT ( 'NONE',  ( 13.77187500061451786, -6.054752690667223547, -1.112240025338166033E-15 ) ) ;
#12950 = CARTESIAN_POINT ( 'NONE',  ( 10.61250000122903536, 4.330127018922192761, -2.499999999999997780 ) ) ;
#12951 = CARTESIAN_POINT ( 'NONE',  ( 17.37187500061451573, -6.054752690667223547, -1.112240025338166033E-15 ) ) ;
#12952 = CARTESIAN_POINT ( 'NONE',  ( 16.83749999999999858, 5.773502691896255534, 3.535250795749688894E-16 ) ) ;
#12953 = CARTESIAN_POINT ( 'NONE',  ( 8.484375000614518214, 6.421520780324663323E-16, -5.243569643749999010 ) ) ;
#12954 = CARTESIAN_POINT ( 'NONE',  ( 4.243569643749999010, 10.61562500061451786, -32.45002607614398471 ) ) ;
#12955 = CARTESIAN_POINT ( 'NONE',  ( 27.86250000122903359, 0.000000000000000000, 4.999999999999998224 ) ) ;
#12956 = CARTESIAN_POINT ( 'NONE',  ( 23.03437500061451360, -2.746126346562646425, 4.756430356249996549 ) ) ;
#12957 = CARTESIAN_POINT ( 'NONE',  ( 30.00000000000000000, 0.000000000000000000, 9.999999999999998224 ) ) ;
#12958 = CARTESIAN_POINT ( 'NONE',  ( 23.72812500061451502, 6.421520780324663323E-16, -5.243569643749999010 ) ) ;
#12959 = CARTESIAN_POINT ( 'NONE',  ( 11.21250000000000036, -5.773502691896255534, -1.060575238724906372E-15 ) ) ;
#12960 = CARTESIAN_POINT ( 'NONE',  ( 28.77187500061451431, 3.027376345333613106, -5.243569643749998122 ) ) ;
#12961 = CARTESIAN_POINT ( 'NONE',  ( 24.60000000000000142, 0.000000000000000000, 4.999999999999998224 ) ) ;
#12962 = CARTESIAN_POINT ( 'NONE',  ( 6.890625000614516438, -3.027376345333614438, 5.243569643749998122 ) ) ;
#12963 = CARTESIAN_POINT ( 'NONE',  ( 25.17187500061451644, 4.119189519843966529, 2.378215178124999607 ) ) ;
#12964 = CARTESIAN_POINT ( 'NONE',  ( 16.88437500061451502, -4.541064518000419881, 2.621784821874995952 ) ) ;
#12965 = CARTESIAN_POINT ( 'NONE',  ( 10.80937500061451573, 2.746126346562643317, 4.756430356249998326 ) ) ;
#12966 = CARTESIAN_POINT ( 'NONE',  ( 29.40000000122903145, -2.886751345948125991, -5.000000000000000000 ) ) ;
#12967 = CARTESIAN_POINT ( 'NONE',  ( 8.746875000614515727, -3.027376345333614438, 5.243569643749998122 ) ) ;
#12968 = ORIENTED_EDGE ( 'NONE', *, *, #28075, .F. ) ;
#12969 = CARTESIAN_POINT ( 'NONE',  ( 17.93437500061451928, 6.421520780324663323E-16, -5.243569643749999010 ) ) ;
#12970 = CYLINDRICAL_SURFACE ( 'NONE', #22942, 4.999999999999998224 ) ;
#12971 = CARTESIAN_POINT ( 'NONE',  ( 26.66250000000000142, 2.886751345948129099, -4.999999999999998224 ) ) ;
#12973 = EDGE_CURVE ( 'NONE', #28631, #32715, #47787, .T. ) ;
#12972 = CARTESIAN_POINT ( 'NONE',  ( 3.825000000000001954, 4.330127018922191873, 2.499999999999999556 ) ) ;
#12974 = DIRECTION ( 'NONE',  ( -1.000000000000000000, -0.000000000000000000, -0.000000000000000000 ) ) ;
#12975 = CARTESIAN_POINT ( 'NONE',  ( 17.62500000000000000, 6.123233995736764310E-16, -4.999999999999998224 ) ) ;
#12976 = VERTEX_POINT ( 'NONE', #32034 ) ;
#12977 = CARTESIAN_POINT ( 'NONE',  ( 11.28749999999999787, -2.886751345948125991, -5.000000000000000000 ) ) ;
#12978 = CARTESIAN_POINT ( 'NONE',  ( 10.84687500061451715, 0.000000000000000000, 4.756430356249998326 ) ) ;
#12979 = CARTESIAN_POINT ( 'NONE',  ( 25.22812500061451502, 4.541064518000418104, 2.621784821874999949 ) ) ;
#12980 = CARTESIAN_POINT ( 'NONE',  ( 15.15000000000000036, 0.000000000000000000, 4.999999999999998224 ) ) ;
#12981 =( BOUNDED_CURVE ( )  B_SPLINE_CURVE ( 2, ( #30503, #6887, #40150, #62669, #68947, #24585, #47133 ),
 .UNSPECIFIED., .F., .F. ) 
 B_SPLINE_CURVE_WITH_KNOTS ( ( 3, 2, 2, 3 ),
 ( 0.9799999999999999822, 0.9833333333333333925, 0.9866666666666668029, 0.9900000000000002132 ),
 .UNSPECIFIED. ) 
 CURVE ( )  GEOMETRIC_REPRESENTATION_ITEM ( )  RATIONAL_B_SPLINE_CURVE ( ( 1.000000000000000000, 0.8660254037844387076, 1.000000000000000000, 0.8660254037844387076, 1.000000000000000000, 0.8660254037844298258, 1.000000000000008882 ) ) 
 REPRESENTATION_ITEM ( '' )  );
#12982 = CARTESIAN_POINT ( 'NONE',  ( 8.850000001229034297, 5.773502691896255534, 3.535250795749688894E-16 ) ) ;
#12983 = CARTESIAN_POINT ( 'NONE',  ( 7.228125000614517681, 4.541064518000418104, 2.621784821874999949 ) ) ;
#12984 = CARTESIAN_POINT ( 'NONE',  ( 20.81250000000000000, 2.886751345948129099, -4.999999999999998224 ) ) ;
#12985 = CARTESIAN_POINT ( 'NONE',  ( 21.14062500061451289, 6.054752690667223547, 3.707466751127219781E-16 ) ) ;
#12986 = CARTESIAN_POINT ( 'NONE',  ( 4.800000001229032698, 5.773502691896255534, 3.535250795749688401E-16 ) ) ;
#12987 = CARTESIAN_POINT ( 'NONE',  ( 25.31250000122903288, -4.330127018922190985, -2.500000000000001332 ) ) ;
#12988 = CARTESIAN_POINT ( 'NONE',  ( -3.756430356250000102, 17.81562499938548427, 30.00000000000000000 ) ) ;
#12989 = CARTESIAN_POINT ( 'NONE',  ( 4.050000000000001599, -4.330127018922190985, -2.500000000000001332 ) ) ;
#12990 = ORIENTED_EDGE ( 'NONE', *, *, #72086, .T. ) ;
#12991 = CARTESIAN_POINT ( 'NONE',  ( 21.85312500061451502, -4.541064518000417216, -2.621784821875001281 ) ) ;
#12992 = CARTESIAN_POINT ( 'NONE',  ( 26.95312500061451644, 4.541064518000418104, -2.621784821874998173 ) ) ;
#12993 = CARTESIAN_POINT ( 'NONE',  ( 27.34687500061451360, -3.027376345333610441, -5.243569643749999898 ) ) ;
#12994 = CARTESIAN_POINT ( 'NONE',  ( 15.17812500061451608, 6.421520780324663323E-16, -5.243569643749999010 ) ) ;
#12995 = CARTESIAN_POINT ( 'NONE',  ( -2.121784821874996840, 9.978125000614594953, -26.32496088578401583 ) ) ;
#12996 = CARTESIAN_POINT ( 'NONE',  ( 25.12500000122903288, 2.886751345948126879, 4.999999999999999112 ) ) ;
#12997 = CARTESIAN_POINT ( 'NONE',  ( 22.58437500061451431, 4.119189519843966529, 2.378215178124999607 ) ) ;
#12998 = CARTESIAN_POINT ( 'NONE',  ( 17.84062500061451573, -3.027376345333610441, -5.243569643749999898 ) ) ;
#12999 = CARTESIAN_POINT ( 'NONE',  ( -5.810221930991193690E-16, 14.60000000122903252, -34.00000000000000000 ) ) ;
#13000 = CARTESIAN_POINT ( 'NONE',  ( 3.037500001229032964, 4.330127018922191873, 2.499999999999999556 ) ) ;
#13001 = CARTESIAN_POINT ( 'NONE',  ( 11.44687500061451857, -3.027376345333614438, 5.243569643749998122 ) ) ;
#13002 = CARTESIAN_POINT ( 'NONE',  ( 8.559375000614515727, 4.541064518000418104, -2.621784821874998173 ) ) ;
#13003 = CARTESIAN_POINT ( 'NONE',  ( 19.77187500061451786, 3.027376345333613106, -5.243569643749998122 ) ) ;
#13004 = ORIENTED_EDGE ( 'NONE', *, *, #31222, .F. ) ;
#13005 = CARTESIAN_POINT ( 'NONE',  ( 23.54062500061451146, -3.027376345333614438, 5.243569643749998122 ) ) ;
#13006 = CARTESIAN_POINT ( 'NONE',  ( 19.84687500061451360, 6.054752690667223547, 3.707466751127219781E-16 ) ) ;
#13007 = CARTESIAN_POINT ( 'NONE',  ( 23.54062500061451146, -3.027376345333614438, 5.243569643749998122 ) ) ;
#13008 = CARTESIAN_POINT ( 'NONE',  ( -1.071796769724488563, 9.854903811796701163, 34.00000000000000000 ) ) ;
#13009 = CARTESIAN_POINT ( 'NONE',  ( 1.999999999999998668, 14.90000000000000036, 26.53589838486224650 ) ) ;
#13010 = CARTESIAN_POINT ( 'NONE',  ( 3.384375000614517237, -4.541064518000419881, 2.621784821874995952 ) ) ;
#13011 = CARTESIAN_POINT ( 'NONE',  ( 8.962500001229033231, 0.000000000000000000, 4.999999999999998224 ) ) ;
#13012 = CARTESIAN_POINT ( 'NONE',  ( 4.462500001229035007, 0.000000000000000000, 4.999999999999998224 ) ) ;
#13013 = CARTESIAN_POINT ( 'NONE',  ( -5.810221930991193690E-16, 13.70000000122903394, -34.00000000000000000 ) ) ;
#13014 = CARTESIAN_POINT ( 'NONE',  ( 26.47500000122903074, 2.886751345948126879, 4.999999999999999112 ) ) ;
#13015 = CARTESIAN_POINT ( 'NONE',  ( 2.000000000000000444, 20.16874999877096641, 26.53589838486224650 ) ) ;
#13016 = CARTESIAN_POINT ( 'NONE',  ( 10.02187500061451964, 3.027376345333611329, 5.243569643749999010 ) ) ;
#13017 = CARTESIAN_POINT ( 'NONE',  ( 9.412499999999999645, -5.773502691896255534, -1.060575238724906372E-15 ) ) ;
#13018 = CARTESIAN_POINT ( 'NONE',  ( 17.65312500061451573, 0.000000000000000000, 5.243569643749999010 ) ) ;
#13019 = CARTESIAN_POINT ( 'NONE',  ( 10.69687500061451679, -3.027376345333610441, -5.243569643749999898 ) ) ;
#13020 = CARTESIAN_POINT ( 'NONE',  ( 29.47500000122903430, 2.886751345948129099, -4.999999999999998224 ) ) ;
#13021 = CARTESIAN_POINT ( 'NONE',  ( 20.52187500061451786, -6.054752690667223547, -1.112240025338166033E-15 ) ) ;
#13022 = CARTESIAN_POINT ( 'NONE',  ( 7.696875000614516793, 6.054752690667223547, 3.707466751127219781E-16 ) ) ;
#13023 = CARTESIAN_POINT ( 'NONE',  ( 3.815625000614518036, -6.054752690667223547, -1.112240025338166033E-15 ) ) ;
#13024 = CARTESIAN_POINT ( 'NONE',  ( 30.00000000000000000, 0.000000000000000000, 4.999999999999998224 ) ) ;
#13025 = CARTESIAN_POINT ( 'NONE',  ( 8.840625000614515727, -3.027376345333610441, -5.243569643749999898 ) ) ;
#13026 = CARTESIAN_POINT ( 'NONE',  ( 18.21562500061451573, -6.054752690667223547, -1.112240025338166033E-15 ) ) ;
#13027 = ORIENTED_EDGE ( 'NONE', *, *, #63628, .F. ) ;
#13028 = CARTESIAN_POINT ( 'NONE',  ( 6.450000001229034829, -2.886751345948125991, -5.000000000000000000 ) ) ;
#13029 = CARTESIAN_POINT ( 'NONE',  ( 13.75312500061451715, -4.541064518000417216, -2.621784821875001281 ) ) ;
#13030 = CARTESIAN_POINT ( 'NONE',  ( 12.85312500061451502, -4.541064518000417216, -2.621784821875001281 ) ) ;
#13031 = CARTESIAN_POINT ( 'NONE',  ( 22.69687500061451857, -2.746126346562646425, 4.756430356249996549 ) ) ;
#13032 = CARTESIAN_POINT ( 'NONE',  ( 14.36249999999999893, -5.773502691896255534, -1.060575238724906372E-15 ) ) ;
#13033 = CARTESIAN_POINT ( 'NONE',  ( 7.237500001229035362, -4.330127018922194537, 2.499999999999995559 ) ) ;
#13034 = EDGE_CURVE ( 'NONE', #69794, #14534, #40046, .T. ) ;
#13035 =( BOUNDED_CURVE ( )  B_SPLINE_CURVE ( 2, ( #66872, #32877, #4085, #54683, #48783, #26615, #43243, #16241, #3719, #60572, #71308, #70946, #38421, #60943, #25880, #10347, #9979, #55416, #4811, #27343, #61312, #26983, #10708, #59849, #53961, #9618, #20317, #15506, #65393, #14784, #37326, #32516, #49512, #31789, #65764, #49152, #21055, #72768, #55778, #56848, #16599, #44706, #5535, #22153, #67241, #5170, #39153, #61670, #28072, #27705, #33596, #56141, #5891, #51322, #34681, #46143, #11069, #34315, #50600, #17680, #51686, #23598, #6254, #28782, #12154, #29154, #68682, #726, #5, #22512, #23234, #62762, #62400, #45059, #67596, #11798, #16962, #39516, #50959, #62043, #22864, #45785, #11438, #68320, #50246, #33957, #56496, #28422, #357, #45420, #57211, #67956, #17328, #63122, #40239, #39887, #6625, #40600, #1090, #18043, #33241, #57577, #52046, #6980, #35770, #42420, #13232, #18765, #52406, #52769, #1815, #59023, #18406, #46871, #24322, #8068, #29511, #2526, #13595, #40972, #63487, #47229, #25047, #69410, #58293, #41331, #30960, #53496, #64576, #23955, #63840, #69043, #12875, #35407, #64206, #7699, #24682, #2171, #30236, #70119, #69761, #13965, #25419, #1450, #36140, #46505, #19496, #2889, #19867, #57933, #19129, #35049, #58660, #53127, #41683, #30600, #7340, #29869, #47590, #47962, #42054, #36503, #8424, #70490, #12518, #9529, #48692, #54595, #14331, #49790, #54232, #53871, #66410, #71215, #21696, #4367, #32062, #20592, #10260, #43884, #15061, #43518, #65672, #43149, #72315, #59384, #27257, #48329, #3998, #60857, #20227, #66041, #70854, #31697, #9890, #21331, #54962, #15787, #37598, #38328, #4723, #3629, #60484, #8795, #26897, #15419, #42780, #65300, #32792, #26524, #49422, #26151, #60119, #49062, #55329, #64941, #71590, #36866, #31329, #32426, #3263, #20964, #14690, #25791, #71955, #37233, #59755, #9162, #37962, #45701, #51235, #34229, #56763, #12072, #61228, #27986, #45334, #50874, #17241, #38708, #33872, #62677, #68234, #5806, #272, #67869, #22782, #39801, #40157, #10622, #66784, #62317, #6533, #72684, #11712, #17598, #67511, #50516, #6167, #16875, #34594, #16157, #29066, #33505, #33152, #57122, #73044, #1002, #28696 ),
 .UNSPECIFIED., .F., .F. ) 
 B_SPLINE_CURVE_WITH_KNOTS ( ( 3, 2, 2, 2, 2, 2, 2, 2, 2, 2, 2, 2, 2, 2, 2, 2, 2, 2, 2, 2, 2, 2, 2, 2, 2, 2, 2, 2, 2, 2, 2, 2, 2, 2, 2, 2, 2, 2, 2, 2, 2, 2, 2, 2, 2, 2, 2, 2, 2, 2, 2, 2, 2, 2, 2, 2, 2, 2, 2, 2, 2, 2, 2, 2, 2, 2, 2, 2, 2, 2, 2, 2, 2, 2, 2, 2, 2, 2, 2, 2, 2, 2, 2, 2, 2, 2, 2, 2, 2, 2, 2, 2, 2, 2, 2, 2, 2, 2, 2, 2, 2, 2, 2, 2, 2, 2, 2, 2, 2, 2, 2, 2, 2, 2, 2, 2, 2, 2, 2, 2, 2, 2, 2, 2, 2, 2, 2, 2, 2, 2, 2, 2, 2, 2, 3 ),
 ( 0.000000000000000000, 0.007499808158871946150, 0.01499961631774389230, 0.02249942447661583758, 0.02999923263548778460, 0.03749904079435972815, 0.04499884895323167516, 0.05249865711210362218, 0.05999846527097556920, 0.06749827342984751621, 0.07499808158871945629, 0.08249788974759139637, 0.08999769790646335033, 0.09749750606533530428, 0.1049973142242072444, 0.1124971223830791844, 0.1199969305419511384, 0.1274967387008230923, 0.1349965468596950324, 0.1424963550185669725, 0.1499961631774389126, 0.1574959713363108804, 0.1649957794951827927, 0.1724955876540547328, 0.1799953958129267007, 0.1874952039717986407, 0.1949950121306706086, 0.2024948202895425486, 0.2099946284484144887, 0.2174944366072864288, 0.2249942447661583689, 0.2324940529250303090, 0.2399938610839022768, 0.2474936692427742169, 0.2549934774016461847, 0.2624932855605180970, 0.2699930937193900649, 0.2774929018782620327, 0.2849927100371339450, 0.2924925181960058573, 0.2999923263548778252, 0.3074921345137497930, 0.3149919426726217608, 0.3224917508314936732, 0.3299915589903655855, 0.3374913671492375533, 0.3449911753081094656, 0.3524909834669814890, 0.3599907916258534013, 0.3674905997847253691, 0.3749904079435972815, 0.3824902161024691938, 0.3899900242613412171, 0.3974898324202131294, 0.4049896405790850973, 0.4124894487379570096, 0.4199892568968289774, 0.4274890650557008898, 0.4349888732145728576, 0.4424886813734448254, 0.4499884895323167378, 0.4574882976911887056, 0.4649881058500606179, 0.4724879140089325857, 0.4799877221678045536, 0.4874875303266764659, 0.4949873384855484337, 0.5024871466444204016, 0.5099869548032923694, 0.5174867629621642262, 0.5249865711210361940, 0.5324863792799081619, 0.5399861874387801297, 0.5474859955976520975, 0.5549858037565240654, 0.5624856119153959222, 0.5699854200742678900, 0.5774852282331398579, 0.5849850363920117147, 0.5924848445508836825, 0.5999846527097556503, 0.6074844608686276182, 0.6149842690274995860, 0.6224840771863715538, 0.6299838853452435217, 0.6374836935041153785, 0.6449835016629873463, 0.6524833098218593141, 0.6599831179807311710, 0.6674829261396031388, 0.6749827342984751066, 0.6824825424573470745, 0.6899823506162189313, 0.6974821587750910101, 0.7049819669339629780, 0.7124817750928348348, 0.7199815832517068026, 0.7274813914105787704, 0.7349811995694507383, 0.7424810077283225951, 0.7499808158871945629, 0.7574806240460665308, 0.7649804322049383876, 0.7724802403638103554, 0.7799800485226824343, 0.7874798566815544021, 0.7949796648404262589, 0.8024794729992982267, 0.8099792811581701946, 0.8174790893170420514, 0.8249788974759140192, 0.8324787056347859870, 0.8399785137936579549, 0.8474783219525298117, 0.8549781301114017795, 0.8624779382702738584, 0.8699777464291457152, 0.8774775545880176830, 0.8849773627468896509, 0.8924771709057616187, 0.8999769790646334755, 0.9074767872235054433, 0.9149765953823774112, 0.9224764035412492680, 0.9299762117001212358, 0.9374760198589933147, 0.9449758280178651715, 0.9524756361767371393, 0.9599754443356091071, 0.9674752524944810750, 0.9749750606533529318, 0.9824748688122248996, 0.9899746769710968675, 0.9974744851299687243, 1.000000000000000000 ),
 .UNSPECIFIED. ) 
 CURVE ( )  GEOMETRIC_REPRESENTATION_ITEM ( )  RATIONAL_B_SPLINE_CURVE ( ( 1.000000000000000000, 0.8660254037844387076, 1.000000000000000000, 0.8660254037844387076, 1.000000000000000000, 0.8660254037844387076, 1.000000000000000000, 0.8660254037844387076, 1.000000000000000000, 0.8660254037844387076, 1.000000000000000000, 0.8660254037844387076, 1.000000000000000000, 0.8660254037844387076, 1.000000000000000000, 0.8660254037844387076, 1.000000000000000000, 0.8660254037844387076, 1.000000000000000000, 0.8660254037844387076, 1.000000000000000000, 0.8660254037844387076, 1.000000000000000000, 0.8660254037844387076, 1.000000000000000000, 0.8660254037844387076, 1.000000000000000000, 0.8660254037844387076, 1.000000000000000000, 0.8660254037844387076, 1.000000000000000000, 0.8660254037844387076, 1.000000000000000000, 0.8660254037844387076, 1.000000000000000000, 0.8660254037844387076, 1.000000000000000000, 0.8660254037844387076, 1.000000000000000000, 0.8660254037844387076, 1.000000000000000000, 0.8660254037844387076, 1.000000000000000000, 0.8660254037844387076, 1.000000000000000000, 0.8660254037844387076, 1.000000000000000000, 0.8660254037844387076, 1.000000000000000000, 0.8660254037844387076, 1.000000000000000000, 0.8660254037844387076, 1.000000000000000000, 0.8660254037844387076, 1.000000000000000000, 0.8660254037844387076, 1.000000000000000000, 0.8660254037844387076, 1.000000000000000000, 0.8660254037844387076, 1.000000000000000000, 0.8660254037844387076, 1.000000000000000000, 0.8660254037844387076, 1.000000000000000000, 0.8660254037844387076, 1.000000000000000000, 0.8660254037844387076, 1.000000000000000000, 0.8660254037844387076, 1.000000000000000000, 0.8660254037844387076, 1.000000000000000000, 0.8660254037844387076, 1.000000000000000000, 0.8660254037844387076, 1.000000000000000000, 0.8660254037844387076, 1.000000000000000000, 0.8660254037844387076, 1.000000000000000000, 0.8660254037844387076, 1.000000000000000000, 0.8660254037844387076, 1.000000000000000000, 0.8660254037844387076, 1.000000000000000000, 0.8660254037844387076, 1.000000000000000000, 0.8660254037844387076, 1.000000000000000000, 0.8660254037844387076, 1.000000000000000000, 0.8660254037844387076, 1.000000000000000000, 0.8660254037844387076, 1.000000000000000000, 0.8660254037844387076, 1.000000000000000000, 0.8660254037844387076, 1.000000000000000000, 0.8660254037844387076, 1.000000000000000000, 0.8660254037844387076, 1.000000000000000000, 0.8660254037844387076, 1.000000000000000000, 0.8660254037844387076, 1.000000000000000000, 0.8660254037844387076, 1.000000000000000000, 0.8660254037844387076, 1.000000000000000000, 0.8660254037844387076, 1.000000000000000000, 0.8660254037844387076, 1.000000000000000000, 0.8660254037844387076, 1.000000000000000000, 0.8660254037844387076, 1.000000000000000000, 0.8660254037844387076, 1.000000000000000000, 0.8660254037844387076, 1.000000000000000000, 0.8660254037844387076, 1.000000000000000000, 0.8660254037844387076, 1.000000000000000000, 0.8660254037844387076, 1.000000000000000000, 0.8660254037844387076, 1.000000000000000000, 0.8660254037844387076, 1.000000000000000000, 0.8660254037844387076, 1.000000000000000000, 0.8660254037844387076, 1.000000000000000000, 0.8660254037844387076, 1.000000000000000000, 0.8660254037844387076, 1.000000000000000000, 0.8660254037844387076, 1.000000000000000000, 0.8660254037844387076, 1.000000000000000000, 0.8660254037844387076, 1.000000000000000000, 0.8660254037844387076, 1.000000000000000000, 0.8660254037844387076, 1.000000000000000000, 0.8660254037844387076, 1.000000000000000000, 0.8660254037844387076, 1.000000000000000000, 0.8660254037844387076, 1.000000000000000000, 0.8660254037844387076, 1.000000000000000000, 0.8660254037844387076, 1.000000000000000000, 0.8660254037844387076, 1.000000000000000000, 0.8660254037844387076, 1.000000000000000000, 0.8660254037844387076, 1.000000000000000000, 0.8660254037844387076, 1.000000000000000000, 0.8660254037844387076, 1.000000000000000000, 0.8660254037844387076, 1.000000000000000000, 0.8660254037844387076, 1.000000000000000000, 0.8660254037844387076, 1.000000000000000000, 0.8660254037844387076, 1.000000000000000000, 0.8660254037844387076, 1.000000000000000000, 0.8660254037844387076, 1.000000000000000000, 0.8660254037844387076, 1.000000000000000000, 0.8660254037844387076, 1.000000000000000000, 0.8660254037844387076, 1.000000000000000000, 0.8660254037844387076, 1.000000000000000000, 0.8660254037844387076, 1.000000000000000000, 0.8660254037844387076, 1.000000000000000000, 0.8660254037844387076, 1.000000000000000000, 0.8660254037844387076, 1.000000000000000000, 0.8660254037844387076, 1.000000000000000000, 0.8660254037844387076, 1.000000000000000000, 0.8660254037844387076, 1.000000000000000000, 0.8660254037844387076, 1.000000000000000000, 0.8660254037844387076, 1.000000000000000000, 0.8660254037844387076, 1.000000000000000000, 0.8660254037844387076, 1.000000000000000000, 0.8660254037844387076, 1.000000000000000000, 0.8660254037844387076, 1.000000000000000000, 0.8660254037844387076, 1.000000000000000000, 0.8660254037844387076, 1.000000000000000000, 0.8660254037844387076, 1.000000000000000000, 0.8660254037844387076, 1.000000000000000000, 0.8660254037844387076, 1.000000000000000000, 0.8660254037844387076, 1.000000000000000000, 0.8660254037844387076, 1.000000000000000000, 0.8660254037844387076, 1.000000000000000000, 0.8660254037844387076, 1.000000000000000000, 0.8660254037844387076, 1.000000000000000000, 0.8660254037844387076, 1.000000000000000000, 0.8660254037844387076, 1.000000000000000000, 0.8660254037844387076, 1.000000000000000000, 0.8660254037844387076, 1.000000000000000000, 0.8660254037844387076, 1.000000000000000000, 0.8660254037844387076, 1.000000000000000000, 0.8660254037844387076, 1.000000000000000000, 0.8660254037844387076, 1.000000000000000000, 0.8660254037844387076, 1.000000000000000000, 0.8660254037844387076, 1.000000000000000000, 0.8660254037844387076, 1.000000000000000000, 0.8660254037844387076, 1.000000000000000000, 0.8660254037844387076, 1.000000000000000000, 0.8660254037844387076, 1.000000000000000000, 0.9548848677736607726, 0.9401542295229587953 ) ) 
 REPRESENTATION_ITEM ( '' )  );
#13036 = CARTESIAN_POINT ( 'NONE',  ( 15.72187500061451892, 3.027376345333613106, -5.243569643749998122 ) ) ;
#13037 = CARTESIAN_POINT ( 'NONE',  ( 17.40000000122903145, 5.773502691896255534, 3.535250795749688894E-16 ) ) ;
#13038 = CARTESIAN_POINT ( 'NONE',  ( 24.52499999999999858, 4.330127018922191873, 2.499999999999999556 ) ) ;
#13039 = CARTESIAN_POINT ( 'NONE',  ( -0.7368881354385758975, 9.859898613939513723, -34.17910028561248481 ) ) ;
#13040 = CARTESIAN_POINT ( 'NONE',  ( -1.071796769724489229, 14.56115380933863257, 34.00000000000000000 ) ) ;
#13041 = CYLINDRICAL_SURFACE ( 'NONE', #70129, 4.000000000000000000 ) ;
#13042 = CARTESIAN_POINT ( 'NONE',  ( 4.779258346327469376, 1.469247991000700582, 4.779258346327429408 ) ) ;
#13043 = CARTESIAN_POINT ( 'NONE',  ( 13.95000000000000107, -4.330127018922190985, -2.500000000000001332 ) ) ;
#13044 = CARTESIAN_POINT ( 'NONE',  ( 17.40937500061451715, -4.541064518000417216, -2.621784821875001281 ) ) ;
#13045 = CARTESIAN_POINT ( 'NONE',  ( 15.18750000000000000, -2.886751345948130876, 4.999999999999996447 ) ) ;
#13046 = CARTESIAN_POINT ( 'NONE',  ( 14.84062500061451750, 6.054752690667223547, 3.707466751127219781E-16 ) ) ;
#13047 = CARTESIAN_POINT ( 'NONE',  ( 9.918750001229033941, -5.773502691896255534, -1.060575238724906372E-15 ) ) ;
#13048 = CARTESIAN_POINT ( 'NONE',  ( 4.000000000000000000, 16.55000000000000071, 30.00000000000000000 ) ) ;
#13049 = CARTESIAN_POINT ( 'NONE',  ( 25.62187500061451573, 3.027376345333613106, -5.243569643749998122 ) ) ;
#13050 = CARTESIAN_POINT ( 'NONE',  ( 18.79687500061451289, 4.119189519843966529, -2.378215178124998275 ) ) ;
#13051 = CARTESIAN_POINT ( 'NONE',  ( 10.75312500061451715, 4.541064518000418104, -2.621784821874998173 ) ) ;
#13052 = CARTESIAN_POINT ( 'NONE',  ( 14.85937500061451644, 4.541064518000418104, -2.621784821874998173 ) ) ;
#13053 = ORIENTED_EDGE ( 'NONE', *, *, #19020, .T. ) ;
#13054 = CARTESIAN_POINT ( 'NONE',  ( 27.40312500061451573, 4.541064518000418104, -2.621784821874998173 ) ) ;
#13055 = CARTESIAN_POINT ( 'NONE',  ( 20.65312500061451573, 4.541064518000418104, -2.621784821874998173 ) ) ;
#13056 = CARTESIAN_POINT ( 'NONE',  ( 29.01562500061451644, -6.054752690667223547, -1.112240025338166033E-15 ) ) ;
#13057 = CARTESIAN_POINT ( 'NONE',  ( 3.242103837493086330E-14, 12.80000000122903536, -34.00000000000000000 ) ) ;
#13058 = CARTESIAN_POINT ( 'NONE',  ( 10.35000000000000142, -4.330127018922190985, -2.500000000000001332 ) ) ;
#13059 = CARTESIAN_POINT ( 'NONE',  ( 19.83750000122903145, -4.330127018922194537, 2.499999999999995559 ) ) ;
#13060 = DIRECTION ( 'NONE',  ( -0.000000000000000000, -0.000000000000000000, -1.000000000000000000 ) ) ;
#13061 = CARTESIAN_POINT ( 'NONE',  ( 9.384375000614516793, 5.492252693125287522, 3.363034840372157021E-16 ) ) ;
#13062 = ORIENTED_EDGE ( 'NONE', *, *, #9622, .F. ) ;
#13063 = CARTESIAN_POINT ( 'NONE',  ( 18.59999999999999787, 4.330127018922192761, -2.499999999999997780 ) ) ;
#13064 = CARTESIAN_POINT ( 'NONE',  ( 20.40000000000000213, 4.330127018922192761, -2.499999999999997780 ) ) ;
#13065 = CARTESIAN_POINT ( 'NONE',  ( 19.50937500061451857, 0.000000000000000000, 5.243569643749999010 ) ) ;
#13066 = CARTESIAN_POINT ( 'NONE',  ( 14.80312500061451608, 4.541064518000418104, -2.621784821874998173 ) ) ;
#13067 = VERTEX_POINT ( 'NONE', #48302 ) ;
#13068 = CARTESIAN_POINT ( 'NONE',  ( 9.750000000000001776, 0.000000000000000000, 4.999999999999998224 ) ) ;
#13069 = CARTESIAN_POINT ( 'NONE',  ( 4.790625000614518569, -3.027376345333610441, -5.243569643749999898 ) ) ;
#13070 = CARTESIAN_POINT ( 'NONE',  ( 9.056250001229033231, -4.330127018922190985, -2.500000000000001332 ) ) ;
#13071 = CARTESIAN_POINT ( 'NONE',  ( 11.66249999999999964, -5.773502691896255534, -1.060575238724906372E-15 ) ) ;
#13072 = CARTESIAN_POINT ( 'NONE',  ( 29.33437500061451431, -2.746126346562646425, 4.756430356249996549 ) ) ;
#13073 = CARTESIAN_POINT ( 'NONE',  ( 4.243569643749999898, 18.67812500061451431, 30.00000000000000000 ) ) ;
#13074 = CARTESIAN_POINT ( 'NONE',  ( 2.859375000614519546, 0.000000000000000000, 5.243569643749999010 ) ) ;
#13075 = CARTESIAN_POINT ( 'NONE',  ( 11.62500000000000000, -4.330127018922194537, 2.499999999999995559 ) ) ;
#13076 = CARTESIAN_POINT ( 'NONE',  ( -3.756430356250001434, 16.95312499938548356, 32.16877607737301048 ) ) ;
#13077 = CARTESIAN_POINT ( 'NONE',  ( 26.29687500061451644, -3.027376345333614438, 5.243569643749998122 ) ) ;
#13078 = ORIENTED_EDGE ( 'NONE', *, *, #9420, .T. ) ;
#13079 = CARTESIAN_POINT ( 'NONE',  ( 21.17812500061451431, 4.541064518000418104, 2.621784821874999949 ) ) ;
#13080 = CARTESIAN_POINT ( 'NONE',  ( 23.89687500061451786, 6.054752690667223547, 3.707466751127219781E-16 ) ) ;
#13081 = ADVANCED_FACE ( 'NONE', ( #32769 ), #27230, .T. ) ;
#13082 = CARTESIAN_POINT ( 'NONE',  ( 2.121784821875001281, 15.45312500061459282, -26.32496088578401938 ) ) ;
#13083 = CARTESIAN_POINT ( 'NONE',  ( 6.328125000614515550, 4.541064518000418104, 2.621784821874999949 ) ) ;
#13084 = CARTESIAN_POINT ( 'NONE',  ( 28.32187500061451502, 2.746126346562645981, -4.756430356249997438 ) ) ;
#13085 = CARTESIAN_POINT ( 'NONE',  ( 23.01562500061451644, 3.027376345333611329, 5.243569643749999010 ) ) ;
#13086 = CARTESIAN_POINT ( 'NONE',  ( 27.19687500061451502, -4.119189519843965641, -2.378215178125001383 ) ) ;
#13087 = CARTESIAN_POINT ( 'NONE',  ( 11.59687500061451892, -2.746126346562642428, -4.756430356249999214 ) ) ;
#13088 = CARTESIAN_POINT ( 'NONE',  ( 16.09687500061452070, -3.027376345333610441, -5.243569643749999898 ) ) ;
#13089 = CARTESIAN_POINT ( 'NONE',  ( 18.72187500061451360, -6.054752690667223547, -1.112240025338166033E-15 ) ) ;
#13090 = CARTESIAN_POINT ( 'NONE',  ( 26.63437500061451857, 4.541064518000418104, 2.621784821874999949 ) ) ;
#13091 = CARTESIAN_POINT ( 'NONE',  ( 4.243569643749999898, 16.03437500061451715, 30.00000000000000000 ) ) ;
#13092 = CARTESIAN_POINT ( 'NONE',  ( 6.628125000614517148, 6.421520780324663323E-16, -5.243569643749999010 ) ) ;
#13093 = CARTESIAN_POINT ( 'NONE',  ( 1.071796769724484344, 16.08259618943233704, 34.00000000000000000 ) ) ;
#13094 = CARTESIAN_POINT ( 'NONE',  ( 4.809375000614516615, -4.541064518000417216, -2.621784821875001281 ) ) ;
#13095 = CARTESIAN_POINT ( 'NONE',  ( 2.000000000000000444, 17.52499999999999858, 26.53589838486224650 ) ) ;
#13096 = CARTESIAN_POINT ( 'NONE',  ( 5.390625000614518214, 6.054752690667223547, 3.707466751127219781E-16 ) ) ;
#13097 = CARTESIAN_POINT ( 'NONE',  ( 10.58437500061451964, -4.541064518000419881, 2.621784821874995952 ) ) ;
#13098 = CARTESIAN_POINT ( 'NONE',  ( 15.93750000122903110, 6.123233995736764310E-16, -4.999999999999998224 ) ) ;
#13099 = CARTESIAN_POINT ( 'NONE',  ( 4.509375000614518569, 4.541064518000418104, -2.621784821874998173 ) ) ;
#13100 = CARTESIAN_POINT ( 'NONE',  ( 8.240625000614516082, -3.027376345333614438, 5.243569643749998122 ) ) ;
#13101 = CARTESIAN_POINT ( 'NONE',  ( -2.000000000000001776, 14.54374999877096641, 33.46410161513775705 ) ) ;
#13102 = CARTESIAN_POINT ( 'NONE',  ( 23.53125000122902932, 6.123233995736764310E-16, -4.999999999999998224 ) ) ;
#13103 = CARTESIAN_POINT ( 'NONE',  ( 16.24687500061451573, 6.054752690667223547, 3.707466751127219781E-16 ) ) ;
#13104 = CYLINDRICAL_SURFACE ( 'NONE', #36062, 4.999999999999998224 ) ;
#13105 = VERTEX_POINT ( 'NONE', #71192 ) ;
#13106 = CARTESIAN_POINT ( 'NONE',  ( 24.40312500061451573, 0.000000000000000000, 5.243569643749999010 ) ) ;
#13107 = CARTESIAN_POINT ( 'NONE',  ( 8.803125000614517859, -4.541064518000417216, -2.621784821875001281 ) ) ;
#13108 = CARTESIAN_POINT ( 'NONE',  ( 26.03437500061451715, 6.421520780324663323E-16, -5.243569643749999010 ) ) ;
#13109 = CARTESIAN_POINT ( 'NONE',  ( 10.34062500061451750, 6.054752690667223547, 3.707466751127219781E-16 ) ) ;
#13110 = CARTESIAN_POINT ( 'NONE',  ( 7.781250001229034652, 6.123233995736764310E-16, -4.999999999999998224 ) ) ;
#13111 = CARTESIAN_POINT ( 'NONE',  ( 10.38750000122903572, -4.330127018922194537, 2.499999999999995559 ) ) ;
#13112 = CARTESIAN_POINT ( 'NONE',  ( 26.09062500061451573, 6.054752690667223547, 3.707466751127219781E-16 ) ) ;
#13113 = CARTESIAN_POINT ( 'NONE',  ( 4.243569643749999898, 12.37812500061451715, -30.00000000000000000 ) ) ;
#13114 = CARTESIAN_POINT ( 'NONE',  ( 11.62500000122903465, 2.886751345948126879, 4.999999999999999112 ) ) ;
#13115 = CARTESIAN_POINT ( 'NONE',  ( 22.19062500061451715, -3.027376345333614438, 5.243569643749998122 ) ) ;
#13116 = CARTESIAN_POINT ( 'NONE',  ( 10.38750000000000107, -2.886751345948125991, -5.000000000000000000 ) ) ;
#13117 = CARTESIAN_POINT ( 'NONE',  ( 20.05312500061451431, -4.541064518000417216, -2.621784821875001281 ) ) ;
#13118 = CARTESIAN_POINT ( 'NONE',  ( 20.69999999999999929, -4.330127018922190985, -2.500000000000001332 ) ) ;
#13119 = CARTESIAN_POINT ( 'NONE',  ( 14.02500000122903323, -5.773502691896255534, -1.060575238724906372E-15 ) ) ;
#13120 = CARTESIAN_POINT ( 'NONE',  ( 10.67812500061451608, 6.421520780324663323E-16, -5.243569643749999010 ) ) ;
#13121 = VECTOR ( 'NONE', #7652, 1000.000000000000000 ) ;
#13122 = EDGE_CURVE ( 'NONE', #860, #33359, #37208, .T. ) ;
#13123 = CARTESIAN_POINT ( 'NONE',  ( 12.66562500061451502, 3.027376345333611329, 5.243569643749999010 ) ) ;
#13124 = CARTESIAN_POINT ( 'NONE',  ( 24.56250000122903288, 4.330127018922192761, -2.499999999999997780 ) ) ;
#13125 = CARTESIAN_POINT ( 'NONE',  ( 20.22187500061451715, 3.027376345333613106, -5.243569643749998122 ) ) ;
#13126 = DIRECTION ( 'NONE',  ( -1.000000000000000000, -0.000000000000000000, -0.000000000000000000 ) ) ;
#13127 = CARTESIAN_POINT ( 'NONE',  ( 6.975000001229032520, 2.886751345948129099, -4.999999999999998224 ) ) ;
#13128 = CARTESIAN_POINT ( 'NONE',  ( 8.671875000614518214, 3.027376345333611329, 5.243569643749999010 ) ) ;
#13129 = CARTESIAN_POINT ( 'NONE',  ( 26.74687500061451573, -3.027376345333614438, 5.243569643749998122 ) ) ;
#13130 = FACE_OUTER_BOUND ( 'NONE', #12493, .T. ) ;
#13131 = CARTESIAN_POINT ( 'NONE',  ( 20.69062500061451715, 6.054752690667223547, 3.707466751127219781E-16 ) ) ;
#13132 = CARTESIAN_POINT ( 'NONE',  ( 27.08437500061451786, 4.541064518000418104, 2.621784821874999949 ) ) ;
#13133 = CARTESIAN_POINT ( 'NONE',  ( -3.756430356249999214, 16.54062499938548569, 27.83122392262697176 ) ) ;
#13134 = CARTESIAN_POINT ( 'NONE',  ( 19.06875000122903074, 2.886751345948045611, -5.000000000000141220 ) ) ;
#13135 = CARTESIAN_POINT ( 'NONE',  ( 8.071875000614518569, 3.027376345333613106, -5.243569643749998122 ) ) ;
#13136 = CARTESIAN_POINT ( 'NONE',  ( 18.14062500061451644, -3.027376345333614438, 5.243569643749998122 ) ) ;
#13137 = ORIENTED_EDGE ( 'NONE', *, *, #7149, .F. ) ;
#13138 = CARTESIAN_POINT ( 'NONE',  ( 25.12499999999999645, -4.330127018922194537, 2.499999999999995559 ) ) ;
#13139 = CARTESIAN_POINT ( 'NONE',  ( 27.66562500061451146, -6.054752690667223547, -1.112240025338166033E-15 ) ) ;
#13140 = CARTESIAN_POINT ( 'NONE',  ( 4.546875000614517326, 6.054752690667223547, 3.707466751127219781E-16 ) ) ;
#13141 = CARTESIAN_POINT ( 'NONE',  ( 10.16250000122903252, 4.330127018922192761, -2.499999999999997780 ) ) ;
#13142 = CARTESIAN_POINT ( 'NONE',  ( 3.607718959681897264, 3.461971838192151818, -3.890427558041640754 ) ) ;
#13143 = CARTESIAN_POINT ( 'NONE',  ( 18.03749999999999787, -2.886751345948125991, -5.000000000000000000 ) ) ;
#13144 = CARTESIAN_POINT ( 'NONE',  ( 21.14062500061451289, 6.054752690667223547, 3.707466751127219781E-16 ) ) ;
#13145 = ORIENTED_EDGE ( 'NONE', *, *, #60921, .T. ) ;
#13146 = CARTESIAN_POINT ( 'NONE',  ( 25.76249999999999929, 2.886751345948129099, -4.999999999999998224 ) ) ;
#13147 = CARTESIAN_POINT ( 'NONE',  ( 27.34687500061451360, -3.027376345333610441, -5.243569643749999898 ) ) ;
#13148 = ORIENTED_EDGE ( 'NONE', *, *, #56915, .T. ) ;
#13149 = CARTESIAN_POINT ( 'NONE',  ( 14.20312500061451644, -4.541064518000417216, -2.621784821875001281 ) ) ;
#13150 = CARTESIAN_POINT ( 'NONE',  ( 5.728125000614515905, 6.421520780324663323E-16, -5.243569643749999010 ) ) ;
#13151 = CARTESIAN_POINT ( 'NONE',  ( 17.03437500061451715, 5.492252693125287522, 3.363034840372157021E-16 ) ) ;
#13152 = CARTESIAN_POINT ( 'NONE',  ( 3.384375000614517237, -4.541064518000419881, 2.621784821874995952 ) ) ;
#13153 = CARTESIAN_POINT ( 'NONE',  ( 16.23750000122903359, -4.330127018922194537, 2.499999999999995559 ) ) ;
#13154 = CARTESIAN_POINT ( 'NONE',  ( 20.13749999999999929, -2.886751345948129988, 4.999999999999997335 ) ) ;
#13155 = CARTESIAN_POINT ( 'NONE',  ( 28.08749999999999858, 5.773502691896255534, 3.535250795749688894E-16 ) ) ;
#13156 = CARTESIAN_POINT ( 'NONE',  ( 3.946875000614517681, -3.027376345333610441, -5.243569643749999898 ) ) ;
#13157 = CARTESIAN_POINT ( 'NONE',  ( 10.50937500061451679, 0.000000000000000000, 5.243569643749999010 ) ) ;
#13158 = CARTESIAN_POINT ( 'NONE',  ( 18.87187500061451573, 3.027376345333613106, -5.243569643749998122 ) ) ;
#13159 = CARTESIAN_POINT ( 'NONE',  ( -4.243569643749999898, 19.80312500061451786, -30.00000000000000000 ) ) ;
#13160 = VERTEX_POINT ( 'NONE', #31675 ) ;
#13161 = CARTESIAN_POINT ( 'NONE',  ( 28.79062500061451502, 6.054752690667223547, 3.707466751127219781E-16 ) ) ;
#13162 = CARTESIAN_POINT ( 'NONE',  ( 29.78437500061451715, 4.541064518000418104, 2.621784821874999949 ) ) ;
#13163 = CARTESIAN_POINT ( 'NONE',  ( 4.659375000614518925, 0.000000000000000000, 5.243569643749999010 ) ) ;
#13164 = CARTESIAN_POINT ( 'NONE',  ( 15.41250000000000142, 2.886751345948129099, -4.999999999999998224 ) ) ;
#13165 = CARTESIAN_POINT ( 'NONE',  ( 13.30312500061451786, -4.541064518000417216, -2.621784821875001281 ) ) ;
#13166 = CARTESIAN_POINT ( 'NONE',  ( -4.000000000000000888, 19.51250000000000284, 32.30940107675850470 ) ) ;
#13167 = CARTESIAN_POINT ( 'NONE',  ( 4.844509297411972781, 1.237226603047926421, -5.095516945469514170 ) ) ;
#13168 = DIRECTION ( 'NONE',  ( -1.000000000000000000, -0.000000000000000000, -0.000000000000000000 ) ) ;
#13169 = CARTESIAN_POINT ( 'NONE',  ( 19.38750000122903216, -4.330127018922194537, 2.499999999999995559 ) ) ;
#13170 = CARTESIAN_POINT ( 'NONE',  ( -1.999999999999999112, 19.34374999877096712, 26.53589838486224650 ) ) ;
#13171 = CARTESIAN_POINT ( 'NONE',  ( 19.20937500061451786, -4.119189519843965641, -2.378215178125001383 ) ) ;
#13172 = CARTESIAN_POINT ( 'NONE',  ( 6.553125000614518747, -4.541064518000417216, -2.621784821875001281 ) ) ;
#13173 = CARTESIAN_POINT ( 'NONE',  ( 24.53437500061451715, -4.541064518000419881, 2.621784821874995952 ) ) ;
#13174 = CARTESIAN_POINT ( 'NONE',  ( -2.121784821874999949, 19.33437500061451786, 26.32496088578401938 ) ) ;
#13175 = ADVANCED_FACE ( 'NONE', ( #60096 ), #9607, .T. ) ;
#13176 = CARTESIAN_POINT ( 'NONE',  ( 25.80937500061451928, 0.000000000000000000, 5.243569643749999010 ) ) ;
#13177 = CARTESIAN_POINT ( 'NONE',  ( 8.550000000000002487, -4.330127018922190985, -2.500000000000001332 ) ) ;
#13178 = CARTESIAN_POINT ( 'NONE',  ( -1.999999999999997113, 12.53750000122903430, 33.46410161513775705 ) ) ;
#13179 = CARTESIAN_POINT ( 'NONE',  ( 14.31562500061451537, 3.027376345333613106, -5.243569643749998122 ) ) ;
#13180 = CARTESIAN_POINT ( 'NONE',  ( 5.887500001229034829, -4.330127018922194537, 2.499999999999995559 ) ) ;
#13181 = CARTESIAN_POINT ( 'NONE',  ( 18.15937500061451715, 0.000000000000000000, 5.243569643749999010 ) ) ;
#13182 = CARTESIAN_POINT ( 'NONE',  ( 10.99687500061451750, -3.027376345333614438, 5.243569643749998122 ) ) ;
#13183 = CARTESIAN_POINT ( 'NONE',  ( 13.91250000122903252, 0.000000000000000000, 4.999999999999998224 ) ) ;
#13184 = ORIENTED_EDGE ( 'NONE', *, *, #8691, .F. ) ;
#13185 = CARTESIAN_POINT ( 'NONE',  ( 11.39062500061451644, -3.027376345333614438, 5.243569643749998122 ) ) ;
#13186 = CARTESIAN_POINT ( 'NONE',  ( 1.071796769724491893, 12.14509619066136814, -26.00000000000000355 ) ) ;
#13187 = CARTESIAN_POINT ( 'NONE',  ( 24.75000000122902932, -2.886751345948129988, 4.999999999999997335 ) ) ;
#13188 = CARTESIAN_POINT ( 'NONE',  ( 11.89687500061451608, -3.027376345333614438, 5.243569643749998122 ) ) ;
#13189 = CARTESIAN_POINT ( 'NONE',  ( 14.39062500061451821, 6.054752690667223547, 3.707466751127219781E-16 ) ) ;
#13190 = DIRECTION ( 'NONE',  ( -0.000000000000000000, -1.000000000000000000, -0.000000000000000000 ) ) ;
#13191 = CARTESIAN_POINT ( 'NONE',  ( 23.18437500061451573, -4.541064518000419881, 2.621784821874995952 ) ) ;
#13192 = FACE_OUTER_BOUND ( 'NONE', #56114, .T. ) ;
#13193 = DIRECTION ( 'NONE',  ( 0.000000000000000000, 0.000000000000000000, -1.000000000000000000 ) ) ;
#13194 = CARTESIAN_POINT ( 'NONE',  ( 3.140625000614516882, 6.054752690667223547, 3.707466751127219781E-16 ) ) ;
#13195 = CARTESIAN_POINT ( 'NONE',  ( -4.243569643749999898, 15.80937500061451573, -30.00000000000000000 ) ) ;
#13196 = SHAPE_REPRESENTATION ( 'valve body', ( #23765 ), #56785 ) ;
#13197 = CARTESIAN_POINT ( 'NONE',  ( 16.17187500061451644, 3.027376345333613106, -5.243569643749998122 ) ) ;
#13198 = CARTESIAN_POINT ( 'NONE',  ( 18.86250000122903359, 0.000000000000000000, 4.999999999999998224 ) ) ;
#13199 = CARTESIAN_POINT ( 'NONE',  ( 12.19687500061451679, 6.054752690667223547, 3.707466751127219781E-16 ) ) ;
#13200 = CARTESIAN_POINT ( 'NONE',  ( 2.121784821874999061, 19.65312500061451573, -33.67503911421598417 ) ) ;
#13201 = CARTESIAN_POINT ( 'NONE',  ( 20.51250000122903216, 4.330127018922192761, -2.499999999999997780 ) ) ;
#13202 = CARTESIAN_POINT ( 'NONE',  ( 11.72812500061451857, 4.541064518000418104, 2.621784821874999949 ) ) ;
#13203 = EDGE_LOOP ( 'NONE', ( #47782, #7859, #70996, #57241 ) ) ;
#13204 = ORIENTED_EDGE ( 'NONE', *, *, #17223, .F. ) ;
#13205 = CARTESIAN_POINT ( 'NONE',  ( 18.56250000000000000, 2.886751345948129099, -4.999999999999998224 ) ) ;
#13206 = CARTESIAN_POINT ( 'NONE',  ( 1.138803498474273873E-14, 15.48124999877096641, 34.00000000000000000 ) ) ;
#13207 = CARTESIAN_POINT ( 'NONE',  ( 12.49687500061451573, -3.027376345333610441, -5.243569643749999898 ) ) ;
#13208 = CARTESIAN_POINT ( 'NONE',  ( 2.991194101639602199, 4.006657223659620293, -3.099915294692820122 ) ) ;
#13209 = CARTESIAN_POINT ( 'NONE',  ( 13.42500000122903536, 2.886751345948126879, 4.999999999999999112 ) ) ;
#13210 = CARTESIAN_POINT ( 'NONE',  ( 21.82500000122903572, 2.886751345948129099, -4.999999999999998224 ) ) ;
#13211 = CARTESIAN_POINT ( 'NONE',  ( 16.71562500061451573, 3.027376345333611329, 5.243569643749999010 ) ) ;
#13212 = CARTESIAN_POINT ( 'NONE',  ( 23.84062500061451928, 6.054752690667223547, 3.707466751127219781E-16 ) ) ;
#13213 = CARTESIAN_POINT ( 'NONE',  ( 29.17500000122903714, 2.886751345948126879, 4.999999999999999112 ) ) ;
#13214 = EDGE_CURVE ( 'NONE', #12198, #11624, #4388, .T. ) ;
#13215 = CARTESIAN_POINT ( 'NONE',  ( 27.89999999999999858, -4.330127018922190985, -2.500000000000001332 ) ) ;
#13216 = CARTESIAN_POINT ( 'NONE',  ( 4.608887683030311599, 1.938663576234528341, 4.872049282877938481 ) ) ;
#13217 = CARTESIAN_POINT ( 'NONE',  ( 29.43750000000000000, 5.773502691896255534, 3.535250795749688894E-16 ) ) ;
#13218 = CARTESIAN_POINT ( 'NONE',  ( 29.92968750030725644, 0.000000000000000000, 5.121784821874998173 ) ) ;
#13219 = CARTESIAN_POINT ( 'NONE',  ( -2.121784821874996840, 14.98437500061451644, -26.32496088578401583 ) ) ;
#13220 = CARTESIAN_POINT ( 'NONE',  ( 4.200000001229033053, -2.886751345948125991, -5.000000000000000000 ) ) ;
#13221 = CARTESIAN_POINT ( 'NONE',  ( 6.150000000000003020, 0.000000000000000000, 4.999999999999998224 ) ) ;
#13222 = CARTESIAN_POINT ( 'NONE',  ( 3.009375000614516793, -4.541064518000417216, -2.621784821875001281 ) ) ;
#13223 = CARTESIAN_POINT ( 'NONE',  ( 10.17187500061451999, -6.054752690667223547, -1.112240025338166033E-15 ) ) ;
#13224 = VECTOR ( 'NONE', #28227, 1000.000000000000000 ) ;
#13225 = CARTESIAN_POINT ( 'NONE',  ( 29.27812500061451573, 4.541064518000418104, 2.621784821874999949 ) ) ;
#13226 = CARTESIAN_POINT ( 'NONE',  ( 3.999999999999999112, 10.77500000000000213, 30.00000000000000000 ) ) ;
#13227 = CARTESIAN_POINT ( 'NONE',  ( -5.378075516623670893, 8.432637420806662121, -27.31137673071734184 ) ) ;
#13228 = CARTESIAN_POINT ( 'NONE',  ( 6.909375000614518036, 0.000000000000000000, 5.243569643749999010 ) ) ;
#13229 = CARTESIAN_POINT ( 'NONE',  ( 10.13437500061451679, -4.541064518000419881, 2.621784821874995952 ) ) ;
#13230 = CARTESIAN_POINT ( 'NONE',  ( 5.362500000000003375, -5.773502691896255534, -1.060575238724906372E-15 ) ) ;
#13231 =( BOUNDED_CURVE ( )  B_SPLINE_CURVE ( 2, ( #17662, #40223, #56481, #35391, #46126, #23581, #34663, #18749, #51303 ),
 .UNSPECIFIED., .F., .F. ) 
 B_SPLINE_CURVE_WITH_KNOTS ( ( 3, 2, 2, 2, 3 ),
 ( 0.7500000000000000000, 0.7536231884057971175, 0.7608695652173913526, 0.7681159420289854767, 0.7717391304347825942 ),
 .UNSPECIFIED. ) 
 CURVE ( )  GEOMETRIC_REPRESENTATION_ITEM ( )  RATIONAL_B_SPLINE_CURVE ( ( 0.9330127018922194093, 0.9330127018922194093, 1.000000000000000000, 0.8660254037844387076, 1.000000000000000000, 0.8660254037844387076, 1.000000000000000000, 0.9330127018922194093, 0.9330127018922194093 ) ) 
 REPRESENTATION_ITEM ( '' )  );
#13232 = CARTESIAN_POINT ( 'NONE',  ( -2.121784821874996840, 15.82812500061459637, 33.67503911421598417 ) ) ;
#13233 = CARTESIAN_POINT ( 'NONE',  ( 3.177768106359410094, 25.19871980768746411, 27.55645491167268091 ) ) ;
#13234 = CARTESIAN_POINT ( 'NONE',  ( 5.475000000000000533, 6.123233995736764310E-16, -4.999999999999998224 ) ) ;
#13235 = CARTESIAN_POINT ( 'NONE',  ( 15.72187500061451537, 4.119189519843966529, 2.378215178124999607 ) ) ;
#13236 = CARTESIAN_POINT ( 'NONE',  ( 19.56562500061451715, -6.054752690667223547, -1.112240025338166033E-15 ) ) ;
#13237 = CARTESIAN_POINT ( 'NONE',  ( 12.59062500061451573, 6.054752690667223547, 3.707466751127219781E-16 ) ) ;
#13238 = CARTESIAN_POINT ( 'NONE',  ( 25.05937500061451573, 2.746126346562645981, -4.756430356249997438 ) ) ;
#13239 = CARTESIAN_POINT ( 'NONE',  ( 8.296875000614516438, -3.027376345333614438, 5.243569643749998122 ) ) ;
#13240 = CARTESIAN_POINT ( 'NONE',  ( 27.22499999999999787, 4.330127018922191873, 2.499999999999999556 ) ) ;
#13241 = CARTESIAN_POINT ( 'NONE',  ( 23.40000000122903145, -2.886751345948129988, 4.999999999999997335 ) ) ;
#13242 = LINE ( 'NONE', #24332, #69724 ) ;
#13243 = CARTESIAN_POINT ( 'NONE',  ( 12.60937500061451821, 4.541064518000418104, -2.621784821874998173 ) ) ;
#13244 = CARTESIAN_POINT ( 'NONE',  ( 27.23437500061451644, -4.541064518000419881, 2.621784821874995952 ) ) ;
#13245 = CARTESIAN_POINT ( 'NONE',  ( 3.421875000614516882, -6.054752690667223547, -1.112240025338166033E-15 ) ) ;
#13246 = CARTESIAN_POINT ( 'NONE',  ( 18.87187500061451573, 3.027376345333613106, -5.243569643749998122 ) ) ;
#13247 = CARTESIAN_POINT ( 'NONE',  ( 12.08437500061451608, 6.421520780324663323E-16, -5.243569643749999010 ) ) ;
#13248 = CARTESIAN_POINT ( 'NONE',  ( -3.756430356250000102, 17.47812499938548214, 30.00000000000000000 ) ) ;
#13249 = CARTESIAN_POINT ( 'NONE',  ( 26.32499999999999929, 4.330127018922191873, 2.499999999999999556 ) ) ;
#13250 = CARTESIAN_POINT ( 'NONE',  ( 4.000000000000000000, 12.50000000000000000, 30.00000000000000000 ) ) ;
#13251 = CARTESIAN_POINT ( 'NONE',  ( -3.000416591977282496E-16, 12.99687500061451750, -34.90005215228797653 ) ) ;
#13252 = CARTESIAN_POINT ( 'NONE',  ( 26.52187500061451431, 2.746126346562645981, -4.756430356249997438 ) ) ;
#13253 = CARTESIAN_POINT ( 'NONE',  ( 15.36562500061451608, 3.027376345333611329, 5.243569643749999010 ) ) ;
#13254 = CARTESIAN_POINT ( 'NONE',  ( 4.312500000000000000, 2.886751345948126879, 4.999999999999999112 ) ) ;
#13255 = LINE ( 'NONE', #52433, #24277 ) ;
#13256 = CARTESIAN_POINT ( 'NONE',  ( 9.299999999999998934, 0.000000000000000000, 4.999999999999998224 ) ) ;
#13257 = CARTESIAN_POINT ( 'NONE',  ( 14.40000000000000036, -4.330127018922190985, -2.500000000000001332 ) ) ;
#13258 = CARTESIAN_POINT ( 'NONE',  ( -3.999999999999999112, 19.21250000122903501, 30.00000000000000000 ) ) ;
#13260 =( BOUNDED_CURVE ( )  B_SPLINE_CURVE ( 2, ( #34344, #17357, #6281, #62789, #11826, #28811, #752, #67622, #45811 ),
 .UNSPECIFIED., .F., .F. ) 
 B_SPLINE_CURVE_WITH_KNOTS ( ( 3, 2, 2, 2, 3 ),
 ( 0.4583333333333333703, 0.4629629629629629650, 0.4722222222222222099, 0.4814814814814814548, 0.4861111111111111049 ),
 .UNSPECIFIED. ) 
 CURVE ( )  GEOMETRIC_REPRESENTATION_ITEM ( )  RATIONAL_B_SPLINE_CURVE ( ( 0.9330127018922194093, 0.9330127018922197424, 1.000000000000000000, 0.8660254037844387076, 1.000000000000000000, 0.8660254037844387076, 1.000000000000000000, 0.9330127018922194093, 0.9330127018922194093 ) ) 
 REPRESENTATION_ITEM ( '' )  );
#13259 = CARTESIAN_POINT ( 'NONE',  ( 15.03750000122903252, 6.123233995736764310E-16, -4.999999999999998224 ) ) ;
#13261 = CARTESIAN_POINT ( 'NONE',  ( 25.58437500061451431, 6.421520780324663323E-16, -5.243569643749999010 ) ) ;
#13262 = ORIENTED_EDGE ( 'NONE', *, *, #17788, .T. ) ;
#13263 = CARTESIAN_POINT ( 'NONE',  ( 20.42812500061451431, -4.541064518000419881, 2.621784821874995952 ) ) ;
#13264 = CARTESIAN_POINT ( 'NONE',  ( 4.978125000614518569, 4.541064518000418104, 2.621784821874999949 ) ) ;
#13265 = CARTESIAN_POINT ( 'NONE',  ( 19.95937500061451786, 0.000000000000000000, 5.243569643749999010 ) ) ;
#13266 = CARTESIAN_POINT ( 'NONE',  ( 5.212500000000002132, 2.886751345948126879, 4.999999999999999112 ) ) ;
#13267 = CARTESIAN_POINT ( 'NONE',  ( 7.715625000614515727, 3.027376345333611329, 5.243569643749999010 ) ) ;
#13268 = CARTESIAN_POINT ( 'NONE',  ( 21.14062500061451289, 6.054752690667223547, 3.707466751127219781E-16 ) ) ;
#13269 = CARTESIAN_POINT ( 'NONE',  ( 9.001249775931846008E-16, 14.06562500061451715, 34.90005215228797653 ) ) ;
#13270 = CARTESIAN_POINT ( 'NONE',  ( 18.93750000122903288, -4.330127018922194537, 2.499999999999995559 ) ) ;
#13271 = CARTESIAN_POINT ( 'NONE',  ( 11.48437500061451644, -4.119189519843968306, 2.378215178124996054 ) ) ;
#13272 = CARTESIAN_POINT ( 'NONE',  ( 10.56562500061451715, -6.054752690667223547, -1.112240025338166033E-15 ) ) ;
#13273 = CARTESIAN_POINT ( 'NONE',  ( 3.421875000614516882, -6.054752690667223547, -1.112240025338166033E-15 ) ) ;
#13274 = CARTESIAN_POINT ( 'NONE',  ( 29.50312500061451360, -4.541064518000417216, -2.621784821875001281 ) ) ;
#13275 = CARTESIAN_POINT ( 'NONE',  ( 22.35937500061451644, -4.541064518000417216, -2.621784821875001281 ) ) ;
#13276 = CARTESIAN_POINT ( 'NONE',  ( 13.41562500061451502, 3.027376345333613106, -5.243569643749998122 ) ) ;
#13277 = CARTESIAN_POINT ( 'NONE',  ( 24.15000000122903145, 5.773502691896255534, 3.535250795749688894E-16 ) ) ;
#13278 = CARTESIAN_POINT ( 'NONE',  ( 25.86562500061451431, -6.054752690667223547, -1.112240025338166033E-15 ) ) ;
#13279 = CARTESIAN_POINT ( 'NONE',  ( 19.43437500061451928, 4.541064518000418104, 2.621784821874999949 ) ) ;
#13280 = CARTESIAN_POINT ( 'NONE',  ( 15.17812500061451608, 6.421520780324663323E-16, -5.243569643749999010 ) ) ;
#13281 = CARTESIAN_POINT ( 'NONE',  ( -4.243569643749999898, 16.22187500061452070, 27.54997392385601529 ) ) ;
#13282 =( BOUNDED_CURVE ( )  B_SPLINE_CURVE ( 2, ( #30918, #64164, #13552, #41291, #36099, #58619, #53459, #42743, #31288 ),
 .UNSPECIFIED., .F., .F. ) 
 B_SPLINE_CURVE_WITH_KNOTS ( ( 3, 2, 2, 2, 3 ),
 ( 0.3586956521739130821, 0.3623188405797101441, 0.3695652173913043237, 0.3768115942028985588, 0.3804347826086956763 ),
 .UNSPECIFIED. ) 
 CURVE ( )  GEOMETRIC_REPRESENTATION_ITEM ( )  RATIONAL_B_SPLINE_CURVE ( ( 0.9330127018922194093, 0.9330127018922198534, 1.000000000000000000, 0.8660254037844387076, 1.000000000000000000, 0.8660254037844387076, 1.000000000000000000, 0.9330127018922188542, 0.9330127018922194093 ) ) 
 REPRESENTATION_ITEM ( '' )  );
#13283 = CARTESIAN_POINT ( 'NONE',  ( 21.10312500061451502, 4.541064518000418104, -2.621784821874998173 ) ) ;
#13284 = CARTESIAN_POINT ( 'NONE',  ( 3.300000001229034918, -2.886751345948125991, -5.000000000000000000 ) ) ;
#13285 = EDGE_LOOP ( 'NONE', ( #1039, #54108, #25522, #10541 ) ) ;
#13286 = CARTESIAN_POINT ( 'NONE',  ( 24.52499999999999858, 4.330127018922191873, 2.499999999999999556 ) ) ;
#13287 = CARTESIAN_POINT ( 'NONE',  ( 1.999999999999998668, 10.40000000000000213, -33.46410161513775705 ) ) ;
#13288 = CARTESIAN_POINT ( 'NONE',  ( 3.756430356250000546, 19.54062499938548214, 27.83122392262697886 ) ) ;
#13289 = CARTESIAN_POINT ( 'NONE',  ( 27.47812500061451502, 4.541064518000418104, 2.621784821874999949 ) ) ;
#13290 = CARTESIAN_POINT ( 'NONE',  ( 8.203125000614518214, 0.000000000000000000, 5.243569643749999010 ) ) ;
#13291 = CARTESIAN_POINT ( 'NONE',  ( 20.58750000122903145, 4.330127018922191873, 2.499999999999999556 ) ) ;
#13292 = CARTESIAN_POINT ( 'NONE',  ( 28.00312500061451715, 0.000000000000000000, 5.243569643749999010 ) ) ;
#13293 = CARTESIAN_POINT ( 'NONE',  ( 24.26249999999999929, -5.773502691896255534, -1.060575238724906372E-15 ) ) ;
#13294 = CARTESIAN_POINT ( 'NONE',  ( 2.000000000000001332, 15.76250000122903216, -26.53589838486224650 ) ) ;
#13295 = CARTESIAN_POINT ( 'NONE',  ( 10.67812500061451608, 6.421520780324663323E-16, -5.243569643749999010 ) ) ;
#13296 = ORIENTED_EDGE ( 'NONE', *, *, #66954, .T. ) ;
#13297 = ADVANCED_FACE ( 'NONE', ( #66630 ), #38177, .F. ) ;
#13298 = CARTESIAN_POINT ( 'NONE',  ( 24.77812500061451217, 4.541064518000418104, 2.621784821874999949 ) ) ;
#13299 = CARTESIAN_POINT ( 'NONE',  ( 6.628125000614517148, 6.421520780324663323E-16, -5.243569643749999010 ) ) ;
#13300 = CARTESIAN_POINT ( 'NONE',  ( 4.603125000614518569, 0.000000000000000000, 5.243569643749999010 ) ) ;
#13301 = CARTESIAN_POINT ( 'NONE',  ( 16.47187500061452070, -5.492252693125287522, -1.008910452111647106E-15 ) ) ;
#13302 = CARTESIAN_POINT ( 'NONE',  ( 0.000000000000000000, 20.00000000000000000, -30.00000000000000000 ) ) ;
#13303 = CARTESIAN_POINT ( 'NONE',  ( 12.63749999999999929, -2.886751345948125991, -5.000000000000000000 ) ) ;
#13304 = CARTESIAN_POINT ( 'NONE',  ( 12.53437500061451537, 6.421520780324663323E-16, -5.243569643749999010 ) ) ;
#13305 = CARTESIAN_POINT ( 'NONE',  ( 9.600000001229034297, -2.886751345948125991, -5.000000000000000000 ) ) ;
#13306 = CARTESIAN_POINT ( 'NONE',  ( 15.94687500061451502, -3.027376345333614438, 5.243569643749998122 ) ) ;
#13307 = CARTESIAN_POINT ( 'NONE',  ( 17.58749999999999858, -2.886751345948125991, -5.000000000000000000 ) ) ;
#13308 = CARTESIAN_POINT ( 'NONE',  ( 7.771875000614516971, 3.027376345333611329, 5.243569643749999010 ) ) ;
#13309 = CARTESIAN_POINT ( 'NONE',  ( -4.243569643749999898, 11.70312500061451644, -30.00000000000000000 ) ) ;
#13310 = CARTESIAN_POINT ( 'NONE',  ( 27.63750000122903216, 6.123233995736764310E-16, -4.999999999999998224 ) ) ;
#13311 = CARTESIAN_POINT ( 'NONE',  ( 23.07187500061451502, -4.119189519843968306, 2.378215178124996054 ) ) ;
#13312 = ORIENTED_EDGE ( 'NONE', *, *, #50852, .F. ) ;
#13313 = CARTESIAN_POINT ( 'NONE',  ( 23.54062500061451146, -3.027376345333614438, 5.243569643749998122 ) ) ;
#13314 = DIRECTION ( 'NONE',  ( 0.000000000000000000, -1.000000000000000000, 8.673617379884035472E-17 ) ) ;
#13315 = CARTESIAN_POINT ( 'NONE',  ( 26.37187500061451217, -6.054752690667223547, -1.112240025338166033E-15 ) ) ;
#13316 = CARTESIAN_POINT ( 'NONE',  ( 28.43437500061451573, 4.541064518000418104, 2.621784821874999949 ) ) ;
#13317 = CARTESIAN_POINT ( 'NONE',  ( 22.91249999999999432, -5.773502691896255534, -1.060575238724906372E-15 ) ) ;
#13318 = CARTESIAN_POINT ( 'NONE',  ( 6.665625000614515905, 3.027376345333613106, -5.243569643749998122 ) ) ;
#13319 = CARTESIAN_POINT ( 'NONE',  ( 23.44687500061451502, 0.000000000000000000, 4.756430356249998326 ) ) ;
#13320 = CARTESIAN_POINT ( 'NONE',  ( 15.68437500061451573, 6.421520780324663323E-16, -5.243569643749999010 ) ) ;
#13321 = CARTESIAN_POINT ( 'NONE',  ( 9.909375000614517148, 2.746126346562643317, 4.756430356249998326 ) ) ;
#13322 = CARTESIAN_POINT ( 'NONE',  ( 29.17500000122903714, 2.886751345948126879, 4.999999999999999112 ) ) ;
#13323 = CARTESIAN_POINT ( 'NONE',  ( 7.434375000614519280, -4.541064518000419881, 2.621784821874995952 ) ) ;
#13324 = ORIENTED_EDGE ( 'NONE', *, *, #43284, .T. ) ;
#13325 = CARTESIAN_POINT ( 'NONE',  ( 19.02187500061451786, 3.027376345333611329, 5.243569643749999010 ) ) ;
#13326 = CARTESIAN_POINT ( 'NONE',  ( -3.468515707051626151, 25.13356901665284937, 32.00919774098884574 ) ) ;
#13327 = CARTESIAN_POINT ( 'NONE',  ( 27.59999999999999787, 4.330127018922192761, -2.499999999999997780 ) ) ;
#13328 = CARTESIAN_POINT ( 'NONE',  ( 28.20937500061451786, -4.541064518000417216, -2.621784821875001281 ) ) ;
#13329 = CYLINDRICAL_SURFACE ( 'NONE', #49034, 1.500000000000000444 ) ;
#13330 = CARTESIAN_POINT ( 'NONE',  ( 27.97500000000000142, 6.123233995736764310E-16, -4.999999999999998224 ) ) ;
#13331 = ORIENTED_EDGE ( 'NONE', *, *, #43332, .T. ) ;
#13332 = CARTESIAN_POINT ( 'NONE',  ( 11.21250000000000036, -5.773502691896255534, -1.060575238724906372E-15 ) ) ;
#13333 = CARTESIAN_POINT ( 'NONE',  ( 12.00937500061451502, 2.746126346562645981, -4.756430356249997438 ) ) ;
#13334 = CARTESIAN_POINT ( 'NONE',  ( 21.10312500061451502, 4.541064518000418104, -2.621784821874998173 ) ) ;
#13335 = CARTESIAN_POINT ( 'NONE',  ( 12.59999999999999964, -4.330127018922190985, -2.500000000000001332 ) ) ;
#13336 = CARTESIAN_POINT ( 'NONE',  ( 7.650000001229034119, -2.886751345948129988, 4.999999999999997335 ) ) ;
#13337 = CARTESIAN_POINT ( 'NONE',  ( 5.503125000614516260, 0.000000000000000000, 5.243569643749999010 ) ) ;
#13338 = CARTESIAN_POINT ( 'NONE',  ( 22.05000000000000071, -4.330127018922190985, -2.500000000000001332 ) ) ;
#13339 = ADVANCED_FACE ( 'NONE', ( #32278 ), #54451, .T. ) ;
#13340 = CARTESIAN_POINT ( 'NONE',  ( 20.42812500061451431, -4.541064518000419881, 2.621784821874995952 ) ) ;
#13341 = CARTESIAN_POINT ( 'NONE',  ( 23.58749999999999858, 5.773502691896255534, 3.535250795749688401E-16 ) ) ;
#13342 = CARTESIAN_POINT ( 'NONE',  ( 25.20000000122903216, -2.886751345948129988, 4.999999999999997335 ) ) ;
#13343 = CARTESIAN_POINT ( 'NONE',  ( 1.878215178125000495, 19.46562499938548640, 26.74683588394047007 ) ) ;
#13344 = CARTESIAN_POINT ( 'NONE',  ( 5.100000000000000533, 4.330127018922192761, -2.499999999999997780 ) ) ;
#13345 = ORIENTED_EDGE ( 'NONE', *, *, #10988, .F. ) ;
#13346 = CARTESIAN_POINT ( 'NONE',  ( 20.01562500061451644, -6.054752690667223547, -1.112240025338166033E-15 ) ) ;
#13347 = CARTESIAN_POINT ( 'NONE',  ( 26.20312500061451644, 0.000000000000000000, 5.243569643749999010 ) ) ;
#13348 = CARTESIAN_POINT ( 'NONE',  ( 26.74687500061451573, -3.027376345333614438, 5.243569643749998122 ) ) ;
#13349 = CARTESIAN_POINT ( 'NONE',  ( 15.21562500061451750, 3.027376345333613106, -5.243569643749998122 ) ) ;
#13350 = CARTESIAN_POINT ( 'NONE',  ( 25.87500000122903288, 2.886751345948129099, -4.999999999999998224 ) ) ;
#13351 = CARTESIAN_POINT ( 'NONE',  ( 18.60937500061451644, 0.000000000000000000, 4.756430356249998326 ) ) ;
#13352 = CARTESIAN_POINT ( 'NONE',  ( 17.27812500061451217, -4.541064518000419881, 2.621784821874995952 ) ) ;
#13353 = CARTESIAN_POINT ( 'NONE',  ( 7.987500000000000711, -2.886751345948130876, 4.999999999999996447 ) ) ;
#13354 = CARTESIAN_POINT ( 'NONE',  ( 28.39687500061452141, 6.054752690667223547, 3.707466751127219781E-16 ) ) ;
#13355 = CARTESIAN_POINT ( 'NONE',  ( 9.759375000614516793, -4.541064518000417216, -2.621784821875001281 ) ) ;
#13356 = CARTESIAN_POINT ( 'NONE',  ( 10.43437500061451750, 4.541064518000418104, 2.621784821874999949 ) ) ;
#13357 = CARTESIAN_POINT ( 'NONE',  ( 17.85937500061451999, -4.541064518000417216, -2.621784821875001281 ) ) ;
#13358 = ORIENTED_EDGE ( 'NONE', *, *, #18629, .F. ) ;
#13359 = CARTESIAN_POINT ( 'NONE',  ( -5.989433049342594906, 8.007954590042436038, 29.59128506087665400 ) ) ;
#13360 = CARTESIAN_POINT ( 'NONE',  ( 20.61562500061451431, 3.027376345333613106, -5.243569643749998122 ) ) ;
#13361 = CARTESIAN_POINT ( 'NONE',  ( 17.70937500061451431, 0.000000000000000000, 5.243569643749999010 ) ) ;
#13362 = CARTESIAN_POINT ( 'NONE',  ( 21.89062500061451289, -3.027376345333610441, -5.243569643749999898 ) ) ;
#13363 = CARTESIAN_POINT ( 'NONE',  ( -2.828200636599751609E-16, 13.58750000000000213, 25.38119784648299770 ) ) ;
#13364 = CARTESIAN_POINT ( 'NONE',  ( 29.31562500061451715, 3.027376345333611329, 5.243569643749999010 ) ) ;
#13365 = CARTESIAN_POINT ( 'NONE',  ( 10.38750000122903572, -4.330127018922194537, 2.499999999999995559 ) ) ;
#13366 = ORIENTED_EDGE ( 'NONE', *, *, #41986, .T. ) ;
#13367 = CARTESIAN_POINT ( 'NONE',  ( 3.975000001229033852, 2.886751345948126879, 4.999999999999999112 ) ) ;
#13368 = CARTESIAN_POINT ( 'NONE',  ( 4.000000000000000000, 18.83749999999999858, -27.69059892324149530 ) ) ;
#13369 = CARTESIAN_POINT ( 'NONE',  ( 24.22500000122903430, 2.886751345948126879, 4.999999999999999112 ) ) ;
#13370 = CARTESIAN_POINT ( 'NONE',  ( 3.999999999999998668, 20.05624999877096570, 32.30940107675850470 ) ) ;
#13371 = EDGE_CURVE ( 'NONE', #11624, #54715, #37815, .T. ) ;
#13372 = CARTESIAN_POINT ( 'NONE',  ( 9.271875000614516082, -6.054752690667223547, -1.112240025338166033E-15 ) ) ;
#13373 = CARTESIAN_POINT ( 'NONE',  ( 14.87812500061451537, 4.541064518000418104, 2.621784821874999949 ) ) ;
#13374 = CARTESIAN_POINT ( 'NONE',  ( 11.52187500061451608, -6.054752690667223547, -1.112240025338166033E-15 ) ) ;
#13375 = CARTESIAN_POINT ( 'NONE',  ( 3.178125000614515638, 4.541064518000418104, 2.621784821874999949 ) ) ;
#13376 = CARTESIAN_POINT ( 'NONE',  ( 20.07187500061451857, -6.054752690667223547, -1.112240025338166033E-15 ) ) ;
#13377 = CARTESIAN_POINT ( 'NONE',  ( 6.646875000614518747, -3.027376345333610441, -5.243569643749999898 ) ) ;
#13378 = CARTESIAN_POINT ( 'NONE',  ( 1.071796769724479237, 18.89240381056766793, 25.99999999999999645 ) ) ;
#13379 = CARTESIAN_POINT ( 'NONE',  ( 7.490625000614516082, -3.027376345333610441, -5.243569643749999898 ) ) ;
#13380 = CARTESIAN_POINT ( 'NONE',  ( 18.51562500061451289, 3.027376345333611329, 5.243569643749999010 ) ) ;
#13381 = ORIENTED_EDGE ( 'NONE', *, *, #37950, .F. ) ;
#13382 = CARTESIAN_POINT ( 'NONE',  ( 15.44062500061451537, -3.027376345333614438, 5.243569643749998122 ) ) ;
#13383 = CARTESIAN_POINT ( 'NONE',  ( 11.91562500061451857, -6.054752690667223547, -1.112240025338166033E-15 ) ) ;
#13384 = CARTESIAN_POINT ( 'NONE',  ( 23.82187500061451502, 2.746126346562645981, -4.756430356249997438 ) ) ;
#13385 = CARTESIAN_POINT ( 'NONE',  ( 10.76250000000000107, -5.773502691896255534, -1.060575238724906372E-15 ) ) ;
#13386 = CARTESIAN_POINT ( 'NONE',  ( 6.375000001229031987, -5.773502691896255534, -1.060575238724906372E-15 ) ) ;
#13387 = EDGE_CURVE ( 'NONE', #51427, #3917, #54488, .T. ) ;
#13388 = CARTESIAN_POINT ( 'NONE',  ( 14.67187500061451821, -6.054752690667223547, -1.112240025338166033E-15 ) ) ;
#13389 = CARTESIAN_POINT ( 'NONE',  ( 16.46250000122903501, 4.330127018922192761, -2.499999999999997780 ) ) ;
#13390 = CARTESIAN_POINT ( 'NONE',  ( 23.62500000000000000, 4.330127018922191873, 2.499999999999999556 ) ) ;
#13391 = CARTESIAN_POINT ( 'NONE',  ( -4.243569643749999898, 18.45312500061451644, -30.00000000000000000 ) ) ;
#13392 = CARTESIAN_POINT ( 'NONE',  ( 16.31250000122903288, -4.330127018922190985, -2.500000000000001332 ) ) ;
#13393 = CYLINDRICAL_SURFACE ( 'NONE', #6436, 4.999999999999998224 ) ;
#13394 = CARTESIAN_POINT ( 'NONE',  ( 19.35937500061451644, 4.541064518000418104, -2.621784821874998173 ) ) ;
#13395 =( BOUNDED_CURVE ( )  B_SPLINE_CURVE ( 2, ( #52310, #35314, #18305, #2425, #35673, #63024, #12423 ),
 .UNSPECIFIED., .F., .F. ) 
 B_SPLINE_CURVE_WITH_KNOTS ( ( 3, 2, 2, 3 ),
 ( 0.4166666666666667407, 0.4194444444444445086, 0.4222222222222222210, 0.4249999999999999889 ),
 .UNSPECIFIED. ) 
 CURVE ( )  GEOMETRIC_REPRESENTATION_ITEM ( )  RATIONAL_B_SPLINE_CURVE ( ( 0.9999999999999973355, 0.8660254037844413721, 1.000000000000000000, 0.8660254037844387076, 1.000000000000000000, 0.8660254037844387076, 1.000000000000000000 ) ) 
 REPRESENTATION_ITEM ( '' )  );
#13396 = CARTESIAN_POINT ( 'NONE',  ( 29.92500000000000071, 4.330127018922191873, 2.499999999999999556 ) ) ;
#13397 = CARTESIAN_POINT ( 'NONE',  ( 14.91562500061451679, 3.027376345333611329, 5.243569643749999010 ) ) ;
#13398 = CARTESIAN_POINT ( 'NONE',  ( 10.55625000122903323, 4.330127018922192761, -2.499999999999997780 ) ) ;
#13399 = LINE ( 'NONE', #6797, #2348 ) ;
#13400 = CARTESIAN_POINT ( 'NONE',  ( 23.85937500061451644, 4.541064518000418104, -2.621784821874998173 ) ) ;
#13401 = CARTESIAN_POINT ( 'NONE',  ( 17.10937500061451644, 2.746126346562643317, 4.756430356249998326 ) ) ;
#13402 = CARTESIAN_POINT ( 'NONE',  ( 9.215625000614515727, -6.054752690667223547, -1.112240025338166033E-15 ) ) ;
#13403 = CARTESIAN_POINT ( 'NONE',  ( 14.89687500061451786, 6.054752690667223547, 3.707466751127219781E-16 ) ) ;
#13404 = ORIENTED_EDGE ( 'NONE', *, *, #49345, .F. ) ;
#13405 = CARTESIAN_POINT ( 'NONE',  ( 25.62187500061451573, 3.027376345333613106, -5.243569643749998122 ) ) ;
#13406 = CARTESIAN_POINT ( 'NONE',  ( 26.87812500061451360, 6.421520780324663323E-16, -5.243569643749999010 ) ) ;
#13407 = CARTESIAN_POINT ( 'NONE',  ( 18.06562500061451715, 3.027376345333611329, 5.243569643749999010 ) ) ;
#13408 = CARTESIAN_POINT ( 'NONE',  ( 29.72812500061451502, 4.541064518000418104, 2.621784821874999949 ) ) ;
#13409 = DIRECTION ( 'NONE',  ( 0.000000000000000000, 0.000000000000000000, 1.000000000000000000 ) ) ;
#13410 = CARTESIAN_POINT ( 'NONE',  ( 8.699999999999999289, 4.330127018922192761, -2.499999999999997780 ) ) ;
#13411 = CARTESIAN_POINT ( 'NONE',  ( 19.27500000122903145, 2.886751345948126879, 4.999999999999999112 ) ) ;
#13412 = CYLINDRICAL_SURFACE ( 'NONE', #6574, 4.000000000000000000 ) ;
#13413 = CARTESIAN_POINT ( 'NONE',  ( 10.92187500061451644, -4.119189519843968306, 2.378215178124996054 ) ) ;
#13414 = ORIENTED_EDGE ( 'NONE', *, *, #19199, .F. ) ;
#13415 = CARTESIAN_POINT ( 'NONE',  ( 16.72500000000000142, 6.123233995736764310E-16, -4.999999999999998224 ) ) ;
#13416 = CARTESIAN_POINT ( 'NONE',  ( 21.97500000000000142, -4.330127018922194537, 2.499999999999995559 ) ) ;
#13417 = CARTESIAN_POINT ( 'NONE',  ( 18.79687500061451644, -3.027376345333610441, -5.243569643749999898 ) ) ;
#13418 = CARTESIAN_POINT ( 'NONE',  ( 13.19062500061451537, -3.027376345333614438, 5.243569643749998122 ) ) ;
#13419 = ORIENTED_EDGE ( 'NONE', *, *, #36009, .T. ) ;
#13420 = CARTESIAN_POINT ( 'NONE',  ( -0.6945831915928805111, 10.00052343484236950, -33.93923269050669944 ) ) ;
#13421 = CARTESIAN_POINT ( 'NONE',  ( 5.690625000614516260, -3.027376345333610441, -5.243569643749999898 ) ) ;
#13422 = CARTESIAN_POINT ( 'NONE',  ( 12.00000000000000000, 0.000000000000000000, 4.999999999999998224 ) ) ;
#13423 = CARTESIAN_POINT ( 'NONE',  ( 12.56250000000000178, -5.773502691896255534, -1.060575238724906372E-15 ) ) ;
#13424 = CARTESIAN_POINT ( 'NONE',  ( 28.88437500061451502, -2.746126346562646425, 4.756430356249996549 ) ) ;
#13425 = VECTOR ( 'NONE', #18752, 1000.000000000000000 ) ;
#13426 = CARTESIAN_POINT ( 'NONE',  ( 4.243569643749999010, 16.01562500061451644, 27.54997392385601174 ) ) ;
#13427 = CARTESIAN_POINT ( 'NONE',  ( 29.42812500061451431, -4.541064518000419881, 2.621784821874995952 ) ) ;
#13428 = CARTESIAN_POINT ( 'NONE',  ( 8.737500000000002487, 5.773502691896255534, 3.535250795749688894E-16 ) ) ;
#13429 = CARTESIAN_POINT ( 'NONE',  ( 2.655984681222220721E-16, 16.35312499938548214, 25.66244784525396483 ) ) ;
#13430 = CARTESIAN_POINT ( 'NONE',  ( 23.63437500061451502, -4.541064518000419881, 2.621784821874995952 ) ) ;
#13431 = EDGE_LOOP ( 'NONE', ( #29593, #62251 ) ) ;
#13432 = CARTESIAN_POINT ( 'NONE',  ( 21.77812500061451928, -4.541064518000419881, 2.621784821874995952 ) ) ;
#13433 = CARTESIAN_POINT ( 'NONE',  ( 23.48437500061451644, 4.541064518000418104, 2.621784821874999949 ) ) ;
#13434 = CARTESIAN_POINT ( 'NONE',  ( 4.243569643749999898, 15.97812500061459495, -30.00000000000000000 ) ) ;
#13435 = CARTESIAN_POINT ( 'NONE',  ( 5.578125000614518214, -4.541064518000419881, 2.621784821874995952 ) ) ;
#13436 = CARTESIAN_POINT ( 'NONE',  ( 27.57187500061451857, 2.746126346562643317, 4.756430356249998326 ) ) ;
#13437 = CARTESIAN_POINT ( 'NONE',  ( 24.62812500061451715, 6.421520780324663323E-16, -5.243569643749999010 ) ) ;
#13438 = CARTESIAN_POINT ( 'NONE',  ( 28.13437500061451502, -2.746126346562641984, -4.756430356249999214 ) ) ;
#13439 = CARTESIAN_POINT ( 'NONE',  ( 11.14687500061451608, -2.746126346562642428, -4.756430356249999214 ) ) ;
#13440 = EDGE_CURVE ( 'NONE', #15065, #70677, #10281, .T. ) ;
#13441 = CARTESIAN_POINT ( 'NONE',  ( 15.90937500061451892, 0.000000000000000000, 5.243569643749999010 ) ) ;
#13442 = CARTESIAN_POINT ( 'NONE',  ( 24.00937500061451502, 0.000000000000000000, 5.243569643749999010 ) ) ;
#13443 = CARTESIAN_POINT ( 'NONE',  ( 9.001249775931846008E-16, 14.12187500061451750, 34.90005215228797653 ) ) ;
#13444 = CARTESIAN_POINT ( 'NONE',  ( 8.390625000614518214, -3.027376345333610441, -5.243569643749999898 ) ) ;
#13445 = CARTESIAN_POINT ( 'NONE',  ( 3.999999999999998668, 10.47500000122903430, -32.30940107675850470 ) ) ;
#13446 = CARTESIAN_POINT ( 'NONE',  ( 3.196875000614516793, 6.054752690667223547, 3.707466751127219781E-16 ) ) ;
#13447 = CYLINDRICAL_SURFACE ( 'NONE', #64280, 4.000000000000000000 ) ;
#13448 = CARTESIAN_POINT ( 'NONE',  ( 4.753125000614515372, -4.541064518000417216, -2.621784821875001281 ) ) ;
#13449 = CARTESIAN_POINT ( 'NONE',  ( 10.09687500061451715, -3.027376345333614438, 5.243569643749998122 ) ) ;
#13450 = FILL_AREA_STYLE ('',( #69271 ) ) ;
#13451 = CARTESIAN_POINT ( 'NONE',  ( 15.71250000122903501, 0.000000000000000000, 4.999999999999998224 ) ) ;
#13452 = CARTESIAN_POINT ( 'NONE',  ( 29.35312500061451502, 0.000000000000000000, 5.243569643749999010 ) ) ;
#13453 = CARTESIAN_POINT ( 'NONE',  ( 8.278125000614515727, -4.541064518000419881, 2.621784821874995952 ) ) ;
#13454 = CARTESIAN_POINT ( 'NONE',  ( -8.484601909799255319E-16, 14.13124999877096855, 34.61880215351700940 ) ) ;
#13455 = CARTESIAN_POINT ( 'NONE',  ( 21.54375000122902861, -2.886751345948129988, 4.999999999999997335 ) ) ;
#13456 = CARTESIAN_POINT ( 'NONE',  ( 16.92187500061451999, -6.054752690667223547, -1.112240025338166033E-15 ) ) ;
#13457 = CARTESIAN_POINT ( 'NONE',  ( 4.000000000000000000, 19.19374999877096499, 30.00000000000000000 ) ) ;
#13458 = ORIENTED_EDGE ( 'NONE', *, *, #53850, .F. ) ;
#13459 = CARTESIAN_POINT ( 'NONE',  ( 21.44062500061452070, -3.027376345333610441, -5.243569643749999898 ) ) ;
#13460 = CARTESIAN_POINT ( 'NONE',  ( 10.86562500061451431, 3.027376345333611329, 5.243569643749999010 ) ) ;
#13461 = CARTESIAN_POINT ( 'NONE',  ( 25.92187500061451644, -6.054752690667223547, -1.112240025338166033E-15 ) ) ;
#13462 = CARTESIAN_POINT ( 'NONE',  ( 10.71562500061451928, 3.027376345333613106, -5.243569643749998122 ) ) ;
#13463 = CARTESIAN_POINT ( 'NONE',  ( 30.00000000000000000, 0.000000000000000000, 4.999999999999998224 ) ) ;
#13464 = CARTESIAN_POINT ( 'NONE',  ( 9.600000001229034297, -2.886751345948125991, -5.000000000000000000 ) ) ;
#13465 =( BOUNDED_CURVE ( )  B_SPLINE_CURVE ( 2, ( #67418, #49694, #55594, #11258, #22687, #56323, #67771, #72584, #17146 ),
 .UNSPECIFIED., .F., .F. ) 
 B_SPLINE_CURVE_WITH_KNOTS ( ( 3, 2, 2, 2, 3 ),
 ( 0.9583333333333333703, 0.9629629629629629095, 0.9722222222222222099, 0.9814814814814815103, 0.9861111111111111605 ),
 .UNSPECIFIED. ) 
 CURVE ( )  GEOMETRIC_REPRESENTATION_ITEM ( )  RATIONAL_B_SPLINE_CURVE ( ( 0.9330127018922192983, 0.9330127018922200755, 1.000000000000000000, 0.8660254037844387076, 1.000000000000000000, 0.8660254037844387076, 1.000000000000000000, 0.9330127018922185211, 0.9330127018922194093 ) ) 
 REPRESENTATION_ITEM ( '' )  );
#13466 = CARTESIAN_POINT ( 'NONE',  ( 25.60312500061451502, 4.541064518000418104, -2.621784821874998173 ) ) ;
#13467 = CARTESIAN_POINT ( 'NONE',  ( 2.121784821875001281, 10.05312500061451608, -26.32496088578401938 ) ) ;
#13468 = CARTESIAN_POINT ( 'NONE',  ( 13.72500000122903074, 2.886751345948129099, -4.999999999999998224 ) ) ;
#13469 = CARTESIAN_POINT ( 'NONE',  ( 22.45312500061451644, 4.541064518000418104, -2.621784821874998173 ) ) ;
#13470 = CARTESIAN_POINT ( 'NONE',  ( 19.04062500061451146, -3.027376345333614438, 5.243569643749998122 ) ) ;
#13471 = CARTESIAN_POINT ( 'NONE',  ( 5.109375000614518214, 0.000000000000000000, 5.243569643749999010 ) ) ;
#13472 = CARTESIAN_POINT ( 'NONE',  ( 18.48750000000000071, -2.886751345948125991, -5.000000000000000000 ) ) ;
#13473 = CARTESIAN_POINT ( 'NONE',  ( 13.01250000122903394, 0.000000000000000000, 4.999999999999998224 ) ) ;
#13474 = EDGE_CURVE ( 'NONE', #69337, #50344, #55362, .T. ) ;
#13475 = CARTESIAN_POINT ( 'NONE',  ( 9.665625000614515017, -6.054752690667223547, -1.112240025338166033E-15 ) ) ;
#13476 = CARTESIAN_POINT ( 'NONE',  ( 13.56562500061451892, 3.027376345333611329, 5.243569643749999010 ) ) ;
#13477 = CARTESIAN_POINT ( 'NONE',  ( 24.71250000122903145, 0.000000000000000000, 4.999999999999998224 ) ) ;
#13478 = AXIS2_PLACEMENT_3D ( 'NONE', #12415, #6518, #69301 ) ;
#13479 = CARTESIAN_POINT ( 'NONE',  ( 22.80937500061451573, -4.541064518000417216, -2.621784821875001281 ) ) ;
#13480 = CARTESIAN_POINT ( 'NONE',  ( 21.15937500061451715, 4.541064518000418104, -2.621784821874998173 ) ) ;
#13481 = CARTESIAN_POINT ( 'NONE',  ( -2.928932188134523606, 4.999999999999997335, -2.928932188134523606 ) ) ;
#13482 = EDGE_CURVE ( 'NONE', #2226, #46707, #7106, .T. ) ;
#13483 = CARTESIAN_POINT ( 'NONE',  ( 6.750000001229033764, -2.886751345948129988, 4.999999999999997335 ) ) ;
#13484 = CARTESIAN_POINT ( 'NONE',  ( 5.446875000614518569, 6.054752690667223547, 3.707466751127219781E-16 ) ) ;
#13485 = CARTESIAN_POINT ( 'NONE',  ( 25.99687500061451928, -3.027376345333610441, -5.243569643749999898 ) ) ;
#13486 = CARTESIAN_POINT ( 'NONE',  ( 3.759375000614517681, 0.000000000000000000, 5.243569643749999010 ) ) ;
#13487 = VECTOR ( 'NONE', #63583, 1000.000000000000000 ) ;
#13488 = CARTESIAN_POINT ( 'NONE',  ( 22.00312500061451360, 4.541064518000418104, -2.621784821874998173 ) ) ;
#13489 = CARTESIAN_POINT ( 'NONE',  ( 25.88437500061451502, -4.541064518000419881, 2.621784821874995952 ) ) ;
#13490 = CARTESIAN_POINT ( 'NONE',  ( 1.878215178125000495, 15.97812499938548392, 26.74683588394047007 ) ) ;
#13491 = CARTESIAN_POINT ( 'NONE',  ( 3.176339285701963888, -3.861459405730729433, 3.176339285701963888 ) ) ;
#13492 = CARTESIAN_POINT ( 'NONE',  ( 27.75000000122903288, 5.773502691896255534, 3.535250795749688401E-16 ) ) ;
#13493 = CARTESIAN_POINT ( 'NONE',  ( 7.171875000614517326, 3.027376345333613106, -5.243569643749998122 ) ) ;
#13494 = CARTESIAN_POINT ( 'NONE',  ( 17.72812500061451502, -4.541064518000419881, 2.621784821874995952 ) ) ;
#13495 = VECTOR ( 'NONE', #20312, 1000.000000000000000 ) ;
#13496 = ORIENTED_EDGE ( 'NONE', *, *, #48843, .F. ) ;
#13497 = CARTESIAN_POINT ( 'NONE',  ( -3.137519842735245283E-14, 12.91250000000000142, -26.00000000000000711 ) ) ;
#13498 = CARTESIAN_POINT ( 'NONE',  ( 26.46562500061451573, 3.027376345333613106, -5.243569643749998122 ) ) ;
#13499 = CARTESIAN_POINT ( 'NONE',  ( 4.284375000614518925, -4.541064518000419881, 2.621784821874995952 ) ) ;
#13500 = CARTESIAN_POINT ( 'NONE',  ( -1.071796769724491005, 15.85759618943233207, -34.00000000000000000 ) ) ;
#13501 = DIRECTION ( 'NONE',  ( -1.000000000000000000, -0.000000000000000000, -0.000000000000000000 ) ) ;
#13502 = CARTESIAN_POINT ( 'NONE',  ( 17.43750000000000355, -2.886751345948129988, 4.999999999999997335 ) ) ;
#13503 = CARTESIAN_POINT ( 'NONE',  ( 20.27812500061451573, 4.541064518000418104, 2.621784821874999949 ) ) ;
#13504 = ADVANCED_FACE ( 'NONE', ( #22640 ), #45190, .F. ) ;
#13505 = ORIENTED_EDGE ( 'NONE', *, *, #71944, .T. ) ;
#13506 = CARTESIAN_POINT ( 'NONE',  ( 23.88749999999999929, -2.886751345948125991, -5.000000000000000000 ) ) ;
#13507 = CARTESIAN_POINT ( 'NONE',  ( 25.28437500061451715, 4.541064518000418104, 2.621784821874999949 ) ) ;
#13508 = ORIENTED_EDGE ( 'NONE', *, *, #72232, .T. ) ;
#13509 = CARTESIAN_POINT ( 'NONE',  ( 0.000000000000000000, -4.999999999999998224, 0.000000000000000000 ) ) ;
#13510 = CARTESIAN_POINT ( 'NONE',  ( 14.12812500061451715, -4.541064518000419881, 2.621784821874995952 ) ) ;
#13511 = CARTESIAN_POINT ( 'NONE',  ( 4.753125000614515372, -4.541064518000417216, -2.621784821875001281 ) ) ;
#13512 = CARTESIAN_POINT ( 'NONE',  ( 17.48437500061451644, 5.492252693125287522, 3.363034840372157021E-16 ) ) ;
#13513 = CARTESIAN_POINT ( 'NONE',  ( 29.01562500061451644, -6.054752690667223547, -1.112240025338166033E-15 ) ) ;
#13514 = CARTESIAN_POINT ( 'NONE',  ( 16.35000000122903430, -2.886751345948125991, -5.000000000000000000 ) ) ;
#13515 = CARTESIAN_POINT ( 'NONE',  ( 19.31250000000000000, -5.773502691896255534, -1.060575238724906372E-15 ) ) ;
#13516 = CARTESIAN_POINT ( 'NONE',  ( 26.21249999999999858, 2.886751345948129099, -4.999999999999998224 ) ) ;
#13517 = CARTESIAN_POINT ( 'NONE',  ( 1.626862140677534273E-15, 10.66249999999999964, -26.00000000000000355 ) ) ;
#13518 = CARTESIAN_POINT ( 'NONE',  ( 8.596875000614518925, 6.054752690667223547, 3.707466751127219781E-16 ) ) ;
#13519 = CARTESIAN_POINT ( 'NONE',  ( 19.65937500061451360, -4.541064518000417216, -2.621784821875001281 ) ) ;
#13520 = CARTESIAN_POINT ( 'NONE',  ( 3.999999999999998668, 11.37500000122903643, 27.69059892324149530 ) ) ;
#13521 = ORIENTED_EDGE ( 'NONE', *, *, #34883, .F. ) ;
#13522 = CARTESIAN_POINT ( 'NONE',  ( 28.04062500061451502, -3.027376345333614438, 5.243569643749998122 ) ) ;
#13523 = CARTESIAN_POINT ( 'NONE',  ( 3.637500000000001954, -2.886751345948125991, -5.000000000000000000 ) ) ;
#13524 = ADVANCED_FACE ( 'NONE', ( #1213 ), #28914, .F. ) ;
#13525 = CARTESIAN_POINT ( 'NONE',  ( 5.746875000614517504, -3.027376345333610441, -5.243569643749999898 ) ) ;
#13526 = CARTESIAN_POINT ( 'NONE',  ( 15.90000000000000036, 4.330127018922192761, -2.499999999999997780 ) ) ;
#13527 = CARTESIAN_POINT ( 'NONE',  ( 12.70312500061451821, 0.000000000000000000, 5.243569643749999010 ) ) ;
#13528 = CARTESIAN_POINT ( 'NONE',  ( 2.828200636599751609E-16, 19.81250000000000000, 25.38119784648299415 ) ) ;
#13529 = CARTESIAN_POINT ( 'NONE',  ( 8.418750001229032165, 2.886751345948238789, 4.999999999999807265 ) ) ;
#13530 = CARTESIAN_POINT ( 'NONE',  ( 18.52500000122903145, -5.773502691896255534, -1.060575238724906372E-15 ) ) ;
#13531 = CARTESIAN_POINT ( 'NONE',  ( 0.2033016277077261402, 10.00000000000000533, 24.00000000000001066 ) ) ;
#13532 = CARTESIAN_POINT ( 'NONE',  ( 16.84687500061451715, -2.746126346562646425, 4.756430356249996549 ) ) ;
#13533 = CARTESIAN_POINT ( 'NONE',  ( 6.703125000614516438, 4.541064518000418104, -2.621784821874998173 ) ) ;
#13534 = CARTESIAN_POINT ( 'NONE',  ( 24.79687500061451999, 6.054752690667223547, 3.707466751127219781E-16 ) ) ;
#13535 = CARTESIAN_POINT ( 'NONE',  ( 4.243569643749999010, 19.22187500061452070, 27.54997392385601174 ) ) ;
#13536 = CARTESIAN_POINT ( 'NONE',  ( 24.34687500061451715, 6.054752690667223547, 3.707466751127219781E-16 ) ) ;
#13537 = CARTESIAN_POINT ( 'NONE',  ( 6.675000000000000711, -4.330127018922194537, 2.499999999999995559 ) ) ;
#13538 = CARTESIAN_POINT ( 'NONE',  ( 4.000000000000000000, 12.20000000122903394, 32.30940107675849049 ) ) ;
#13539 = CARTESIAN_POINT ( 'NONE',  ( 14.35312500061451679, 4.541064518000418104, -2.621784821874998173 ) ) ;
#13540 = CARTESIAN_POINT ( 'NONE',  ( 7.462500001229035007, 4.330127018922192761, -2.499999999999997780 ) ) ;
#13541 = CARTESIAN_POINT ( 'NONE',  ( 12.57187500061451857, 3.027376345333613106, -5.243569643749998122 ) ) ;
#13542 = CARTESIAN_POINT ( 'NONE',  ( 3.908869731033371764, -3.117809716100492512, 3.994975926305053271 ) ) ;
#13543 = ORIENTED_EDGE ( 'NONE', *, *, #4806, .F. ) ;
#13544 = AXIS2_PLACEMENT_3D ( 'NONE', #37917, #67107, #4678 ) ;
#13545 = CARTESIAN_POINT ( 'NONE',  ( 13.56562500061451892, 3.027376345333611329, 5.243569643749999010 ) ) ;
#13546 = CARTESIAN_POINT ( 'NONE',  ( 1.071796769724491227, 19.73615380933863150, 26.00000000000000000 ) ) ;
#13547 = CARTESIAN_POINT ( 'NONE',  ( 23.28750000122903430, 4.330127018922191873, 2.499999999999999556 ) ) ;
#13548 = CARTESIAN_POINT ( 'NONE',  ( 11.67187500061451821, 3.027376345333613106, -5.243569643749998122 ) ) ;
#13549 = CARTESIAN_POINT ( 'NONE',  ( 15.10312500061451502, -4.541064518000417216, -2.621784821875001281 ) ) ;
#13550 = CARTESIAN_POINT ( 'NONE',  ( 27.39375000122903359, -2.886751345948129988, 4.999999999999997335 ) ) ;
#13551 = CARTESIAN_POINT ( 'NONE',  ( 22.99687500061451573, 6.054752690667223547, 3.707466751127219781E-16 ) ) ;
#13552 = CARTESIAN_POINT ( 'NONE',  ( 1.999999999999998668, 15.91250000122903430, 26.53589838486224650 ) ) ;
#13553 = CIRCLE ( 'NONE', #17091, 4.000000000000000000 ) ;
#13554 = DIRECTION ( 'NONE',  ( -0.000000000000000000, -1.000000000000000000, -0.000000000000000000 ) ) ;
#13555 = CARTESIAN_POINT ( 'NONE',  ( -3.999999999999999112, 19.55000000000000071, 30.00000000000000000 ) ) ;
#13556 = CARTESIAN_POINT ( 'NONE',  ( -3.000416591977282496E-16, 14.79687500061451821, -34.90005215228797653 ) ) ;
#13557 = CARTESIAN_POINT ( 'NONE',  ( 14.82187500061451679, 3.027376345333613106, -5.243569643749998122 ) ) ;
#13558 = CARTESIAN_POINT ( 'NONE',  ( 17.62500000122903288, -5.773502691896255534, -1.060575238724906372E-15 ) ) ;
#13559 = AXIS2_PLACEMENT_3D ( 'NONE', #22878, #67255, #5549 ) ;
#13560 = CARTESIAN_POINT ( 'NONE',  ( 11.33437500061451608, 4.541064518000418104, 2.621784821874999949 ) ) ;
#13561 = CARTESIAN_POINT ( 'NONE',  ( -2.121784821874999949, 9.884375000614518569, 26.32496088578401938 ) ) ;
#13562 = CARTESIAN_POINT ( 'NONE',  ( 19.05000000122903359, -2.886751345948125991, -5.000000000000000000 ) ) ;
#13563 = CARTESIAN_POINT ( 'NONE',  ( 12.36562500061451608, -6.054752690667223547, -1.112240025338166033E-15 ) ) ;
#13564 = ORIENTED_EDGE ( 'NONE', *, *, #22499, .T. ) ;
#13565 = ORIENTED_EDGE ( 'NONE', *, *, #37148, .T. ) ;
#13566 = VECTOR ( 'NONE', #55641, 1000.000000000000000 ) ;
#13567 = CARTESIAN_POINT ( 'NONE',  ( 18.26249999999999929, 2.886751345948126879, 4.999999999999999112 ) ) ;
#13568 = CARTESIAN_POINT ( 'NONE',  ( 30.00000000000000000, 6.123233995736764310E-16, -4.999999999999998224 ) ) ;
#13569 = CARTESIAN_POINT ( 'NONE',  ( 11.63437500061451857, 6.421520780324663323E-16, -5.243569643749999010 ) ) ;
#13570 = CYLINDRICAL_SURFACE ( 'NONE', #43301, 4.000000000000000000 ) ;
#13571 = CARTESIAN_POINT ( 'NONE',  ( 12.30000000122903181, -2.886751345948125991, -5.000000000000000000 ) ) ;
#13572 = CARTESIAN_POINT ( 'NONE',  ( 21.41250000122903074, 4.330127018922192761, -2.499999999999997780 ) ) ;
#13573 = CARTESIAN_POINT ( 'NONE',  ( 17.95312500061451644, 4.541064518000418104, -2.621784821874998173 ) ) ;
#13574 = CARTESIAN_POINT ( 'NONE',  ( 21.70312500061451644, 0.000000000000000000, 5.243569643749999010 ) ) ;
#13575 = CARTESIAN_POINT ( 'NONE',  ( 28.42500000122904069, -5.773502691896255534, -1.060575238724906372E-15 ) ) ;
#13576 = CARTESIAN_POINT ( 'NONE',  ( 26.73749999999999716, 5.773502691896255534, 3.535250795749688894E-16 ) ) ;
#13577 = CARTESIAN_POINT ( 'NONE',  ( 3.397178649298551179, 3.668675132081069545, -3.397178649298551179 ) ) ;
#13578 = CARTESIAN_POINT ( 'NONE',  ( 29.92500000000000071, 4.330127018922191873, 2.499999999999999556 ) ) ;
#13579 = CARTESIAN_POINT ( 'NONE',  ( 28.13437500061451502, -4.541064518000419881, 2.621784821874995952 ) ) ;
#13580 = DIRECTION ( 'NONE',  ( -0.4999999999999975575, 0.000000000000000000, 0.8660254037844400399 ) ) ;
#13581 = CARTESIAN_POINT ( 'NONE',  ( -2.121784821874996840, 15.43437500061451928, -26.32496088578401583 ) ) ;
#13582 = CARTESIAN_POINT ( 'NONE',  ( 4.575000001229033941, -5.773502691896255534, -1.060575238724906372E-15 ) ) ;
#13583 = CARTESIAN_POINT ( 'NONE',  ( 6.375000000000001776, 6.123233995736764310E-16, -4.999999999999998224 ) ) ;
#13584 = CARTESIAN_POINT ( 'NONE',  ( 27.48750000000000071, -2.886751345948091796, -5.000000000000060396 ) ) ;
#13585 = CARTESIAN_POINT ( 'NONE',  ( 9.496875000614517504, 6.054752690667223547, 3.707466751127219781E-16 ) ) ;
#13586 = CARTESIAN_POINT ( 'NONE',  ( 27.81562500061452070, 3.027376345333613106, -5.243569643749998122 ) ) ;
#13587 = DIRECTION ( 'NONE',  ( -1.000000000000000000, -0.000000000000000000, -0.000000000000000000 ) ) ;
#13588 = CARTESIAN_POINT ( 'NONE',  ( -3.039972894299037609, 9.532883912050412079, -35.18750932600423909 ) ) ;
#13589 = CARTESIAN_POINT ( 'NONE',  ( 3.999999999999999112, 17.63750000122903572, -30.00000000000000000 ) ) ;
#13590 = CARTESIAN_POINT ( 'NONE',  ( 8.446875000614518569, -3.027376345333610441, -5.243569643749999898 ) ) ;
#13591 = CARTESIAN_POINT ( 'NONE',  ( 11.48437500061451644, -4.541064518000419881, 2.621784821874995952 ) ) ;
#13592 = EDGE_CURVE ( 'NONE', #30864, #38892, #62891, .T. ) ;
#13593 = CARTESIAN_POINT ( 'NONE',  ( 4.724999999999999645, 4.330127018922191873, 2.499999999999999556 ) ) ;
#13594 = VECTOR ( 'NONE', #9100, 1000.000000000000000 ) ;
#13595 = CARTESIAN_POINT ( 'NONE',  ( -2.121784821874996840, 15.37812500061459531, 33.67503911421598417 ) ) ;
#13596 = CARTESIAN_POINT ( 'NONE',  ( 1.774929369453897232, 25.43659371523960644, 33.59414506192486982 ) ) ;
#13597 = CARTESIAN_POINT ( 'NONE',  ( 6.337499999999998579, -2.886751345948125991, -5.000000000000000000 ) ) ;
#13598 = CARTESIAN_POINT ( 'NONE',  ( 14.18437500061451573, -2.746126346562642428, -4.756430356249999214 ) ) ;
#13599 = CARTESIAN_POINT ( 'NONE',  ( 20.91562500061451502, -6.054752690667223547, -1.112240025338166033E-15 ) ) ;
#13600 = CARTESIAN_POINT ( 'NONE',  ( 12.02812500061451573, 6.421520780324663323E-16, -5.243569643749999010 ) ) ;
#13601 = CARTESIAN_POINT ( 'NONE',  ( 23.44687500061451502, 0.000000000000000000, 4.756430356249998326 ) ) ;
#13602 = CARTESIAN_POINT ( 'NONE',  ( 9.571875000614518569, 3.027376345333611329, 5.243569643749999010 ) ) ;
#13603 = CARTESIAN_POINT ( 'NONE',  ( 26.06250000000000000, -5.773502691896255534, -1.060575238724906372E-15 ) ) ;
#13604 = CARTESIAN_POINT ( 'NONE',  ( 23.17500000122903359, 2.886751345948129099, -4.999999999999998224 ) ) ;
#13605 = CARTESIAN_POINT ( 'NONE',  ( 0.000000000000000000, 27.50000000000000000, 30.00000000000000000 ) ) ;
#13606 = AXIS2_PLACEMENT_3D ( 'NONE', #67615, #16981, #28444 ) ;
#13607 = CARTESIAN_POINT ( 'NONE',  ( 12.68437500061451573, 4.541064518000418104, 2.621784821874999949 ) ) ;
#13608 = CARTESIAN_POINT ( 'NONE',  ( 25.47187500061451715, -6.054752690667223547, -1.112240025338166033E-15 ) ) ;
#13609 = CARTESIAN_POINT ( 'NONE',  ( 3.721875000614518036, 3.027376345333611329, 5.243569643749999010 ) ) ;
#13610 = CARTESIAN_POINT ( 'NONE',  ( 24.26250000122903216, 0.000000000000000000, 4.999999999999998224 ) ) ;
#13611 = CARTESIAN_POINT ( 'NONE',  ( 19.47187500061451360, 3.027376345333611329, 5.243569643749999010 ) ) ;
#13612 = CARTESIAN_POINT ( 'NONE',  ( 11.03437500061451715, -4.541064518000419881, 2.621784821874995952 ) ) ;
#13613 = CARTESIAN_POINT ( 'NONE',  ( 3.756430356250000102, 12.64062499938548356, 30.00000000000000000 ) ) ;
#13614 = CARTESIAN_POINT ( 'NONE',  ( 24.29999999999999716, -4.330127018922190985, -2.500000000000001332 ) ) ;
#13615 = CARTESIAN_POINT ( 'NONE',  ( 2.655984681222220721E-16, 19.95312499938548356, 25.66244784525396483 ) ) ;
#13616 = CARTESIAN_POINT ( 'NONE',  ( -4.243569643749997233, 11.34687500061451892, -27.54997392385601174 ) ) ;
#13617 = CARTESIAN_POINT ( 'NONE',  ( 25.99687500061451928, -2.746126346562642428, -4.756430356249999214 ) ) ;
#13618 = CARTESIAN_POINT ( 'NONE',  ( 14.20312500061451644, -4.541064518000417216, -2.621784821875001281 ) ) ;
#13619 = CARTESIAN_POINT ( 'NONE',  ( 4.050000000000001599, -4.330127018922190985, -2.500000000000001332 ) ) ;
#13620 =( BOUNDED_CURVE ( )  B_SPLINE_CURVE ( 2, ( #43932, #5133, #321, #28385, #60532, #10670, #44304, #43565, #60904, #9939, #72362, #56463, #32477, #15465, #55010, #10307, #38381, #50565, #39115, #26945, #62000, #11401, #49470, #73092, #4416, #4771, #22473, #55377, #61631, #45024, #72003, #33920, #16564, #22116, #5854, #50923, #49838, #44672, #66834, #16205, #21378, #66458, #15835, #38756, #61277, #33200, #55739, #17644, #23193, #52012, #7660, #28744, #35013, #51284, #12119, #41294, #17289, #12839, #12486, #18007, #18369, #30200, #63804, #686, #40939, #6216, #35373, #6586, #23560, #69007, #45747, #57173, #62726, #68283, #62364, #29475, #63084, #68644, #29835, #63453, #6944, #40204, #34644, #57542, #1413, #58255, #22830, #23920, #52370, #1775, #24287, #57896, #29116, #46835, #52731, #7304, #46107, #51650, #45382, #1051, #35735, #40565, #46470, #67918, #69374, #39851, #11761, #18730, #13195, #34278, #56810, #2485, #36833, #32024, #60085, #19093, #42383, #2852, #2136, #19457, #41648, #59347, #42746, #8029, #8758, #31665, #19831, #64168, #30565, #54198, #24647, #65637, #71181, #58623, #9128, #13556, #36468, #65266, #42017, #20191, #3595, #30921, #70816, #53091, #70455, #69723, #8391, #9495, #47926, #47553, #14654, #26117, #48656, #36102, #37197, #53833, #25011, #47193, #70082, #64538, #31292, #64905, #3227, #13931, #20554, #58986, #53462, #25382, #43111, #14295, #25755, #48291, #59720, #15025, #37562, #39036, #71556, #67121, #5413, #16478, #22032, #55655, #27953, #61550, #44589, #5051, #33473, #44218, #49756, #50120, #32386, #38673, #72283, #10952, #56022, #15387, #66007, #61195, #43849, #37929, #50485, #21296, #54925, #20931, #10590, #21661, #27220, #73010, #72651, #33118, #22394, #66750, #43483, #16120, #39398, #61917, #66375, #44943, #67481, #54560, #16844, #26859, #11322, #3962, #26485, #4690, #15751, #49026, #60448, #9857, #4334, #38290, #49390, #71921, #60817, #27588, #10224, #32759, #55296, #51928, #68562, #18646, #41210, #35288, #62288, #56386, #23479, #57456, #11684, #6136, #17920, #1325, #39772, #40483, #63368, #51569, #243, #34199, #12753, #33843, #24196, #56733, #62999, #1687, #50843, #34929, #57090, #17566, #63718 ),
 .UNSPECIFIED., .F., .F. ) 
 B_SPLINE_CURVE_WITH_KNOTS ( ( 3, 2, 2, 2, 2, 2, 2, 2, 2, 2, 2, 2, 2, 2, 2, 2, 2, 2, 2, 2, 2, 2, 2, 2, 2, 2, 2, 2, 2, 2, 2, 2, 2, 2, 2, 2, 2, 2, 2, 2, 2, 2, 2, 2, 2, 2, 2, 2, 2, 2, 2, 2, 2, 2, 2, 2, 2, 2, 2, 2, 2, 2, 2, 2, 2, 2, 2, 2, 2, 2, 2, 2, 2, 2, 2, 2, 2, 2, 2, 2, 2, 2, 2, 2, 2, 2, 2, 2, 2, 2, 2, 2, 2, 2, 2, 2, 2, 2, 2, 2, 2, 2, 2, 2, 2, 2, 2, 2, 2, 2, 2, 2, 2, 2, 2, 2, 2, 2, 2, 2, 2, 2, 2, 2, 2, 2, 2, 2, 2, 2, 2, 2, 2, 2, 3 ),
 ( 0.000000000000000000, 0.007499808062934601276, 0.01499961612586920255, 0.02249942418880380296, 0.02999923225173840510, 0.03749904031467300725, 0.04499884837760760592, 0.05249865644054221153, 0.05999846450347681021, 0.06749827256641140194, 0.07499808062934601449, 0.08249788869228059929, 0.08999769675521521184, 0.09749750481814981051, 0.1049973128810844231, 0.1124971209440190079, 0.1199969290069536204, 0.1274967370698882330, 0.1349965451328228039, 0.1424963531957574303, 0.1499961612586920290, 0.1574959693216266277, 0.1649957773845611986, 0.1724955854474958250, 0.1799953935104304237, 0.1874952015733650224, 0.1949950096362996210, 0.2024948176992342197, 0.2099946257621688461, 0.2174944338251034170, 0.2249942418880380157, 0.2324940499509726144, 0.2399938580139072408, 0.2474936660768418395, 0.2549934741397764659, 0.2624932822027110646, 0.2699930902656456078, 0.2774928983285802619, 0.2849927063915148606, 0.2924925144544494038, 0.2999923225173840580, 0.3074921305803186011, 0.3149919386432532553, 0.3224917467061878540, 0.3299915547691223972, 0.3374913628320570513, 0.3449911708949916500, 0.3524909789579262487, 0.3599907870208608474, 0.3674905950837954460, 0.3749904031467300447, 0.3824902112096646434, 0.3899900192725992421, 0.3974898273355338407, 0.4049896353984684394, 0.4124894434614030381, 0.4199892515243376923, 0.4274890595872722354, 0.4349888676502068341, 0.4424886757131414883, 0.4499884837760760314, 0.4574882918390106856, 0.4649880999019452288, 0.4724879079648798275, 0.4799877160278144816, 0.4874875240907490248, 0.4949873321536836790, 0.5024871402166182222, 0.5099869482795529319, 0.5174867563424874195, 0.5249865644054221292, 0.5324863724683566168, 0.5399861805312912155, 0.5474859885942259252, 0.5549857966571605239, 0.5624856047200950115, 0.5699854127830297212, 0.5774852208459643199, 0.5849850289088988076, 0.5924848369718334062, 0.5999846450347681159, 0.6074844530977027146, 0.6149842611606372023, 0.6224840692235719120, 0.6299838772865065106, 0.6374836853494409983, 0.6449834934123757080, 0.6524833014753103066, 0.6599831095382447943, 0.6674829176011795040, 0.6749827256641141027, 0.6824825337270487013, 0.6899823417899833000, 0.6974821498529178987, 0.7049819579158524974, 0.7124817659787869850, 0.7199815740417216947, 0.7274813821046562934, 0.7349811901675908921, 0.7424809982305254907, 0.7499808062934600894, 0.7574806143563946881, 0.7649804224193292868, 0.7724802304822638854, 0.7799800385451984841, 0.7874798466081331938, 0.7949796546710676814, 0.8024794627340022801, 0.8099792707969368788, 0.8174790788598714775, 0.8249788869228060761, 0.8324786949857406748, 0.8399785030486753845, 0.8474783111116098722, 0.8549781191745444708, 0.8624779272374791805, 0.8699777353004136682, 0.8774775433633482669, 0.8849773514262829766, 0.8924771594892175752, 0.8999769675521520629, 0.9074767756150867726, 0.9149765836780213712, 0.9224763917409558589, 0.9299761998038904576, 0.9374760078668251673, 0.9449758159297596549, 0.9524756239926942536, 0.9599754320556289633, 0.9674752401185635620, 0.9749750481814980496, 0.9824748562444327593, 0.9899746643073673580, 0.9974744723703018456, 1.000000000000000000 ),
 .UNSPECIFIED. ) 
 CURVE ( )  GEOMETRIC_REPRESENTATION_ITEM ( )  RATIONAL_B_SPLINE_CURVE ( ( 1.000000000000000000, 0.8660254037844387076, 1.000000000000000000, 0.8660254037844387076, 1.000000000000000000, 0.8660254037844387076, 1.000000000000000000, 0.8660254037844387076, 1.000000000000000000, 0.8660254037844387076, 1.000000000000000000, 0.8660254037844387076, 1.000000000000000000, 0.8660254037844387076, 1.000000000000000000, 0.8660254037844387076, 1.000000000000000000, 0.8660254037844387076, 1.000000000000000000, 0.8660254037844387076, 1.000000000000000000, 0.8660254037844387076, 1.000000000000000000, 0.8660254037844387076, 1.000000000000000000, 0.8660254037844387076, 1.000000000000000000, 0.8660254037844387076, 1.000000000000000000, 0.8660254037844387076, 1.000000000000000000, 0.8660254037844387076, 1.000000000000000000, 0.8660254037844387076, 1.000000000000000000, 0.8660254037844387076, 1.000000000000000000, 0.8660254037844387076, 1.000000000000000000, 0.8660254037844387076, 1.000000000000000000, 0.8660254037844387076, 1.000000000000000000, 0.8660254037844387076, 1.000000000000000000, 0.8660254037844387076, 1.000000000000000000, 0.8660254037844387076, 1.000000000000000000, 0.8660254037844387076, 1.000000000000000000, 0.8660254037844387076, 1.000000000000000000, 0.8660254037844387076, 1.000000000000000000, 0.8660254037844387076, 1.000000000000000000, 0.8660254037844387076, 1.000000000000000000, 0.8660254037844387076, 1.000000000000000000, 0.8660254037844387076, 1.000000000000000000, 0.8660254037844387076, 1.000000000000000000, 0.8660254037844387076, 1.000000000000000000, 0.8660254037844387076, 1.000000000000000000, 0.8660254037844387076, 1.000000000000000000, 0.8660254037844387076, 1.000000000000000000, 0.8660254037844387076, 1.000000000000000000, 0.8660254037844387076, 1.000000000000000000, 0.8660254037844387076, 1.000000000000000000, 0.8660254037844387076, 1.000000000000000000, 0.8660254037844387076, 1.000000000000000000, 0.8660254037844387076, 1.000000000000000000, 0.8660254037844387076, 1.000000000000000000, 0.8660254037844387076, 1.000000000000000000, 0.8660254037844387076, 1.000000000000000000, 0.8660254037844387076, 1.000000000000000000, 0.8660254037844387076, 1.000000000000000000, 0.8660254037844387076, 1.000000000000000000, 0.8660254037844387076, 1.000000000000000000, 0.8660254037844387076, 1.000000000000000000, 0.8660254037844387076, 1.000000000000000000, 0.8660254037844387076, 1.000000000000000000, 0.8660254037844387076, 1.000000000000000000, 0.8660254037844387076, 1.000000000000000000, 0.8660254037844387076, 1.000000000000000000, 0.8660254037844387076, 1.000000000000000000, 0.8660254037844387076, 1.000000000000000000, 0.8660254037844387076, 1.000000000000000000, 0.8660254037844387076, 1.000000000000000000, 0.8660254037844387076, 1.000000000000000000, 0.8660254037844387076, 1.000000000000000000, 0.8660254037844387076, 1.000000000000000000, 0.8660254037844387076, 1.000000000000000000, 0.8660254037844387076, 1.000000000000000000, 0.8660254037844387076, 1.000000000000000000, 0.8660254037844387076, 1.000000000000000000, 0.8660254037844387076, 1.000000000000000000, 0.8660254037844387076, 1.000000000000000000, 0.8660254037844387076, 1.000000000000000000, 0.8660254037844387076, 1.000000000000000000, 0.8660254037844387076, 1.000000000000000000, 0.8660254037844387076, 1.000000000000000000, 0.8660254037844387076, 1.000000000000000000, 0.8660254037844387076, 1.000000000000000000, 0.8660254037844387076, 1.000000000000000000, 0.8660254037844387076, 1.000000000000000000, 0.8660254037844387076, 1.000000000000000000, 0.8660254037844387076, 1.000000000000000000, 0.8660254037844387076, 1.000000000000000000, 0.8660254037844387076, 1.000000000000000000, 0.8660254037844387076, 1.000000000000000000, 0.8660254037844387076, 1.000000000000000000, 0.8660254037844387076, 1.000000000000000000, 0.8660254037844387076, 1.000000000000000000, 0.8660254037844387076, 1.000000000000000000, 0.8660254037844387076, 1.000000000000000000, 0.8660254037844387076, 1.000000000000000000, 0.8660254037844387076, 1.000000000000000000, 0.8660254037844387076, 1.000000000000000000, 0.8660254037844387076, 1.000000000000000000, 0.8660254037844387076, 1.000000000000000000, 0.8660254037844387076, 1.000000000000000000, 0.8660254037844387076, 1.000000000000000000, 0.8660254037844387076, 1.000000000000000000, 0.8660254037844387076, 1.000000000000000000, 0.8660254037844387076, 1.000000000000000000, 0.8660254037844387076, 1.000000000000000000, 0.8660254037844387076, 1.000000000000000000, 0.8660254037844387076, 1.000000000000000000, 0.8660254037844387076, 1.000000000000000000, 0.8660254037844387076, 1.000000000000000000, 0.8660254037844387076, 1.000000000000000000, 0.8660254037844387076, 1.000000000000000000, 0.8660254037844387076, 1.000000000000000000, 0.8660254037844387076, 1.000000000000000000, 0.8660254037844387076, 1.000000000000000000, 0.8660254037844387076, 1.000000000000000000, 0.8660254037844387076, 1.000000000000000000, 0.8660254037844387076, 1.000000000000000000, 0.8660254037844387076, 1.000000000000000000, 0.8660254037844387076, 1.000000000000000000, 0.8660254037844387076, 1.000000000000000000, 0.8660254037844387076, 1.000000000000000000, 0.8660254037844387076, 1.000000000000000000, 0.8660254037844387076, 1.000000000000000000, 0.8660254037844387076, 1.000000000000000000, 0.8660254037844387076, 1.000000000000000000, 0.8660254037844387076, 1.000000000000000000, 0.8660254037844387076, 1.000000000000000000, 0.8660254037844387076, 1.000000000000000000, 0.8660254037844387076, 1.000000000000000000, 0.8660254037844387076, 1.000000000000000000, 0.8660254037844387076, 1.000000000000000000, 0.8660254037844387076, 1.000000000000000000, 0.8660254037844387076, 1.000000000000000000, 0.8660254037844387076, 1.000000000000000000, 0.8660254037844387076, 1.000000000000000000, 0.8660254037844387076, 1.000000000000000000, 0.8660254037844387076, 1.000000000000000000, 0.8660254037844387076, 1.000000000000000000, 0.8660254037844387076, 1.000000000000000000, 0.8660254037844387076, 1.000000000000000000, 0.8660254037844387076, 1.000000000000000000, 0.9548846395026737710, 0.9401540804572410259 ) ) 
 REPRESENTATION_ITEM ( '' )  );
#13621 = DIRECTION ( 'NONE',  ( 1.000000000000000000, 0.000000000000000000, 0.000000000000000000 ) ) ;
#13622 = DIRECTION ( 'NONE',  ( -1.000000000000000000, -0.000000000000000000, -0.000000000000000000 ) ) ;
#13623 = CARTESIAN_POINT ( 'NONE',  ( 15.45000000000000107, 4.330127018922192761, -2.499999999999997780 ) ) ;
#13624 = ADVANCED_FACE ( 'NONE', ( #63248 ), #68441, .F. ) ;
#13625 = CARTESIAN_POINT ( 'NONE',  ( -3.000416591977282496E-16, 10.24062500061451608, 25.09994784771203058 ) ) ;
#13626 = CARTESIAN_POINT ( 'NONE',  ( 13.61250000122903359, -4.330127018922190985, -2.500000000000001332 ) ) ;
#13627 = CARTESIAN_POINT ( 'NONE',  ( 25.95937500061451431, -4.541064518000417216, -2.621784821875001281 ) ) ;
#13628 = CARTESIAN_POINT ( 'NONE',  ( 30.00000000000000000, 6.123233995736764310E-16, -4.999999999999998224 ) ) ;
#13629 = VERTEX_POINT ( 'NONE', #17095 ) ;
#13630 = CARTESIAN_POINT ( 'NONE',  ( 19.04062500061451146, -3.027376345333614438, 5.243569643749998122 ) ) ;
#13631 = CARTESIAN_POINT ( 'NONE',  ( 3.328125000614516438, -4.541064518000419881, 2.621784821874995952 ) ) ;
#13632 = CARTESIAN_POINT ( 'NONE',  ( 19.28437500061451360, 6.421520780324663323E-16, -5.243569643749999010 ) ) ;
#13633 = CARTESIAN_POINT ( 'NONE',  ( 29.70937500061451431, 4.541064518000418104, -2.621784821874998173 ) ) ;
#13634 = CARTESIAN_POINT ( 'NONE',  ( 7.565625000614518036, 3.027376345333613106, -5.243569643749998122 ) ) ;
#13635 = CARTESIAN_POINT ( 'NONE',  ( 22.34062500061451573, -3.027376345333610441, -5.243569643749999898 ) ) ;
#13636 = CARTESIAN_POINT ( 'NONE',  ( -4.243569643749999898, 16.20312500061451644, 30.00000000000000000 ) ) ;
#13637 = CARTESIAN_POINT ( 'NONE',  ( 18.56250000122903288, -4.330127018922190985, -2.500000000000001332 ) ) ;
#13638 = CARTESIAN_POINT ( 'NONE',  ( 12.42187500061451821, -5.492252693125287522, -1.008910452111647106E-15 ) ) ;
#13639 = CARTESIAN_POINT ( 'NONE',  ( 8.953125000614518214, 4.541064518000418104, -2.621784821874998173 ) ) ;
#13640 = CARTESIAN_POINT ( 'NONE',  ( 4.246875000614519280, -3.027376345333614438, 5.243569643749998122 ) ) ;
#13641 = CARTESIAN_POINT ( 'NONE',  ( 3.159375000614518036, 4.541064518000418104, -2.621784821874998173 ) ) ;
#13642 = CARTESIAN_POINT ( 'NONE',  ( 21.90937500061451715, -4.541064518000417216, -2.621784821875001281 ) ) ;
#13643 = CARTESIAN_POINT ( 'NONE',  ( 14.46562500061451750, 3.027376345333611329, 5.243569643749999010 ) ) ;
#13644 = CARTESIAN_POINT ( 'NONE',  ( 23.88750000122903216, -4.330127018922194537, 2.499999999999995559 ) ) ;
#13645 = CARTESIAN_POINT ( 'NONE',  ( 24.81562500061451715, 3.027376345333611329, 5.243569643749999010 ) ) ;
#13646 = CARTESIAN_POINT ( 'NONE',  ( 18.98437500061451644, 4.541064518000418104, 2.621784821874999949 ) ) ;
#13647 = CARTESIAN_POINT ( 'NONE',  ( 14.31562500061451537, 3.027376345333613106, -5.243569643749998122 ) ) ;
#13648 = CARTESIAN_POINT ( 'NONE',  ( 2.121784821874999061, 17.45937500061451786, 26.32496088578401583 ) ) ;
#13649=STYLED_ITEM('',(#73144),#45331);
#13650 = CARTESIAN_POINT ( 'NONE',  ( 18.62812500061451715, -4.541064518000419881, 2.621784821874995952 ) ) ;
#13651 = CARTESIAN_POINT ( 'NONE',  ( 10.01250000000000107, 2.886751345948129099, -4.999999999999997335 ) ) ;
#13652 = ORIENTED_EDGE ( 'NONE', *, *, #19932, .T. ) ;
#13653 = CARTESIAN_POINT ( 'NONE',  ( 26.17500000000000071, 6.123233995736764310E-16, -4.999999999999998224 ) ) ;
#13654 = CARTESIAN_POINT ( 'NONE',  ( -3.999999999999999556, 11.41250000000000142, -32.30940107675850470 ) ) ;
#13655 = CARTESIAN_POINT ( 'NONE',  ( 4.818692141996693046, -1.334243621178544226, 4.818692141997074074 ) ) ;
#13656=STYLED_ITEM('',(#73130),#22240);
#13657 = CARTESIAN_POINT ( 'NONE',  ( 26.99062500061451431, 6.054752690667223547, 3.707466751127219781E-16 ) ) ;
#13658 = CARTESIAN_POINT ( 'NONE',  ( 7.228125000614517681, 4.541064518000418104, 2.621784821874999949 ) ) ;
#13659 = CARTESIAN_POINT ( 'NONE',  ( 19.68750000122903288, 4.330127018922191873, 2.499999999999999556 ) ) ;
#13660 = CARTESIAN_POINT ( 'NONE',  ( 24.77812500061451217, 4.541064518000418104, 2.621784821874999949 ) ) ;
#13661 = CARTESIAN_POINT ( 'NONE',  ( 25.19999999999999929, -4.330127018922190985, -2.500000000000001332 ) ) ;
#13662 = CARTESIAN_POINT ( 'NONE',  ( -3.999999999999999112, 16.51250000122903216, -30.00000000000000000 ) ) ;
#13663 = CARTESIAN_POINT ( 'NONE',  ( 26.87812500061451360, 6.421520780324663323E-16, -5.243569643749999010 ) ) ;
#13664 = CARTESIAN_POINT ( 'NONE',  ( 9.328125000614518214, 6.421520780324663323E-16, -5.243569643749999010 ) ) ;
#13665 = VERTEX_POINT ( 'NONE', #51452 ) ;
#13666 = CARTESIAN_POINT ( 'NONE',  ( 24.62812500061451715, 6.421520780324663323E-16, -5.243569643749999010 ) ) ;
#13667 = CARTESIAN_POINT ( 'NONE',  ( 4.640625000614518214, -3.027376345333614438, 5.243569643749998122 ) ) ;
#13668 = VECTOR ( 'NONE', #50802, 1000.000000000000000 ) ;
#13669 = CARTESIAN_POINT ( 'NONE',  ( 14.25937500061451679, -4.119189519843965641, -2.378215178125001383 ) ) ;
#13670 = FACE_OUTER_BOUND ( 'NONE', #2202, .T. ) ;
#13671 =( BOUNDED_CURVE ( )  B_SPLINE_CURVE ( 2, ( #49234, #21503, #54767, #15959, #61033, #10431, #55863 ),
 .UNSPECIFIED., .F., .F. ) 
 B_SPLINE_CURVE_WITH_KNOTS ( ( 3, 2, 2, 3 ),
 ( 0.2916666666666667407, 0.2944444444444445086, 0.2972222222222222210, 0.2999999999999999889 ),
 .UNSPECIFIED. ) 
 CURVE ( )  GEOMETRIC_REPRESENTATION_ITEM ( )  RATIONAL_B_SPLINE_CURVE ( ( 0.9999999999999973355, 0.8660254037844413721, 1.000000000000000000, 0.8660254037844387076, 1.000000000000000000, 0.8660254037844387076, 1.000000000000000000 ) ) 
 REPRESENTATION_ITEM ( '' )  );
#13672 = CARTESIAN_POINT ( 'NONE',  ( 12.30000000000000249, 4.330127018922192761, -2.499999999999997780 ) ) ;
#13673 = CARTESIAN_POINT ( 'NONE',  ( 13.99687500061451928, 6.054752690667223547, 3.707466751127219781E-16 ) ) ;
#13674 = CARTESIAN_POINT ( 'NONE',  ( 7.762500001229033053, -4.330127018922190985, -2.500000000000001332 ) ) ;
#13675 = CARTESIAN_POINT ( 'NONE',  ( 17.59687500061451715, 6.054752690667223547, 3.707466751127219781E-16 ) ) ;
#13676 = CARTESIAN_POINT ( 'NONE',  ( 15.78749999999999964, -2.886751345948125991, -5.000000000000000000 ) ) ;
#13677 = CARTESIAN_POINT ( 'NONE',  ( 7.321875000614516793, 3.027376345333611329, 5.243569643749999010 ) ) ;
#13678 = CARTESIAN_POINT ( 'NONE',  ( -4.243569643749997233, 12.64062500061451999, -27.54997392385601174 ) ) ;
#13679 = CARTESIAN_POINT ( 'NONE',  ( -1.071796769724491005, 11.80759618943233669, -34.00000000000000000 ) ) ;
#13680 = CARTESIAN_POINT ( 'NONE',  ( 22.13437500061451146, -2.746126346562646425, 4.756430356249996549 ) ) ;
#13681 = ORIENTED_EDGE ( 'NONE', *, *, #27532, .T. ) ;
#13682 = CARTESIAN_POINT ( 'NONE',  ( 25.56562500061452070, 3.027376345333613106, -5.243569643749998122 ) ) ;
#13683 = CARTESIAN_POINT ( 'NONE',  ( -4.243569643749998122, 10.44687500061451679, 32.45002607614398471 ) ) ;
#13684 = CARTESIAN_POINT ( 'NONE',  ( 1.071796769724488785, 20.45134618820329919, 34.00000000000000000 ) ) ;
#13685 = CARTESIAN_POINT ( 'NONE',  ( 25.17187500061451644, 3.027376345333613106, -5.243569643749998122 ) ) ;
#13686 = CARTESIAN_POINT ( 'NONE',  ( 28.20937500061451786, -4.541064518000417216, -2.621784821875001281 ) ) ;
#13687 = CARTESIAN_POINT ( 'NONE',  ( 22.80000000000000071, 0.000000000000000000, 4.999999999999998224 ) ) ;
#13688 =( BOUNDED_CURVE ( )  B_SPLINE_CURVE ( 2, ( #71304, #71678, #10343, #4082, #65761, #31418, #21052 ),
 .UNSPECIFIED., .F., .T. ) 
 B_SPLINE_CURVE_WITH_KNOTS ( ( 3, 2, 2, 3 ),
 ( 0.2833333333333333814, 0.2861111111111111494, 0.2888888888888889173, 0.2916666666666667407 ),
 .UNSPECIFIED. ) 
 CURVE ( )  GEOMETRIC_REPRESENTATION_ITEM ( )  RATIONAL_B_SPLINE_CURVE ( ( 0.9999999999999973355, 0.8660254037844413721, 1.000000000000000000, 0.8660254037844387076, 1.000000000000000000, 0.8660254037844360431, 1.000000000000002665 ) ) 
 REPRESENTATION_ITEM ( '' )  );
#13689 = CARTESIAN_POINT ( 'NONE',  ( 3.553125000614516082, 4.541064518000418104, -2.621784821874998173 ) ) ;
#13690 = CARTESIAN_POINT ( 'NONE',  ( 21.83437500061451786, -2.746126346562642428, -4.756430356249999214 ) ) ;
#13691 = CARTESIAN_POINT ( 'NONE',  ( 16.92187500061451999, -6.054752690667223547, -1.112240025338166033E-15 ) ) ;
#13692 = CARTESIAN_POINT ( 'NONE',  ( 8.071875000614515017, 4.119189519843966529, 2.378215178124999607 ) ) ;
#13693 = AXIS2_PLACEMENT_3D ( 'NONE', #58463, #44614, #16503 ) ;
#13694 = CARTESIAN_POINT ( 'NONE',  ( 3.140625000614516882, 6.054752690667223547, 3.707466751127219781E-16 ) ) ;
#13695 = CARTESIAN_POINT ( 'NONE',  ( 8.559375000614515727, 4.541064518000418104, -2.621784821874998173 ) ) ;
#13696 = CARTESIAN_POINT ( 'NONE',  ( 17.85937500061451999, -4.541064518000417216, -2.621784821875001281 ) ) ;
#13697 = CARTESIAN_POINT ( 'NONE',  ( -3.179381680195804805, 25.19837022949101168, 27.55859303876839306 ) ) ;
#13698 = CARTESIAN_POINT ( 'NONE',  ( 25.87500000000000000, 4.330127018922191873, 2.499999999999999556 ) ) ;
#13699 = CARTESIAN_POINT ( 'NONE',  ( 27.98437500061451289, 4.541064518000418104, 2.621784821874999949 ) ) ;
#13700 = DIRECTION ( 'NONE',  ( 0.000000000000000000, 0.000000000000000000, 1.000000000000000000 ) ) ;
#13701 = CARTESIAN_POINT ( 'NONE',  ( 5.625000001229036428, 2.886751345948129099, -4.999999999999997335 ) ) ;
#13702 = ORIENTED_EDGE ( 'NONE', *, *, #1440, .T. ) ;
#13703 = CARTESIAN_POINT ( 'NONE',  ( 7.912499999999999645, 2.886751345948126879, 4.999999999999999112 ) ) ;
#13704 = CARTESIAN_POINT ( 'NONE',  ( 12.87187500061451750, 5.824947211148865298E-16, -4.756430356249998326 ) ) ;
#13705 = CARTESIAN_POINT ( 'NONE',  ( 21.17812500061451431, 4.541064518000418104, 2.621784821874999949 ) ) ;
#13706 = CARTESIAN_POINT ( 'NONE',  ( 11.58750000000000036, -2.886751345948129988, 4.999999999999997335 ) ) ;
#13707 = CARTESIAN_POINT ( 'NONE',  ( 8.625000001229034652, -5.773502691896255534, -1.060575238724906372E-15 ) ) ;
#13708 = CARTESIAN_POINT ( 'NONE',  ( 7.265625000614516438, 3.027376345333611329, 5.243569643749999010 ) ) ;
#13709 = CARTESIAN_POINT ( 'NONE',  ( 22.80000000000000071, 0.000000000000000000, 4.999999999999998224 ) ) ;
#13710 = EDGE_CURVE ( 'NONE', #67926, #55851, #17578, .T. ) ;
#13711 = CARTESIAN_POINT ( 'NONE',  ( 21.70312500061451644, 0.000000000000000000, 5.243569643749999010 ) ) ;
#13712 = CARTESIAN_POINT ( 'NONE',  ( 23.62500000000000000, 4.330127018922191873, 2.499999999999999556 ) ) ;
#13713 = CARTESIAN_POINT ( 'NONE',  ( 26.58750000122903145, -4.330127018922194537, 2.499999999999995559 ) ) ;
#13714 = CARTESIAN_POINT ( 'NONE',  ( -0.6941602726958887581, 20.61426555956768780, 33.93677853444431491 ) ) ;
#13715 =( BOUNDED_CURVE ( )  B_SPLINE_CURVE ( 2, ( #42411, #1805, #13222, #35398, #7330, #30227, #13956 ),
 .UNSPECIFIED., .F., .F. ) 
 B_SPLINE_CURVE_WITH_KNOTS ( ( 3, 2, 2, 3 ),
 ( 0.9939432722679919507, 0.9944444444444444642, 0.9972222222222222321, 0.9976655291192481068 ),
 .UNSPECIFIED. ) 
 CURVE ( )  GEOMETRIC_REPRESENTATION_ITEM ( )  RATIONAL_B_SPLINE_CURVE ( ( 0.9603783820186277964, 0.9758280376091080788, 1.000000000000000000, 0.8660254037844387076, 1.000000000000000000, 0.9786189294896985302, 0.9640622897159665250 ) ) 
 REPRESENTATION_ITEM ( '' )  );
#13716 = CARTESIAN_POINT ( 'NONE',  ( 5.062500000000000888, 2.886751345948129099, -4.999999999999998224 ) ) ;
#13717 = VERTEX_POINT ( 'NONE', #11205 ) ;
#13718 = CARTESIAN_POINT ( 'NONE',  ( 19.37812500061451715, 4.541064518000418104, 2.621784821874999949 ) ) ;
#13719 = CARTESIAN_POINT ( 'NONE',  ( 25.71562500061451573, 3.027376345333611329, 5.243569643749999010 ) ) ;
#13720 = CARTESIAN_POINT ( 'NONE',  ( 27.75937500061451502, -4.541064518000417216, -2.621784821875001281 ) ) ;
#13721 = CARTESIAN_POINT ( 'NONE',  ( 10.20000000000000107, 0.000000000000000000, 4.999999999999998224 ) ) ;
#13722 = CARTESIAN_POINT ( 'NONE',  ( 13.75312500061451715, -4.541064518000417216, -2.621784821875001281 ) ) ;
#13723 = CARTESIAN_POINT ( 'NONE',  ( 29.42812500061451431, -4.541064518000419881, 2.621784821874995952 ) ) ;
#13724 = CARTESIAN_POINT ( 'NONE',  ( 8.878125000614515372, 6.421520780324663323E-16, -5.243569643749999010 ) ) ;
#13725 = CARTESIAN_POINT ( 'NONE',  ( -4.243569643749999898, 10.31562500061459353, -32.45002607614398471 ) ) ;
#13726 = CARTESIAN_POINT ( 'NONE',  ( 9.001249775931846008E-16, 12.32187500061451857, 34.90005215228797653 ) ) ;
#13727 = CARTESIAN_POINT ( 'NONE',  ( 25.76250000122903216, -4.330127018922190985, -2.500000000000001332 ) ) ;
#13728 = CARTESIAN_POINT ( 'NONE',  ( 20.03437500061451715, -4.119189519843968306, 2.378215178124996054 ) ) ;
#13729 = CARTESIAN_POINT ( 'NONE',  ( 16.86562500061451786, -6.054752690667223547, -1.112240025338166033E-15 ) ) ;
#13730 = CARTESIAN_POINT ( 'NONE',  ( 4.000000000000000000, 18.38750000000000284, -27.69059892324149885 ) ) ;
#13731 = CARTESIAN_POINT ( 'NONE',  ( 9.384375000614518569, 6.421520780324663323E-16, -5.243569643749999010 ) ) ;
#13732 = CARTESIAN_POINT ( 'NONE',  ( 10.80937500061451928, 4.541064518000418104, -2.621784821874998173 ) ) ;
#13733 = CARTESIAN_POINT ( 'NONE',  ( 17.78437500061451715, -4.541064518000419881, 2.621784821874995952 ) ) ;
#13734 = ORIENTED_EDGE ( 'NONE', *, *, #15386, .T. ) ;
#13735 = CARTESIAN_POINT ( 'NONE',  ( -4.518949595698570576, 8.925733855591197141, 33.96564934234342559 ) ) ;
#13736 = CARTESIAN_POINT ( 'NONE',  ( 22.52812500061451573, 4.541064518000418104, 2.621784821874999949 ) ) ;
#13737 = CARTESIAN_POINT ( 'NONE',  ( 15.38437500061451679, 4.541064518000418104, 2.621784821874999949 ) ) ;
#13738 = CARTESIAN_POINT ( 'NONE',  ( 21.40312500061451573, -4.541064518000417216, -2.621784821875001281 ) ) ;
#13739 = CARTESIAN_POINT ( 'NONE',  ( -3.999999999999999112, 13.70000000000000107, 30.00000000000000000 ) ) ;
#13740 = CARTESIAN_POINT ( 'NONE',  ( 27.77812500061451573, 6.421520780324663323E-16, -5.243569643749999010 ) ) ;
#13741 = CARTESIAN_POINT ( 'NONE',  ( 9.225000001229034297, 2.886751345948129099, -4.999999999999998224 ) ) ;
#13742 = ORIENTED_EDGE ( 'NONE', *, *, #55050, .T. ) ;
#13743 = CARTESIAN_POINT ( 'NONE',  ( 4.350000001229033408, 5.773502691896255534, 3.535250795749688894E-16 ) ) ;
#13744 = CARTESIAN_POINT ( 'NONE',  ( -3.999999999999997335, 18.68750000000000000, -27.69059892324149175 ) ) ;
#13745 = VECTOR ( 'NONE', #71427, 1000.000000000000000 ) ;
#13746 = CARTESIAN_POINT ( 'NONE',  ( 25.91250000122903074, 4.330127018922192761, -2.499999999999997780 ) ) ;
#13747 = CARTESIAN_POINT ( 'NONE',  ( -7.967954043666661671E-16, 13.09062499938548285, 34.33755215474603517 ) ) ;
#13748 = CARTESIAN_POINT ( 'NONE',  ( 6.271875000614517859, 3.027376345333613106, -5.243569643749998122 ) ) ;
#13749 = CARTESIAN_POINT ( 'NONE',  ( 14.76562500061451821, 3.027376345333613106, -5.243569643749998122 ) ) ;
#13750 = CARTESIAN_POINT ( 'NONE',  ( 9.196875000614518569, -3.027376345333614438, 5.243569643749998122 ) ) ;
#13751 = CARTESIAN_POINT ( 'NONE',  ( 27.22500000122903430, 2.886751345948129099, -4.999999999999998224 ) ) ;
#13752 = CARTESIAN_POINT ( 'NONE',  ( 17.93437500061451928, 6.421520780324663323E-16, -5.243569643749999010 ) ) ;
#13753 = CARTESIAN_POINT ( 'NONE',  ( 4.734375000614518214, -4.541064518000419881, 2.621784821874995952 ) ) ;
#13754 = DIRECTION ( 'NONE',  ( 0.000000000000000000, 0.000000000000000000, 1.000000000000000000 ) ) ;
#13755 = CARTESIAN_POINT ( 'NONE',  ( 8.465625000614515727, 3.027376345333613106, -5.243569643749998122 ) ) ;
#13756 = CARTESIAN_POINT ( 'NONE',  ( 16.97812500061451502, 6.421520780324663323E-16, -5.243569643749999010 ) ) ;
#13757 = ORIENTED_EDGE ( 'NONE', *, *, #54130, .F. ) ;
#13758 = CARTESIAN_POINT ( 'NONE',  ( 11.91562500061451857, -6.054752690667223547, -1.112240025338166033E-15 ) ) ;
#13759 = VECTOR ( 'NONE', #44424, 1000.000000000000000 ) ;
#13760 = CARTESIAN_POINT ( 'NONE',  ( 7.687500001229033764, -4.330127018922194537, 2.499999999999995559 ) ) ;
#13761 = CARTESIAN_POINT ( 'NONE',  ( 11.57812500061451644, 6.421520780324663323E-16, -5.243569643749999010 ) ) ;
#13762 = CARTESIAN_POINT ( 'NONE',  ( 20.25937500061451857, 4.119189519843966529, -2.378215178124998275 ) ) ;
#13763 = CARTESIAN_POINT ( 'NONE',  ( 10.83750000000000036, -2.886751345948125991, -5.000000000000000000 ) ) ;
#13764 = CARTESIAN_POINT ( 'NONE',  ( 7.200000001229035718, -2.886751345948129988, 4.999999999999997335 ) ) ;
#13765 = ADVANCED_FACE ( 'NONE', ( #33732 ), #50732, .F. ) ;
#13766 = CARTESIAN_POINT ( 'NONE',  ( 14.40937500061451715, 4.541064518000418104, -2.621784821874998173 ) ) ;
#13767 = CARTESIAN_POINT ( 'NONE',  ( 16.95000000122903216, 5.773502691896255534, 3.535250795749688894E-16 ) ) ;
#13768 = CARTESIAN_POINT ( 'NONE',  ( 23.55000000000000071, 4.330127018922192761, -2.499999999999997780 ) ) ;
#13769 = CARTESIAN_POINT ( 'NONE',  ( 9.001249775931846008E-16, 19.46562500061451573, -25.09994784771203058 ) ) ;
#13770 = DIRECTION ( 'NONE',  ( -1.000000000000000000, -0.000000000000000000, -0.000000000000000000 ) ) ;
#13771 = CARTESIAN_POINT ( 'NONE',  ( -2.000000000000000000, 18.57500000000000284, 26.53589838486224650 ) ) ;
#13772 = DIRECTION ( 'NONE',  ( 0.000000000000000000, -0.7071067811865437980, 0.7071067811865512365 ) ) ;
#13773 = CARTESIAN_POINT ( 'NONE',  ( 45.00000000000000000, 0.000000000000000000, 0.000000000000000000 ) ) ;
#13774 = CARTESIAN_POINT ( 'NONE',  ( 45.00000000000000000, 0.000000000000000000, 0.000000000000000000 ) ) ;
#13775 = CARTESIAN_POINT ( 'NONE',  ( 16.24687500061451573, 6.054752690667223547, 3.707466751127219781E-16 ) ) ;
#13776 = CARTESIAN_POINT ( 'NONE',  ( 28.31250000000000000, -5.773502691896255534, -1.060575238724906372E-15 ) ) ;
#13777 = CARTESIAN_POINT ( 'NONE',  ( 13.90312500061451750, 4.541064518000418104, -2.621784821874998173 ) ) ;
#13778 = CARTESIAN_POINT ( 'NONE',  ( 28.84687500061451360, 0.000000000000000000, 4.756430356249998326 ) ) ;
#13779 = CARTESIAN_POINT ( 'NONE',  ( 24.23437500061451644, 6.421520780324663323E-16, -5.243569643749999010 ) ) ;
#13780 = CARTESIAN_POINT ( 'NONE',  ( 16.39687500061451431, -4.119189519843965641, -2.378215178125001383 ) ) ;
#13781 = CARTESIAN_POINT ( 'NONE',  ( 9.853125000614516793, 4.541064518000418104, -2.621784821874998173 ) ) ;
#13782 = CARTESIAN_POINT ( 'NONE',  ( 14.48437500061451821, 4.541064518000418104, 2.621784821874999949 ) ) ;
#13783 = VERTEX_POINT ( 'NONE', #69173 ) ;
#13784 = CARTESIAN_POINT ( 'NONE',  ( 26.18437500061451573, 4.541064518000418104, 2.621784821874999949 ) ) ;
#13785 = CARTESIAN_POINT ( 'NONE',  ( 28.19062500061451715, -3.027376345333610441, -5.243569643749999898 ) ) ;
#13786 = CARTESIAN_POINT ( 'NONE',  ( 18.85312500061451502, 4.541064518000418104, -2.621784821874998173 ) ) ;
#13787 = CARTESIAN_POINT ( 'NONE',  ( 1.071796769724491893, 13.04509619066137027, -26.00000000000000355 ) ) ;
#13788 = EDGE_CURVE ( 'NONE', #57550, #18233, #1623, .T. ) ;
#13789 = CARTESIAN_POINT ( 'NONE',  ( 4.859696611844813496, 1.176158510076063646, -5.109958294157806336 ) ) ;
#13790 = VECTOR ( 'NONE', #39078, 1000.000000000000000 ) ;
#13791 = CARTESIAN_POINT ( 'NONE',  ( 7.575000000000001954, -4.330127018922194537, 2.499999999999995559 ) ) ;
#13792 = VECTOR ( 'NONE', #55884, 1000.000000000000000 ) ;
#13793 = CARTESIAN_POINT ( 'NONE',  ( 19.20000000122903572, 5.773502691896255534, 3.535250795749688894E-16 ) ) ;
#13794 = CARTESIAN_POINT ( 'NONE',  ( 23.13750000122903216, 6.123233995736764310E-16, -4.999999999999998224 ) ) ;
#13795 = CARTESIAN_POINT ( 'NONE',  ( 9.009375000614516793, 2.746126346562643317, 4.756430356249998326 ) ) ;
#13796 = ORIENTED_EDGE ( 'NONE', *, *, #69469, .F. ) ;
#13797 = CARTESIAN_POINT ( 'NONE',  ( 17.47499999999999787, -4.330127018922194537, 2.499999999999995559 ) ) ;
#13798 = CARTESIAN_POINT ( 'NONE',  ( 18.63749999999999929, 5.773502691896255534, 3.535250795749688894E-16 ) ) ;
#13799 = CARTESIAN_POINT ( 'NONE',  ( 20.10937500061451289, -4.541064518000417216, -2.621784821875001281 ) ) ;
#13800 = CARTESIAN_POINT ( 'NONE',  ( 14.65312500061451573, -4.541064518000417216, -2.621784821875001281 ) ) ;
#13801 = VERTEX_POINT ( 'NONE', #41807 ) ;
#13802 = CARTESIAN_POINT ( 'NONE',  ( -1.999999999999999112, 16.64374999877096784, 26.53589838486224650 ) ) ;
#13803 = CARTESIAN_POINT ( 'NONE',  ( 6.103125000614515905, -4.541064518000417216, -2.621784821875001281 ) ) ;
#13804 = CARTESIAN_POINT ( 'NONE',  ( -3.999999999999999112, 14.03750000000000142, 27.69059892324149530 ) ) ;
#13805 = CARTESIAN_POINT ( 'NONE',  ( 11.84999999999999964, 4.330127018922192761, -2.499999999999997780 ) ) ;
#13806 = CARTESIAN_POINT ( 'NONE',  ( 28.62187500061451217, 5.824947211148865298E-16, -4.756430356249998326 ) ) ;
#13807 = CARTESIAN_POINT ( 'NONE',  ( 2.121784821874999061, 14.70312500061451644, 26.32496088578401583 ) ) ;
#13808 = CARTESIAN_POINT ( 'NONE',  ( 27.32812500061451644, 6.421520780324663323E-16, -5.243569643749999010 ) ) ;
#13809 = CARTESIAN_POINT ( 'NONE',  ( 7.950000000000001954, 0.000000000000000000, 4.999999999999998224 ) ) ;
#13810 = CARTESIAN_POINT ( 'NONE',  ( -1.878215178124999163, 16.39062499938548356, 26.74683588394047007 ) ) ;
#13811 = CARTESIAN_POINT ( 'NONE',  ( 24.79687500061451999, 6.054752690667223547, 3.707466751127219781E-16 ) ) ;
#13812 = ORIENTED_EDGE ( 'NONE', *, *, #12071, .F. ) ;
#13813 = CARTESIAN_POINT ( 'NONE',  ( 20.76562500061451644, 3.027376345333611329, 5.243569643749999010 ) ) ;
#13814 = CARTESIAN_POINT ( 'NONE',  ( 4.243569643749999010, 16.91562500061459318, -32.45002607614398471 ) ) ;
#13815 = CARTESIAN_POINT ( 'NONE',  ( 7.603125000614517681, 4.541064518000418104, -2.621784821874998173 ) ) ;
#13816 = CARTESIAN_POINT ( 'NONE',  ( 26.25937500061451857, 0.000000000000000000, 4.756430356249998326 ) ) ;
#13817 = CARTESIAN_POINT ( 'NONE',  ( 23.65312500061451573, -4.541064518000417216, -2.621784821875001281 ) ) ;
#13818 = CARTESIAN_POINT ( 'NONE',  ( 10.13437500061451679, -4.119189519843968306, 2.378215178124996054 ) ) ;
#13819 = CARTESIAN_POINT ( 'NONE',  ( 1.878215178125000495, 15.86562499938548321, 26.74683588394047007 ) ) ;
#13820 = CARTESIAN_POINT ( 'NONE',  ( 16.39687500061451786, -3.027376345333614438, 5.243569643749998122 ) ) ;
#13821 = CARTESIAN_POINT ( 'NONE',  ( 24.98437500061451644, -4.541064518000419881, 2.621784821874995952 ) ) ;
#13822 = CARTESIAN_POINT ( 'NONE',  ( -2.121784821874999949, 15.28437500061451892, 26.32496088578401938 ) ) ;
#13823 = CARTESIAN_POINT ( 'NONE',  ( 4.903125000614516615, 4.541064518000418104, -2.621784821874998173 ) ) ;
#13824 = CARTESIAN_POINT ( 'NONE',  ( 29.24062500061451431, 6.054752690667223547, 3.707466751127219781E-16 ) ) ;
#13825 = CARTESIAN_POINT ( 'NONE',  ( 2.971875000614517592, -6.054752690667223547, -1.112240025338166033E-15 ) ) ;
#13826 = CARTESIAN_POINT ( 'NONE',  ( 4.275000000000001243, 4.330127018922191873, 2.499999999999999556 ) ) ;
#13827 = CARTESIAN_POINT ( 'NONE',  ( 5.728125000614515905, 6.421520780324663323E-16, -5.243569643749999010 ) ) ;
#13828 = CARTESIAN_POINT ( 'NONE',  ( 8.446875000614518569, -3.027376345333610441, -5.243569643749999898 ) ) ;
#13829 =( NAMED_UNIT ( * ) SI_UNIT ( $, .STERADIAN. ) SOLID_ANGLE_UNIT ( ) );
#13830 = CARTESIAN_POINT ( 'NONE',  ( 17.51250000122903216, 0.000000000000000000, 4.999999999999998224 ) ) ;
#13831 = CARTESIAN_POINT ( 'NONE',  ( 29.39062500061451289, -3.027376345333614438, 5.243569643749998122 ) ) ;
#13832 = CARTESIAN_POINT ( 'NONE',  ( 5.578125000614518214, -4.541064518000419881, 2.621784821874995952 ) ) ;
#13833 = CARTESIAN_POINT ( 'NONE',  ( -3.999999999999999556, 14.88124999877096499, 27.69059892324149175 ) ) ;
#13834 = CARTESIAN_POINT ( 'NONE',  ( 21.43125000122903145, 4.330127018922191873, 2.499999999999999556 ) ) ;
#13835 = CARTESIAN_POINT ( 'NONE',  ( 14.44687500061451679, 6.054752690667223547, 3.707466751127219781E-16 ) ) ;
#13836 = CARTESIAN_POINT ( 'NONE',  ( 3.999999999999999112, 17.63750000122903572, 30.00000000000000000 ) ) ;
#13837 = EDGE_LOOP ( 'NONE', ( #45915, #33207, #62238, #30436, #23367 ) ) ;
#13838 = CARTESIAN_POINT ( 'NONE',  ( 22.19062500061451715, -3.027376345333614438, 5.243569643749998122 ) ) ;
#13839 = CARTESIAN_POINT ( 'NONE',  ( 8.465625000614515727, 3.027376345333613106, -5.243569643749998122 ) ) ;
#13840 = CARTESIAN_POINT ( 'NONE',  ( 23.59687500061451715, -3.027376345333614438, 5.243569643749998122 ) ) ;
#13841 = CARTESIAN_POINT ( 'NONE',  ( 8.540625000614518569, 6.054752690667223547, 3.707466751127219781E-16 ) ) ;
#13842 = CARTESIAN_POINT ( 'NONE',  ( 7.818750001229033408, 2.886751345948129099, -4.999999999999997335 ) ) ;
#13843 = CARTESIAN_POINT ( 'NONE',  ( 10.65000000122903323, 5.773502691896255534, 3.535250795749688894E-16 ) ) ;
#13844 = CARTESIAN_POINT ( 'NONE',  ( 25.11562500061451431, 3.027376345333613106, -5.243569643749998122 ) ) ;
#13845 = CARTESIAN_POINT ( 'NONE',  ( -3.999999999999999112, 19.66250000122903430, -30.00000000000000000 ) ) ;
#13846 = CARTESIAN_POINT ( 'NONE',  ( 10.31250000122903288, 0.000000000000000000, 4.999999999999998224 ) ) ;
#13847 = CARTESIAN_POINT ( 'NONE',  ( 21.32812500061451644, -4.541064518000419881, 2.621784821874995952 ) ) ;
#13848 = CARTESIAN_POINT ( 'NONE',  ( 18.17812500061451786, -4.541064518000419881, 2.621784821874995952 ) ) ;
#13849 = CARTESIAN_POINT ( 'NONE',  ( 5.859375000614519102, 4.541064518000418104, -2.621784821874998173 ) ) ;
#13850 = CARTESIAN_POINT ( 'NONE',  ( 18.26249999999999929, 2.886751345948126879, 4.999999999999999112 ) ) ;
#13851 = CARTESIAN_POINT ( 'NONE',  ( 13.50000000122903288, -2.886751345948129988, 4.999999999999997335 ) ) ;
#13852 = CARTESIAN_POINT ( 'NONE',  ( 11.09062500061451573, -3.027376345333610441, -5.243569643749999898 ) ) ;
#13853 = CARTESIAN_POINT ( 'NONE',  ( 13.37812500061451715, 6.421520780324663323E-16, -5.243569643749999010 ) ) ;
#13854 = EDGE_CURVE ( 'NONE', #4424, #6811, #19252, .T. ) ;
#13855 = CARTESIAN_POINT ( 'NONE',  ( 23.85000000122903430, -2.886751345948129988, 4.999999999999997335 ) ) ;
#13856 = CARTESIAN_POINT ( 'NONE',  ( 21.83437500061451786, -4.541064518000419881, 2.621784821874995952 ) ) ;
#13857 = CARTESIAN_POINT ( 'NONE',  ( 20.67187500061451289, 3.027376345333613106, -5.243569643749998122 ) ) ;
#13858 = CARTESIAN_POINT ( 'NONE',  ( 19.03125000122902932, 6.123233995736764310E-16, -4.999999999999998224 ) ) ;
#13859 = EDGE_CURVE ( 'NONE', #72906, #25370, #17141, .T. ) ;
#13860 = CARTESIAN_POINT ( 'NONE',  ( 7.762500001229033053, -4.330127018922190985, -2.500000000000001332 ) ) ;
#13861 = CARTESIAN_POINT ( 'NONE',  ( 5.409375000614516260, 4.541064518000418104, -2.621784821874998173 ) ) ;
#13862 = CARTESIAN_POINT ( 'NONE',  ( 23.89687500061451786, 6.054752690667223547, 3.707466751127219781E-16 ) ) ;
#13863 = EDGE_CURVE ( 'NONE', #62113, #25000, #29459, .T. ) ;
#13864 = CARTESIAN_POINT ( 'NONE',  ( 4.818692141996693046, -1.334243621178544226, 4.818692141997074074 ) ) ;
#13865 = CARTESIAN_POINT ( 'NONE',  ( 21.47812500061451502, 6.421520780324663323E-16, -5.243569643749999010 ) ) ;
#13866 = CARTESIAN_POINT ( 'NONE',  ( 24.30937500061451573, 4.541064518000418104, -2.621784821874998173 ) ) ;
#13867 = CARTESIAN_POINT ( 'NONE',  ( -3.756430356250000102, 19.72812499938548214, 30.00000000000000000 ) ) ;
#13868 = CARTESIAN_POINT ( 'NONE',  ( 12.37500000122903110, 2.886751345948062486, -5.000000000000113687 ) ) ;
#13869 = DIRECTION ( 'NONE',  ( 1.000000000000000000, 0.000000000000000000, 0.000000000000000000 ) ) ;
#13870 = CARTESIAN_POINT ( 'NONE',  ( 6.496875000614517504, -3.027376345333614438, 5.243569643749998122 ) ) ;
#13871 = CARTESIAN_POINT ( 'NONE',  ( 16.49062500061451786, -3.027376345333610441, -5.243569643749999898 ) ) ;
#13872 = ORIENTED_EDGE ( 'NONE', *, *, #45678, .T. ) ;
#13873 = CARTESIAN_POINT ( 'NONE',  ( 11.55000000000000071, 0.000000000000000000, 4.999999999999998224 ) ) ;
#13874 = CARTESIAN_POINT ( 'NONE',  ( 25.00312500061451715, -4.541064518000417216, -2.621784821875001281 ) ) ;
#13875 = CARTESIAN_POINT ( 'NONE',  ( 2.859375000614519546, 0.000000000000000000, 5.243569643749999010 ) ) ;
#13876 = CARTESIAN_POINT ( 'NONE',  ( 45.00000000000000000, 6.123233995736764310E-16, -4.999999999999998224 ) ) ;
#13877 = CARTESIAN_POINT ( 'NONE',  ( 3.662307474140069186, 3.404096216171143219, -3.815575040102499482 ) ) ;
#13878 = CARTESIAN_POINT ( 'NONE',  ( 15.63749999999999751, -2.886751345948129988, 4.999999999999997335 ) ) ;
#13879 = CARTESIAN_POINT ( 'NONE',  ( 21.81562500061451004, -6.054752690667223547, -1.112240025338166033E-15 ) ) ;
#13880 = ORIENTED_EDGE ( 'NONE', *, *, #71305, .T. ) ;
#13881 = CARTESIAN_POINT ( 'NONE',  ( 25.27499999999999858, 6.123233995736764310E-16, -4.999999999999998224 ) ) ;
#13882 = CARTESIAN_POINT ( 'NONE',  ( 25.77187500061451075, 3.027376345333611329, 5.243569643749999010 ) ) ;
#13883 = VERTEX_POINT ( 'NONE', #60160 ) ;
#13884 = CARTESIAN_POINT ( 'NONE',  ( 25.80000000000000071, 4.330127018922192761, -2.499999999999997780 ) ) ;
#13885 = CARTESIAN_POINT ( 'NONE',  ( 12.66562500061451502, 3.027376345333611329, 5.243569643749999010 ) ) ;
#13886 = CARTESIAN_POINT ( 'NONE',  ( 2.878125000614517592, -4.541064518000419881, 2.621784821874995952 ) ) ;
#13887 = CARTESIAN_POINT ( 'NONE',  ( 15.72187500061451537, 4.119189519843966529, 2.378215178124999607 ) ) ;
#13888 = CARTESIAN_POINT ( 'NONE',  ( 29.69062500061451715, 6.054752690667223547, 3.707466751127219781E-16 ) ) ;
#13889 = CARTESIAN_POINT ( 'NONE',  ( 12.22500000122903430, -5.773502691896255534, -1.060575238724906372E-15 ) ) ;
#13890 = CARTESIAN_POINT ( 'NONE',  ( 20.47500000000000142, 4.330127018922191873, 2.499999999999999556 ) ) ;
#13891 = CARTESIAN_POINT ( 'NONE',  ( 26.58750000000000213, -2.886751345948125991, -5.000000000000000000 ) ) ;
#13892 = CARTESIAN_POINT ( 'NONE',  ( 3.999999999999998668, 14.20624999877096606, 32.30940107675850470 ) ) ;
#13893 = CARTESIAN_POINT ( 'NONE',  ( 6.046875000614519102, -3.027376345333614438, 5.243569643749998122 ) ) ;
#13894 = CARTESIAN_POINT ( 'NONE',  ( 18.30937500061451928, -4.541064518000417216, -2.621784821875001281 ) ) ;
#13895 = CARTESIAN_POINT ( 'NONE',  ( 1.071796769724476572, 11.24509619066136779, 34.00000000000000000 ) ) ;
#13896 = ORIENTED_EDGE ( 'NONE', *, *, #25145, .T. ) ;
#13897 = CARTESIAN_POINT ( 'NONE',  ( 29.09062500061451573, -3.027376345333610441, -5.243569643749999898 ) ) ;
#13898 = CARTESIAN_POINT ( 'NONE',  ( 29.29687500061451644, 6.054752690667223547, 3.707466751127219781E-16 ) ) ;
#13900 = EDGE_CURVE ( 'NONE', #37056, #29389, #52540, .T. ) ;
#13899 = CARTESIAN_POINT ( 'NONE',  ( 5.296875000614518214, -3.027376345333610441, -5.243569643749999898 ) ) ;
#13901 = CARTESIAN_POINT ( 'NONE',  ( 16.91250000000000142, 2.886751345948126879, 4.999999999999999112 ) ) ;
#13902 = CARTESIAN_POINT ( 'NONE',  ( 12.74062500061451786, -3.027376345333614438, 5.243569643749998122 ) ) ;
#13903 = CYLINDRICAL_SURFACE ( 'NONE', #9827, 4.000000000000000000 ) ;
#13904 = CARTESIAN_POINT ( 'NONE',  ( 4.898587196589411843E-16, 20.00000000000000000, 33.99999999999999289 ) ) ;
#13905 = CARTESIAN_POINT ( 'NONE',  ( 8.231250001229033941, 6.123233995736764310E-16, -4.999999999999998224 ) ) ;
#13906 = CARTESIAN_POINT ( 'NONE',  ( 17.77500000122903145, 2.886751345948129099, -4.999999999999998224 ) ) ;
#13907 = CARTESIAN_POINT ( 'NONE',  ( -1.071796769724492115, 19.51115380933863008, 34.00000000000000000 ) ) ;
#13908 = CARTESIAN_POINT ( 'NONE',  ( 17.33437500061451431, -4.119189519843968306, 2.378215178124996054 ) ) ;
#13909 = CARTESIAN_POINT ( 'NONE',  ( 7.265625000614516438, 3.027376345333611329, 5.243569643749999010 ) ) ;
#13910 = CARTESIAN_POINT ( 'NONE',  ( 23.70937500061451786, -4.541064518000417216, -2.621784821875001281 ) ) ;
#13911 = CARTESIAN_POINT ( 'NONE',  ( -2.121784821874999949, 18.88437500061451857, 26.32496088578401938 ) ) ;
#13912 = CARTESIAN_POINT ( 'NONE',  ( 25.13437500061451502, 6.421520780324663323E-16, -5.243569643749999010 ) ) ;
#13913 = CARTESIAN_POINT ( 'NONE',  ( 5.250000000000000888, 0.000000000000000000, 4.999999999999998224 ) ) ;
#13914 = CARTESIAN_POINT ( 'NONE',  ( -3.999999999999999112, 11.56250000122903465, 30.00000000000000000 ) ) ;
#13915 = CARTESIAN_POINT ( 'NONE',  ( 14.46562500061451750, 3.027376345333611329, 5.243569643749999010 ) ) ;
#13917 =( BOUNDED_CURVE ( )  B_SPLINE_CURVE ( 2, ( #29680, #52216, #900, #11252, #40779, #51855, #1619 ),
 .UNSPECIFIED., .F., .F. ) 
 B_SPLINE_CURVE_WITH_KNOTS ( ( 3, 2, 2, 3 ),
 ( 0.9857515426466298969, 0.9861111111111111605, 0.9888888888888889284, 0.9891869394448051800 ),
 .UNSPECIFIED. ) 
 CURVE ( )  GEOMETRIC_REPRESENTATION_ITEM ( )  RATIONAL_B_SPLINE_CURVE ( ( 0.9698051456607861276, 0.9826577056573390090, 1.000000000000000000, 0.8660254037844387076, 1.000000000000000000, 0.9856247669629467634, 0.9743344071885395863 ) ) 
 REPRESENTATION_ITEM ( '' )  );
#13916 = CARTESIAN_POINT ( 'NONE',  ( 4.200000001229033053, -2.886751345948125991, -5.000000000000000000 ) ) ;
#13918 = CARTESIAN_POINT ( 'NONE',  ( 9.984375000614518214, 4.541064518000418104, 2.621784821874999949 ) ) ;
#13919 = CARTESIAN_POINT ( 'NONE',  ( 1.071796769724484344, 14.84509619066137098, 34.00000000000000000 ) ) ;
#13920 = ORIENTED_EDGE ( 'NONE', *, *, #21683, .T. ) ;
#13921 = CARTESIAN_POINT ( 'NONE',  ( 13.41562500061451502, 3.027376345333613106, -5.243569643749998122 ) ) ;
#13922 = CARTESIAN_POINT ( 'NONE',  ( 3.445179128855461848, -3.623644852411430417, -3.790023247856260102 ) ) ;
#13923 = CARTESIAN_POINT ( 'NONE',  ( 23.17500000122903359, 2.886751345948129099, -4.999999999999998224 ) ) ;
#13924 = CARTESIAN_POINT ( 'NONE',  ( 11.07187500061451679, -6.054752690667223547, -1.112240025338166033E-15 ) ) ;
#13925 = CARTESIAN_POINT ( 'NONE',  ( 13.34062500061451750, -3.027376345333610441, -5.243569643749999898 ) ) ;
#13926 = CARTESIAN_POINT ( 'NONE',  ( 29.19375000122903074, -2.886751345948129988, 4.999999999999997335 ) ) ;
#13927 = CARTESIAN_POINT ( 'NONE',  ( 24.34687500061451715, 6.054752690667223547, 3.707466751127219781E-16 ) ) ;
#13928 = CARTESIAN_POINT ( 'NONE',  ( 65.00000000000000000, 0.000000000000000000, 0.000000000000000000 ) ) ;
#13929 = CARTESIAN_POINT ( 'NONE',  ( 30.00000000000000000, 0.000000000000000000, 0.000000000000000000 ) ) ;
#13930 = DIRECTION ( 'NONE',  ( 0.000000000000000000, 0.000000000000000000, 1.000000000000000000 ) ) ;
#13931 = CARTESIAN_POINT ( 'NONE',  ( 4.243569643749999898, 13.74687500061451750, -27.54997392385601529 ) ) ;
#13932 = CARTESIAN_POINT ( 'NONE',  ( 16.88437500061451502, -4.541064518000419881, 2.621784821874995952 ) ) ;
#13933 = CARTESIAN_POINT ( 'NONE',  ( 16.76250000122903216, -4.330127018922190985, -2.500000000000001332 ) ) ;
#13934 = CARTESIAN_POINT ( 'NONE',  ( 11.78437500061451892, 4.541064518000418104, 2.621784821874999949 ) ) ;
#13935 = CARTESIAN_POINT ( 'NONE',  ( -2.121784821874999949, 18.82812500061451644, -33.67503911421598417 ) ) ;
#13936 = CARTESIAN_POINT ( 'NONE',  ( 19.65000000122902790, 5.773502691896255534, 3.535250795749688894E-16 ) ) ;
#13937 = CARTESIAN_POINT ( 'NONE',  ( 13.49062500061451608, 6.054752690667223547, 3.707466751127219781E-16 ) ) ;
#13938 = VERTEX_POINT ( 'NONE', #53256 ) ;
#13939 = ORIENTED_EDGE ( 'NONE', *, *, #5583, .T. ) ;
#13940 = CARTESIAN_POINT ( 'NONE',  ( 14.58750000000000036, 5.773502691896255534, 3.535250795749688894E-16 ) ) ;
#13941 = CARTESIAN_POINT ( 'NONE',  ( 18.00000000000000355, -4.330127018922190985, -2.500000000000001332 ) ) ;
#13942 = CARTESIAN_POINT ( 'NONE',  ( 13.17187500061451821, 3.027376345333611329, 5.243569643749999010 ) ) ;
#13943 = CARTESIAN_POINT ( 'NONE',  ( 12.82500000122903394, 2.886751345948129099, -4.999999999999998224 ) ) ;
#13944 = CARTESIAN_POINT ( 'NONE',  ( 19.98750000122903359, 6.123233995736764310E-16, -4.999999999999998224 ) ) ;
#13945 = CARTESIAN_POINT ( 'NONE',  ( 17.12812500061451715, 4.541064518000418104, 2.621784821874999949 ) ) ;
#13946 = CARTESIAN_POINT ( 'NONE',  ( 19.79062500061451502, 6.054752690667223547, 3.707466751127219781E-16 ) ) ;
#13947 = CARTESIAN_POINT ( 'NONE',  ( 27.75000000122903288, 5.773502691896255534, 3.535250795749688894E-16 ) ) ;
#13948 = CARTESIAN_POINT ( 'NONE',  ( 25.31250000000000000, 2.886751345948129099, -4.999999999999998224 ) ) ;
#13949 = CARTESIAN_POINT ( 'NONE',  ( 7.359375000614516438, 0.000000000000000000, 4.756430356249998326 ) ) ;
#13950 = CARTESIAN_POINT ( 'NONE',  ( 29.55000000000000071, 0.000000000000000000, 4.999999999999998224 ) ) ;
#13951 = CARTESIAN_POINT ( 'NONE',  ( 28.80937500061451573, 4.541064518000418104, -2.621784821874998173 ) ) ;
#13952 = CARTESIAN_POINT ( 'NONE',  ( -2.121784821874996840, 14.08437500061451786, -26.32496088578401583 ) ) ;
#13953 = CARTESIAN_POINT ( 'NONE',  ( 3.562500001229033764, 0.000000000000000000, 4.999999999999998224 ) ) ;
#13954 = CARTESIAN_POINT ( 'NONE',  ( 4.800000000000002487, 0.000000000000000000, 4.999999999999998224 ) ) ;
#13955 = EDGE_CURVE ( 'NONE', #11866, #20886, #32695, .T. ) ;
#13956 = CARTESIAN_POINT ( 'NONE',  ( 2.923357432354301455, -4.056350739605543154, 3.322806236625610588 ) ) ;
#13957 = CARTESIAN_POINT ( 'NONE',  ( 7.696875000614516793, 6.054752690667223547, 3.707466751127219781E-16 ) ) ;
#13958 = CARTESIAN_POINT ( 'NONE',  ( 29.09062500061451573, -3.027376345333610441, -5.243569643749999898 ) ) ;
#13959 = CARTESIAN_POINT ( 'NONE',  ( 3.242103837493086330E-14, 13.13749999999999929, -34.00000000000000000 ) ) ;
#13960 = CARTESIAN_POINT ( 'NONE',  ( -5.810221930991193690E-16, 18.98750000000000071, -34.00000000000000000 ) ) ;
#13961 = CARTESIAN_POINT ( 'NONE',  ( 16.87500000122902932, 2.886751345948095793, -5.000000000000055067 ) ) ;
#13962 = CARTESIAN_POINT ( 'NONE',  ( 6.196875000614515905, -3.027376345333610441, -5.243569643749999898 ) ) ;
#13963 = CARTESIAN_POINT ( 'NONE',  ( 10.47187500061451715, 3.027376345333611329, 5.243569643749999010 ) ) ;
#13964 = CARTESIAN_POINT ( 'NONE',  ( 4.387500000000002842, -2.886751345948129988, 4.999999999999997335 ) ) ;
#13965 = CARTESIAN_POINT ( 'NONE',  ( 9.001249775931846008E-16, 14.51562500061459460, 34.90005215228797653 ) ) ;
#13966 = CARTESIAN_POINT ( 'NONE',  ( 3.795044958738071461, 25.05366892013418934, 31.29105878821236786 ) ) ;
#13967 = CARTESIAN_POINT ( 'NONE',  ( 7.162500000000001421, -5.773502691896255534, -1.060575238724906372E-15 ) ) ;
#13968 = CARTESIAN_POINT ( 'NONE',  ( 15.90937500061451360, -5.492252693125287522, -1.008910452111647106E-15 ) ) ;
#13969 = CARTESIAN_POINT ( 'NONE',  ( 20.54062500061451502, -3.027376345333610441, -5.243569643749999898 ) ) ;
#13970 = CARTESIAN_POINT ( 'NONE',  ( 12.10312500061451857, 4.541064518000418104, -2.621784821874998173 ) ) ;
#13971 = CARTESIAN_POINT ( 'NONE',  ( 22.99687500061451573, 0.000000000000000000, 4.756430356249998326 ) ) ;
#13972 = CARTESIAN_POINT ( 'NONE',  ( 9.871875000614517504, 3.027376345333613106, -5.243569643749998122 ) ) ;
#13973 = CARTESIAN_POINT ( 'NONE',  ( 27.37500000000000000, -4.330127018922194537, 2.499999999999995559 ) ) ;
#13974 = CARTESIAN_POINT ( 'NONE',  ( 23.02500000122903145, -5.773502691896255534, -1.060575238724906372E-15 ) ) ;
#13975 = DIRECTION ( 'NONE',  ( -1.000000000000000000, -0.000000000000000000, -0.000000000000000000 ) ) ;
#13976 = CARTESIAN_POINT ( 'NONE',  ( 10.43437500061451750, 4.541064518000418104, 2.621784821874999949 ) ) ;
#13977 = CARTESIAN_POINT ( 'NONE',  ( 26.97187500061451360, 3.027376345333613106, -5.243569643749998122 ) ) ;
#13978 = CARTESIAN_POINT ( 'NONE',  ( 1.999999999999998668, 18.16250000122903074, -33.46410161513775705 ) ) ;
#13979 = CARTESIAN_POINT ( 'NONE',  ( 11.77500000000000036, 6.123233995736764310E-16, -4.999999999999998224 ) ) ;
#13980 = CARTESIAN_POINT ( 'NONE',  ( 20.78437500061451715, 4.541064518000418104, 2.621784821874999949 ) ) ;
#13981 = CARTESIAN_POINT ( 'NONE',  ( 12.79687500061451821, -3.027376345333614438, 5.243569643749998122 ) ) ;
#13982 = CARTESIAN_POINT ( 'NONE',  ( -3.756430356250001434, 12.90312499938548463, 32.16877607737301048 ) ) ;
#13983 = CARTESIAN_POINT ( 'NONE',  ( 23.13749999999999929, 5.773502691896255534, 3.535250795749688894E-16 ) ) ;
#13984 = CARTESIAN_POINT ( 'NONE',  ( 1.999999999999997335, 14.22499999999999964, 33.46410161513775705 ) ) ;
#13985 = CARTESIAN_POINT ( 'NONE',  ( 2.121784821874999061, 12.50937500061451857, -33.67503911421598417 ) ) ;
#13986 = CARTESIAN_POINT ( 'NONE',  ( 23.85937500061451644, 4.119189519843966529, -2.378215178124998275 ) ) ;
#13987 = CARTESIAN_POINT ( 'NONE',  ( 15.06562500061451537, -6.054752690667223547, -1.112240025338166033E-15 ) ) ;
#13988 = CARTESIAN_POINT ( 'NONE',  ( 3.675000000000001155, 6.123233995736764310E-16, -4.999999999999998224 ) ) ;
#13989 = DIRECTION ( 'NONE',  ( -1.000000000000000000, -0.000000000000000000, -0.000000000000000000 ) ) ;
#13990 = CARTESIAN_POINT ( 'NONE',  ( 22.12500000000000000, 6.123233995736764310E-16, -4.999999999999998224 ) ) ;
#13991 = CARTESIAN_POINT ( 'NONE',  ( 13.35000000000000142, 0.000000000000000000, 4.999999999999998224 ) ) ;
#13992 = CARTESIAN_POINT ( 'NONE',  ( 3.999999999999998668, 18.57500000122903216, 27.69059892324149175 ) ) ;
#13993 = CARTESIAN_POINT ( 'NONE',  ( 13.27500000122903323, 2.886751345948129099, -4.999999999999998224 ) ) ;
#13994 = CARTESIAN_POINT ( 'NONE',  ( 25.02187500061451431, -6.054752690667223547, -1.112240025338166033E-15 ) ) ;
#13995 = CARTESIAN_POINT ( 'NONE',  ( 16.02187500061451786, -6.054752690667223547, -1.112240025338166033E-15 ) ) ;
#13996 = CARTESIAN_POINT ( 'NONE',  ( 25.25625000122903074, -4.330127018922190985, -2.500000000000001332 ) ) ;
#13997 = EDGE_LOOP ( 'NONE', ( #18737, #39216, #63461, #1004 ) ) ;
#13998 = CARTESIAN_POINT ( 'NONE',  ( 19.67812500061451786, 6.421520780324663323E-16, -5.243569643749999010 ) ) ;
#13999 = CARTESIAN_POINT ( 'NONE',  ( 4.828125000614518214, 6.421520780324663323E-16, -5.243569643749999010 ) ) ;
#14000 = CARTESIAN_POINT ( 'NONE',  ( 18.19687500061451502, -3.027376345333614438, 5.243569643749998122 ) ) ;
#14001 = CARTESIAN_POINT ( 'NONE',  ( 29.63437500061451502, 6.421520780324663323E-16, -5.243569643749999010 ) ) ;
#14002 = CARTESIAN_POINT ( 'NONE',  ( 5.053125000614517859, 0.000000000000000000, 5.243569643749999010 ) ) ;
#14003 = CARTESIAN_POINT ( 'NONE',  ( 21.32812500061451644, -4.541064518000419881, 2.621784821874995952 ) ) ;
#14004 = EDGE_CURVE ( 'NONE', #6203, #20497, #24684, .T. ) ;
#14005 = CARTESIAN_POINT ( 'NONE',  ( -2.121784821874996840, 14.92812500061451608, 33.67503911421598417 ) ) ;
#14006 = CARTESIAN_POINT ( 'NONE',  ( 15.52500000122903323, 2.886751345948129099, -4.999999999999998224 ) ) ;
#14007 = CARTESIAN_POINT ( 'NONE',  ( 12.68437500061451573, 4.119189519843966529, 2.378215178124999607 ) ) ;
#14008 = CARTESIAN_POINT ( 'NONE',  ( 7.565625000614518036, 3.027376345333612662, -5.243569643749998122 ) ) ;
#14009 = CARTESIAN_POINT ( 'NONE',  ( 3.946875000614517681, -3.027376345333610441, -5.243569643749999898 ) ) ;
#14010 = CARTESIAN_POINT ( 'NONE',  ( 28.60312500061451502, -4.541064518000417216, -2.621784821875001281 ) ) ;
#14011 = CARTESIAN_POINT ( 'NONE',  ( 22.77187500061451786, -6.054752690667223547, -1.112240025338166033E-15 ) ) ;
#14012 = CARTESIAN_POINT ( 'NONE',  ( 14.42812500061451786, 4.541064518000418104, 2.621784821874999949 ) ) ;
#14013 = CARTESIAN_POINT ( 'NONE',  ( 24.67500000122903359, 2.886751345948126879, 4.999999999999999112 ) ) ;
#14014 = CARTESIAN_POINT ( 'NONE',  ( 24.29062500061451502, 6.054752690667223547, 3.707466751127219781E-16 ) ) ;
#14015 = CARTESIAN_POINT ( 'NONE',  ( 20.29687500061451644, 6.054752690667223547, 3.707466751127219781E-16 ) ) ;
#14016 = CARTESIAN_POINT ( 'NONE',  ( 15.77812500061451573, 4.541064518000418104, 2.621784821874999949 ) ) ;
#14017 = CARTESIAN_POINT ( 'NONE',  ( 4.243569643749999898, 13.74687500061451750, 32.45002607614398471 ) ) ;
#14018 = CARTESIAN_POINT ( 'NONE',  ( 19.79062500061451502, 6.054752690667223547, 3.707466751127219781E-16 ) ) ;
#14019 = CARTESIAN_POINT ( 'NONE',  ( 29.01562500061451644, -6.054752690667223547, -1.112240025338166033E-15 ) ) ;
#14020 = ORIENTED_EDGE ( 'NONE', *, *, #68767, .F. ) ;
#14021 = CARTESIAN_POINT ( 'NONE',  ( 22.64999999999999858, 4.330127018922192761, -2.499999999999997780 ) ) ;
#14022 = CARTESIAN_POINT ( 'NONE',  ( -3.999999999999999556, 10.06250000000000178, -32.30940107675850470 ) ) ;
#14023 = CARTESIAN_POINT ( 'NONE',  ( 16.05000000000000071, 0.000000000000000000, 4.999999999999998224 ) ) ;
#14024 = CARTESIAN_POINT ( 'NONE',  ( 26.35312500061451857, -4.541064518000417216, -2.621784821875001281 ) ) ;
#14025 = CARTESIAN_POINT ( 'NONE',  ( 7.940625000614518036, -3.027376345333610441, -5.243569643749999898 ) ) ;
#14026 = CARTESIAN_POINT ( 'NONE',  ( 19.83750000122903145, -4.330127018922194537, 2.499999999999995559 ) ) ;
#14027 = CARTESIAN_POINT ( 'NONE',  ( 23.65312500061451573, -4.541064518000417216, -2.621784821875001281 ) ) ;
#14028 = CARTESIAN_POINT ( 'NONE',  ( 25.80000000000000071, 4.330127018922192761, -2.499999999999997780 ) ) ;
#14029 = CARTESIAN_POINT ( 'NONE',  ( 28.82812500061451644, 4.541064518000418104, 2.621784821874999949 ) ) ;
#14030 = CARTESIAN_POINT ( 'NONE',  ( 9.103125000614515017, 0.000000000000000000, 5.243569643749999010 ) ) ;
#14031 = ORIENTED_EDGE ( 'NONE', *, *, #71606, .F. ) ;
#14032 = CARTESIAN_POINT ( 'NONE',  ( 26.87812500061451360, 6.421520780324663323E-16, -5.243569643749999010 ) ) ;
#14033 = CARTESIAN_POINT ( 'NONE',  ( 5.315625000614516260, 3.027376345333613106, -5.243569643749998122 ) ) ;
#14034 = CARTESIAN_POINT ( 'NONE',  ( 14.14687500061451786, -2.746126346562646425, 4.756430356249996549 ) ) ;
#14035 = CARTESIAN_POINT ( 'NONE',  ( 3.328125000614516438, -4.541064518000419881, 2.621784821874995952 ) ) ;
#14036 = DIRECTION ( 'NONE',  ( 1.000000000000000000, 0.000000000000000000, -0.000000000000000000 ) ) ;
#14037 = CARTESIAN_POINT ( 'NONE',  ( 13.04999999999999893, -4.330127018922190985, -2.500000000000001332 ) ) ;
#14038 = EDGE_CURVE ( 'NONE', #40656, #17484, #4410, .T. ) ;
#14039 = CARTESIAN_POINT ( 'NONE',  ( 12.94687500061451857, -3.027376345333610441, -5.243569643749999898 ) ) ;
#14040 = CARTESIAN_POINT ( 'NONE',  ( 9.225000001229034297, 2.886751345948129099, -4.999999999999998224 ) ) ;
#14041 = CARTESIAN_POINT ( 'NONE',  ( 16.20937500061451786, 4.541064518000418104, -2.621784821874998173 ) ) ;
#14042 = CARTESIAN_POINT ( 'NONE',  ( 15.97499999999999964, 4.330127018922191873, 2.499999999999999556 ) ) ;
#14043 = CARTESIAN_POINT ( 'NONE',  ( 8.596875000614518925, 6.054752690667223547, 3.707466751127219781E-16 ) ) ;
#14044 = CARTESIAN_POINT ( 'NONE',  ( -3.000416591977282496E-16, 11.14062500061451644, -34.90005215228797653 ) ) ;
#14045 = CARTESIAN_POINT ( 'NONE',  ( 24.75000000000000000, -4.330127018922190985, -2.500000000000001332 ) ) ;
#14046 = CARTESIAN_POINT ( 'NONE',  ( 23.44687500061451502, 0.000000000000000000, 4.756430356249998326 ) ) ;
#14047 = CARTESIAN_POINT ( 'NONE',  ( 26.21250000000000213, 2.886751345948157077, -4.999999999999949374 ) ) ;
#14048 = CARTESIAN_POINT ( 'NONE',  ( 22.11562500061451786, 3.027376345333611329, 5.243569643749999010 ) ) ;
#14049 = CARTESIAN_POINT ( 'NONE',  ( -4.243569643749999898, 9.959375000614517859, 30.00000000000000000 ) ) ;
#14050 = CARTESIAN_POINT ( 'NONE',  ( 26.74687500061451573, -3.027376345333614438, 5.243569643749998122 ) ) ;
#14051 =( BOUNDED_CURVE ( )  B_SPLINE_CURVE ( 2, ( #31574, #54113, #7575, #7940, #19367, #30478, #47465 ),
 .UNSPECIFIED., .F., .F. ) 
 B_SPLINE_CURVE_WITH_KNOTS ( ( 3, 2, 2, 3 ),
 ( 0.3500000000000000333, 0.3527777777777778567, 0.3555555555555556246, 0.3583333333333333925 ),
 .UNSPECIFIED. ) 
 CURVE ( )  GEOMETRIC_REPRESENTATION_ITEM ( )  RATIONAL_B_SPLINE_CURVE ( ( 0.9999999999999973355, 0.8660254037844413721, 1.000000000000000000, 0.8660254037844387076, 1.000000000000000000, 0.8660254037844360431, 1.000000000000002665 ) ) 
 REPRESENTATION_ITEM ( '' )  );
#14052 = CARTESIAN_POINT ( 'NONE',  ( 28.35937500061451289, 4.541064518000418104, -2.621784821874998173 ) ) ;
#14053 = CARTESIAN_POINT ( 'NONE',  ( 3.440625000614518036, -3.027376345333610441, -5.243569643749999898 ) ) ;
#14054 = B_SPLINE_CURVE_WITH_KNOTS ( 'NONE', 3,
 ( #46025, #68919, #969, #6861, #67837, #57810, #51205, #5777, #17210, #40850 ),
 .UNSPECIFIED., .F., .F.,
 ( 4, 3, 3, 4 ),
 ( 4.336808689942017736E-19, 8.679785101976316634E-05, 0.0002172003593263750992, 0.0003478061572614656602 ),
 .UNSPECIFIED. ) ;
#14055 = CARTESIAN_POINT ( 'NONE',  ( 21.30937500061451217, -5.492252693125287522, -1.008910452111647106E-15 ) ) ;
#14056 = CARTESIAN_POINT ( 'NONE',  ( 15.94687500061451502, -3.027376345333614438, 5.243569643749998122 ) ) ;
#14057 = CARTESIAN_POINT ( 'NONE',  ( 9.796875000614514661, 4.119189519843966529, -2.378215178124998275 ) ) ;
#14058 = CARTESIAN_POINT ( 'NONE',  ( 28.76250000122903216, 0.000000000000000000, 4.999999999999998224 ) ) ;
#14059 = CARTESIAN_POINT ( 'NONE',  ( 6.871875000614517504, 3.027376345333611329, 5.243569643749999010 ) ) ;
#14060 = CARTESIAN_POINT ( 'NONE',  ( 17.63437500061451502, 4.541064518000418104, 2.621784821874999949 ) ) ;
#14061 = CARTESIAN_POINT ( 'NONE',  ( 0.000000000000000000, 25.54316770519903557, 26.00000000000000000 ) ) ;
#14062 = CARTESIAN_POINT ( 'NONE',  ( 25.64999999999999858, -4.330127018922190985, -2.500000000000001332 ) ) ;
#14063 = CARTESIAN_POINT ( 'NONE',  ( 27.30937500061451573, -4.541064518000417216, -2.621784821875001281 ) ) ;
#14064 = CARTESIAN_POINT ( 'NONE',  ( 3.756430356249998770, 13.16562499938548392, 32.16877607737302469 ) ) ;
#14065 = CARTESIAN_POINT ( 'NONE',  ( 29.55000000000000071, 0.000000000000000000, 4.999999999999998224 ) ) ;
#14066 = EDGE_LOOP ( 'NONE', ( #71595, #38453, #53600, #54566 ) ) ;
#14067 = CARTESIAN_POINT ( 'NONE',  ( 7.950000000000001954, 0.000000000000000000, 4.999999999999998224 ) ) ;
#14068 = CARTESIAN_POINT ( 'NONE',  ( 8.259375000614515017, -5.492252693125287522, -1.008910452111647106E-15 ) ) ;
#14069 = CARTESIAN_POINT ( 'NONE',  ( 22.52812500061451573, 4.541064518000418104, 2.621784821874999949 ) ) ;
#14070 = CARTESIAN_POINT ( 'NONE',  ( 12.48750000000000249, -2.886751345948129988, 4.999999999999997335 ) ) ;
#14071 = CARTESIAN_POINT ( 'NONE',  ( 7.612500001229035362, 0.000000000000000000, 4.999999999999998224 ) ) ;
#14072 = CARTESIAN_POINT ( 'NONE',  ( 7.303125000614516082, 0.000000000000000000, 5.243569643749999010 ) ) ;
#14073 = CARTESIAN_POINT ( 'NONE',  ( 22.23750000000000071, 5.773502691896255534, 3.535250795749688894E-16 ) ) ;
#14074 = CARTESIAN_POINT ( 'NONE',  ( 18.89062500061451644, 6.054752690667223547, 3.707466751127219781E-16 ) ) ;
#14075 = CARTESIAN_POINT ( 'NONE',  ( 4.133006999854208274, -2.814071958334764201, 4.297262197382941906 ) ) ;
#14076 = CARTESIAN_POINT ( 'NONE',  ( 26.21250000122903501, -4.330127018922190985, -2.500000000000001332 ) ) ;
#14077 = CARTESIAN_POINT ( 'NONE',  ( 5.662500000000000533, 2.886751345948126879, 4.999999999999999112 ) ) ;
#14078 = VERTEX_POINT ( 'NONE', #44666 ) ;
#14079 = CARTESIAN_POINT ( 'NONE',  ( 19.07812500061451644, -4.541064518000419881, 2.621784821874995952 ) ) ;
#14080 = CARTESIAN_POINT ( 'NONE',  ( 26.61562500061451786, 3.027376345333611329, 5.243569643749999010 ) ) ;
#14081 = CARTESIAN_POINT ( 'NONE',  ( 25.09687500061451715, -3.027376345333610441, -5.243569643749999898 ) ) ;
#14082 = CARTESIAN_POINT ( 'NONE',  ( 8.737500000000002487, 5.773502691896255534, 3.535250795749688894E-16 ) ) ;
#14083 = CARTESIAN_POINT ( 'NONE',  ( 10.75312500061451715, 4.541064518000418104, -2.621784821874998173 ) ) ;
#14084 = CARTESIAN_POINT ( 'NONE',  ( 28.30312500061451431, 4.541064518000418104, -2.621784821874998173 ) ) ;
#14085 = CARTESIAN_POINT ( 'NONE',  ( 8.090625000614515727, 6.054752690667223547, 3.707466751127219781E-16 ) ) ;
#14086 = CARTESIAN_POINT ( 'NONE',  ( 3.053854506608032704, -3.959065788097787753, 3.087202309779018883 ) ) ;
#14087 = CARTESIAN_POINT ( 'NONE',  ( 2.121784821875001281, 11.90937500061451892, 33.67503911421598417 ) ) ;
#14088 = CARTESIAN_POINT ( 'NONE',  ( 24.52500000122903145, 2.886751345948129099, -4.999999999999998224 ) ) ;
#14089 = CARTESIAN_POINT ( 'NONE',  ( 19.20937500061451786, -4.119189519843965641, -2.378215178125001383 ) ) ;
#14090 = CARTESIAN_POINT ( 'NONE',  ( 13.49062500061451786, 6.054752690667223547, 3.707466751127219781E-16 ) ) ;
#14091 = CARTESIAN_POINT ( 'NONE',  ( 10.77187500061451786, 3.027376345333613106, -5.243569643749998122 ) ) ;
#14092 = CARTESIAN_POINT ( 'NONE',  ( 8.971875000614515372, 3.027376345333613106, -5.243569643749998122 ) ) ;
#14093 = CARTESIAN_POINT ( 'NONE',  ( 17.03437500061451715, 6.421520780324663323E-16, -5.243569643749999010 ) ) ;
#14094 = ORIENTED_EDGE ( 'NONE', *, *, #23957, .T. ) ;
#14095 = CARTESIAN_POINT ( 'NONE',  ( -2.152738742430648777, 9.767338418468105132, 35.60400921600815138 ) ) ;
#14096 = CARTESIAN_POINT ( 'NONE',  ( 22.30312500061451431, -4.541064518000417216, -2.621784821875001281 ) ) ;
#14097 = CARTESIAN_POINT ( 'NONE',  ( 15.68437500061451573, 6.421520780324663323E-16, -5.243569643749999010 ) ) ;
#14098 = CARTESIAN_POINT ( 'NONE',  ( 22.90312500061451573, 4.541064518000418104, -2.621784821874998173 ) ) ;
#14099 = CARTESIAN_POINT ( 'NONE',  ( 1.999999999999998668, 15.35000000000000142, 26.53589838486224650 ) ) ;
#14100 = CARTESIAN_POINT ( 'NONE',  ( 26.61562500061451786, 3.027376345333611329, 5.243569643749999010 ) ) ;
#14101 = CARTESIAN_POINT ( 'NONE',  ( 7.275000001229035007, -5.773502691896255534, -1.060575238724906372E-15 ) ) ;
#14102 = ORIENTED_EDGE ( 'NONE', *, *, #36894, .F. ) ;
#14103 = CARTESIAN_POINT ( 'NONE',  ( 5.400000001229032343, -2.886751345948129988, 4.999999999999997335 ) ) ;
#14104 = CARTESIAN_POINT ( 'NONE',  ( 1.999999999999998668, 16.69999999999999929, -33.46410161513775705 ) ) ;
#14105 = CARTESIAN_POINT ( 'NONE',  ( 24.97500000122903430, 2.886751345948129099, -4.999999999999998224 ) ) ;
#14106 = CARTESIAN_POINT ( 'NONE',  ( 3.756430356250000546, 13.24062499938548321, 27.83122392262697886 ) ) ;
#14107 = VECTOR ( 'NONE', #63299, 1000.000000000000000 ) ;
#14108 = CARTESIAN_POINT ( 'NONE',  ( 7.321875000614516793, 3.027376345333611329, 5.243569643749999010 ) ) ;
#14109 = CARTESIAN_POINT ( 'NONE',  ( 20.60625000122902861, 0.000000000000000000, 4.999999999999998224 ) ) ;
#14110 = CARTESIAN_POINT ( 'NONE',  ( 14.95312500061451644, 0.000000000000000000, 5.243569643749999010 ) ) ;
#14111 = CARTESIAN_POINT ( 'NONE',  ( 9.421875000614519990, 3.027376345333613106, -5.243569643749998122 ) ) ;
#14112 = CARTESIAN_POINT ( 'NONE',  ( 26.55000000122902648, -2.886751345948129988, 4.999999999999997335 ) ) ;
#14113 =( BOUNDED_CURVE ( )  B_SPLINE_CURVE ( 2, ( #26716, #44073, #38149, #49250, #71785, #66602, #59576 ),
 .UNSPECIFIED., .F., .F. ) 
 B_SPLINE_CURVE_WITH_KNOTS ( ( 3, 2, 2, 3 ),
 ( 0.7833333333333334370, 0.7861111111111112049, 0.7888888888888888618, 0.7916666666666666297 ),
 .UNSPECIFIED. ) 
 CURVE ( )  GEOMETRIC_REPRESENTATION_ITEM ( )  RATIONAL_B_SPLINE_CURVE ( ( 0.9999999999999946709, 0.8660254037844440367, 1.000000000000000000, 0.8660254037844387076, 1.000000000000000000, 0.8660254037844387076, 1.000000000000000000 ) ) 
 REPRESENTATION_ITEM ( '' )  );
#14114 = CARTESIAN_POINT ( 'NONE',  ( 16.88437500061451502, -4.541064518000419881, 2.621784821874995952 ) ) ;
#14115 = CARTESIAN_POINT ( 'NONE',  ( 4.096875000614518925, 6.054752690667223547, 3.707466751127219781E-16 ) ) ;
#14116 = CARTESIAN_POINT ( 'NONE',  ( -5.000000000000004441, 0.000000000000000000, 4.999999999999998224 ) ) ;
#14117 = CARTESIAN_POINT ( 'NONE',  ( 6.590625000614518392, -3.027376345333610441, -5.243569643749999898 ) ) ;
#14118 =( BOUNDED_CURVE ( )  B_SPLINE_CURVE ( 2, ( #68643, #52011, #18006, #13194, #40938, #18729, #1774 ),
 .UNSPECIFIED., .F., .F. ) 
 B_SPLINE_CURVE_WITH_KNOTS ( ( 3, 2, 2, 3 ),
 ( 0.9855061078632572080, 0.9861111111111111605, 0.9888888888888889284, 0.9894304826859887658 ),
 .UNSPECIFIED. ) 
 CURVE ( )  GEOMETRIC_REPRESENTATION_ITEM ( )  RATIONAL_B_SPLINE_CURVE ( ( 0.9543511520354772681, 0.9708201762974799642, 1.000000000000000000, 0.8660254037844387076, 1.000000000000000000, 0.9738784682994507946, 0.9579429634675318272 ) ) 
 REPRESENTATION_ITEM ( '' )  );
#14119 = CARTESIAN_POINT ( 'NONE',  ( 14.91562500061451679, 3.027376345333611329, 5.243569643749999010 ) ) ;
#14120 = EDGE_LOOP ( 'NONE', ( #29700, #57009, #23078, #30077 ) ) ;
#14121 = ADVANCED_FACE ( 'NONE', ( #33914, #38373, #315 ), #60898, .T. ) ;
#14122 = CARTESIAN_POINT ( 'NONE',  ( 12.85312500061451502, -4.541064518000417216, -2.621784821875001281 ) ) ;
#14123 = CARTESIAN_POINT ( 'NONE',  ( 4.800000001229032698, 5.773502691896255534, 3.535250795749688894E-16 ) ) ;
#14124 = CARTESIAN_POINT ( 'NONE',  ( 11.27812500061451573, 4.541064518000418104, 2.621784821874999949 ) ) ;
#14125 = CARTESIAN_POINT ( 'NONE',  ( 21.08437500061451786, 5.824947211148865298E-16, -4.756430356249998326 ) ) ;
#14126 = CARTESIAN_POINT ( 'NONE',  ( 10.35000000000000142, -4.330127018922190985, -2.500000000000001332 ) ) ;
#14127 = CARTESIAN_POINT ( 'NONE',  ( 7.350000001229033408, -2.886751345948125991, -5.000000000000000000 ) ) ;
#14128 = CARTESIAN_POINT ( 'NONE',  ( 19.27500000000000213, -4.330127018922194537, 2.499999999999995559 ) ) ;
#14129 = ADVANCED_FACE ( 'NONE', ( #5127 ), #22824, .F. ) ;
#14130 =( BOUNDED_CURVE ( )  B_SPLINE_CURVE ( 2, ( #17326, #45057, #28069, #22150, #10705, #11066, #62398, #67594, #45783 ),
 .UNSPECIFIED., .F., .T. ) 
 B_SPLINE_CURVE_WITH_KNOTS ( ( 3, 2, 2, 2, 3 ),
 ( 0.2282608695652174058, 0.2318840579710144956, 0.2391304347826087029, 0.2463768115942029102, 0.2500000000000000000 ),
 .UNSPECIFIED. ) 
 CURVE ( )  GEOMETRIC_REPRESENTATION_ITEM ( )  RATIONAL_B_SPLINE_CURVE ( ( 0.9330127018922194093, 0.9330127018922196314, 1.000000000000000000, 0.8660254037844387076, 1.000000000000000000, 0.8660254037844387076, 1.000000000000000000, 0.9330127018922196314, 0.9330127018922194093 ) ) 
 REPRESENTATION_ITEM ( '' )  );
#14131 = CARTESIAN_POINT ( 'NONE',  ( 15.23437500061451644, 6.421520780324663323E-16, -5.243569643749999010 ) ) ;
#14132 = CARTESIAN_POINT ( 'NONE',  ( 16.98750000122903359, 4.330127018922191873, 2.499999999999999556 ) ) ;
#14133 = CARTESIAN_POINT ( 'NONE',  ( 22.12500000000000000, 6.123233995736764310E-16, -4.999999999999998224 ) ) ;
#14134 = CARTESIAN_POINT ( 'NONE',  ( -4.243569643749997233, 19.39062500061451999, -27.54997392385601174 ) ) ;
#14135 = CARTESIAN_POINT ( 'NONE',  ( 4.000000000000000000, 20.15000000000000213, 30.00000000000000000 ) ) ;
#14136 = CARTESIAN_POINT ( 'NONE',  ( -3.999999999999997335, 18.68750000000000000, 32.30940107675850470 ) ) ;
#14137 = CARTESIAN_POINT ( 'NONE',  ( 23.10000000122903074, -2.886751345948142422, -4.999999999999970690 ) ) ;
#14138 = CARTESIAN_POINT ( 'NONE',  ( 3.494527216699953698, -3.576116613012044976, 3.526356099291672042 ) ) ;
#14139 = DIRECTION ( 'NONE',  ( 0.000000000000000000, 0.000000000000000000, 1.000000000000000000 ) ) ;
#14140 = CARTESIAN_POINT ( 'NONE',  ( 15.27187500061451786, 3.027376345333613106, -5.243569643749998122 ) ) ;
#14141 = EDGE_CURVE ( 'NONE', #2091, #8533, #6793, .T. ) ;
#14142 = CARTESIAN_POINT ( 'NONE',  ( 28.01249999999999574, 2.886751345948129099, -4.999999999999998224 ) ) ;
#14143 = CARTESIAN_POINT ( 'NONE',  ( 11.72812500061451857, 4.541064518000418104, 2.621784821874999949 ) ) ;
#14144 = CARTESIAN_POINT ( 'NONE',  ( 28.99687500061451217, -4.119189519843965641, -2.378215178125001383 ) ) ;
#14145 = CARTESIAN_POINT ( 'NONE',  ( 22.88437500061451857, 6.421520780324663323E-16, -5.243569643749999010 ) ) ;
#14146 = CARTESIAN_POINT ( 'NONE',  ( 16.32187500061451502, -4.119189519843968306, 2.378215178124996054 ) ) ;
#14147 = CARTESIAN_POINT ( 'NONE',  ( 8.915625000614515017, 3.027376345333613106, -5.243569643749998122 ) ) ;
#14148 = CARTESIAN_POINT ( 'NONE',  ( 14.67187500061451821, -6.054752690667223547, -1.112240025338166033E-15 ) ) ;
#14149 = ORIENTED_EDGE ( 'NONE', *, *, #37745, .T. ) ;
#14150 = CARTESIAN_POINT ( 'NONE',  ( 26.03437500061451715, 6.421520780324663323E-16, -5.243569643749999010 ) ) ;
#14151 = CARTESIAN_POINT ( 'NONE',  ( 28.45312500061451289, 0.000000000000000000, 5.243569643749999010 ) ) ;
#14152 = CARTESIAN_POINT ( 'NONE',  ( 27.89062500061451289, 6.054752690667223547, 3.707466751127219781E-16 ) ) ;
#14153 = CARTESIAN_POINT ( 'NONE',  ( 3.939080010846523372, -3.079553322829319928, -4.243980907203444453 ) ) ;
#14154 = CARTESIAN_POINT ( 'NONE',  ( 8.362500000000002487, 2.886751345948126879, 4.999999999999999112 ) ) ;
#14155 = CARTESIAN_POINT ( 'NONE',  ( 16.08750000122903501, 4.330127018922191873, 2.499999999999999556 ) ) ;
#14156 = CARTESIAN_POINT ( 'NONE',  ( -1.626862140677534273E-15, 19.98124999877096641, 34.00000000000000000 ) ) ;
#14157 = CARTESIAN_POINT ( 'NONE',  ( 7.659375000614514484, 2.746126346562643317, 4.756430356249998326 ) ) ;
#14158 = VERTEX_POINT ( 'NONE', #22108 ) ;
#14159 = CARTESIAN_POINT ( 'NONE',  ( 15.00000000000000000, 4.330127018922192761, -2.499999999999997780 ) ) ;
#14160 = CARTESIAN_POINT ( 'NONE',  ( 19.57500000000000284, 4.330127018922191873, 2.499999999999999556 ) ) ;
#14161 = CARTESIAN_POINT ( 'NONE',  ( 13.64062500061451644, -3.027376345333614438, 5.243569643749998122 ) ) ;
#14162 = ORIENTED_EDGE ( 'NONE', *, *, #30313, .T. ) ;
#14163 = DIRECTION ( 'NONE',  ( 1.000000000000000000, 0.000000000000000000, 0.000000000000000000 ) ) ;
#14164 = CARTESIAN_POINT ( 'NONE',  ( 4.243569643749999898, 15.99687500061451573, -27.54997392385601529 ) ) ;
#14165 = CARTESIAN_POINT ( 'NONE',  ( 6.778125000614518392, 4.541064518000418104, 2.621784821874999949 ) ) ;
#14166 = CARTESIAN_POINT ( 'NONE',  ( 3.756430356250000102, 13.09062499938548463, 30.00000000000000000 ) ) ;
#14167 = CARTESIAN_POINT ( 'NONE',  ( 11.17500000000000071, -4.330127018922194537, 2.499999999999995559 ) ) ;
#14168 = CARTESIAN_POINT ( 'NONE',  ( 28.92187500061451644, -4.119189519843968306, 2.378215178124996054 ) ) ;
#14169 = ORIENTED_EDGE ( 'NONE', *, *, #1145, .F. ) ;
#14170 = CARTESIAN_POINT ( 'NONE',  ( 4.243569643749999898, 15.97812500061451857, 30.00000000000000000 ) ) ;
#14171 = CARTESIAN_POINT ( 'NONE',  ( 27.29062500061451502, -3.027376345333610441, -5.243569643749999898 ) ) ;
#14172 = CARTESIAN_POINT ( 'NONE',  ( 7.724999999999999645, 6.123233995736764310E-16, -4.999999999999998224 ) ) ;
#14173 = CARTESIAN_POINT ( 'NONE',  ( -3.756430356250000102, 16.91562499938548214, 30.00000000000000000 ) ) ;
#14174 = CARTESIAN_POINT ( 'NONE',  ( 23.10937500061451644, 0.000000000000000000, 5.243569643749999010 ) ) ;
#14175 = CARTESIAN_POINT ( 'NONE',  ( 20.46562500061451928, -6.054752690667223547, -1.112240025338166033E-15 ) ) ;
#14176 = CARTESIAN_POINT ( 'NONE',  ( -2.121784821874999949, 14.77812500061459389, -33.67503911421598417 ) ) ;
#14177 = CARTESIAN_POINT ( 'NONE',  ( 22.65000000122903856, -2.886751345948125991, -5.000000000000000000 ) ) ;
#14178 = CARTESIAN_POINT ( 'NONE',  ( 5.465625000614517504, 3.027376345333611329, 5.243569643749999010 ) ) ;
#14179 = CARTESIAN_POINT ( 'NONE',  ( 27.68437500061451573, -4.119189519843968306, 2.378215178124996054 ) ) ;
#14180 = CARTESIAN_POINT ( 'NONE',  ( 21.92812500061451431, 6.421520780324663323E-16, -5.243569643749999010 ) ) ;
#14181 = CARTESIAN_POINT ( 'NONE',  ( 11.18437500061451928, 5.824947211148865298E-16, -4.756430356249998326 ) ) ;
#14182 = CARTESIAN_POINT ( 'NONE',  ( -7.967954043666661671E-16, 15.22812499938548214, 34.33755215474603517 ) ) ;
#14183 = CARTESIAN_POINT ( 'NONE',  ( 16.43437500061451573, -4.541064518000419881, 2.621784821874995952 ) ) ;
#14184 = CARTESIAN_POINT ( 'NONE',  ( 25.17187500061451644, 3.027376345333613106, -5.243569643749998122 ) ) ;
#14185 = CARTESIAN_POINT ( 'NONE',  ( -4.243569643749999898, 15.32187500061451502, 27.54997392385601529 ) ) ;
#14186 = CARTESIAN_POINT ( 'NONE',  ( 4.715625000614516615, -6.054752690667223547, -1.112240025338166033E-15 ) ) ;
#14187 = CARTESIAN_POINT ( 'NONE',  ( 29.80312500061451431, 0.000000000000000000, 5.243569643749999010 ) ) ;
#14188 = CARTESIAN_POINT ( 'NONE',  ( 29.05312500061451431, -4.541064518000417216, -2.621784821875001281 ) ) ;
#14189 = LINE ( 'NONE', #3118, #61961 ) ;
#14190 = CARTESIAN_POINT ( 'NONE',  ( 0.8114860633430618364, 9.969066991719973458, -35.94832491657660256 ) ) ;
#14191 = CARTESIAN_POINT ( 'NONE',  ( 29.21250000122903145, 0.000000000000000000, 4.999999999999998224 ) ) ;
#14192 = CARTESIAN_POINT ( 'NONE',  ( 7.996875000614519280, -3.027376345333610441, -5.243569643749999898 ) ) ;
#14193 = CARTESIAN_POINT ( 'NONE',  ( 14.81250000122903288, 0.000000000000000000, 4.999999999999998224 ) ) ;
#14194 = CARTESIAN_POINT ( 'NONE',  ( 3.646875000614520079, 6.054752690667223547, 3.707466751127219781E-16 ) ) ;
#14195 = CARTESIAN_POINT ( 'NONE',  ( 10.95000000122903394, -2.886751345948125991, -5.000000000000000000 ) ) ;
#14196 = CARTESIAN_POINT ( 'NONE',  ( 5.053125000614517859, 0.000000000000000000, 5.243569643749999010 ) ) ;
#14197 = CARTESIAN_POINT ( 'NONE',  ( 3.999999999999998668, 14.65624999877096535, 32.30940107675850470 ) ) ;
#14198 = CARTESIAN_POINT ( 'NONE',  ( 20.30625000122903145, -4.330127018922190985, -2.500000000000001332 ) ) ;
#14199 = CARTESIAN_POINT ( 'NONE',  ( 14.07187500061451679, 3.027376345333611329, 5.243569643749999010 ) ) ;
#14200 = CARTESIAN_POINT ( 'NONE',  ( 7.687499999999998224, -2.886751345948193048, -4.999999999999883649 ) ) ;
#14201 = EDGE_LOOP ( 'NONE', ( #69016, #43451, #47137, #36436 ) ) ;
#14202 = CARTESIAN_POINT ( 'NONE',  ( 21.89062500061451289, -3.027376345333610441, -5.243569643749999898 ) ) ;
#14203 = CARTESIAN_POINT ( 'NONE',  ( 6.365625000614518747, 3.027376345333611329, 5.243569643749999010 ) ) ;
#14204 = CARTESIAN_POINT ( 'NONE',  ( 25.47187500061451715, -6.054752690667223547, -1.112240025338166033E-15 ) ) ;
#14205 = CARTESIAN_POINT ( 'NONE',  ( 6.553125000614518747, -4.541064518000417216, -2.621784821875001281 ) ) ;
#14206 = CARTESIAN_POINT ( 'NONE',  ( 13.57500000000000107, 6.123233995736764310E-16, -4.999999999999998224 ) ) ;
#14207 = CARTESIAN_POINT ( 'NONE',  ( 8.137500001229033941, -4.330127018922194537, 2.499999999999995559 ) ) ;
#14208 = CARTESIAN_POINT ( 'NONE',  ( 24.14062500061451289, -3.027376345333610441, -5.243569643749999898 ) ) ;
#14209 = CARTESIAN_POINT ( 'NONE',  ( -4.243569643749997233, 10.84062500061451395, -27.54997392385601174 ) ) ;
#14210 = CARTESIAN_POINT ( 'NONE',  ( 9.262500001229033941, 4.330127018922192761, -2.499999999999997780 ) ) ;
#14211 = CARTESIAN_POINT ( 'NONE',  ( 20.72812500061451502, 4.541064518000418104, 2.621784821874999949 ) ) ;
#14213 = EDGE_CURVE ( 'NONE', #38333, #12248, #70458, .T. ) ;
#14212 = CARTESIAN_POINT ( 'NONE',  ( 18.66562500061451146, -6.054752690667223547, -1.112240025338166033E-15 ) ) ;
#14214 = CARTESIAN_POINT ( 'NONE',  ( 28.39687500061452141, 5.492252693125287522, 3.363034840372157021E-16 ) ) ;
#14215 = EDGE_CURVE ( 'NONE', #50028, #7649, #5491, .T. ) ;
#14216 = CARTESIAN_POINT ( 'NONE',  ( 18.63749999999999929, 5.773502691896255534, 3.535250795749688894E-16 ) ) ;
#14217 = CARTESIAN_POINT ( 'NONE',  ( 13.31250000122903288, 4.330127018922192761, -2.499999999999997780 ) ) ;
#14218 = CARTESIAN_POINT ( 'NONE',  ( 10.37812500061451715, 4.541064518000418104, 2.621784821874999949 ) ) ;
#14219 = CARTESIAN_POINT ( 'NONE',  ( 12.81562500061451537, -6.054752690667223547, -1.112240025338166033E-15 ) ) ;
#14220 = CARTESIAN_POINT ( 'NONE',  ( 23.13750000122903216, 6.123233995736764310E-16, -4.999999999999998224 ) ) ;
#14221 = CARTESIAN_POINT ( 'NONE',  ( 22.95937500061451431, 4.541064518000418104, -2.621784821874998173 ) ) ;
#14222 = CARTESIAN_POINT ( 'NONE',  ( 21.38437500061451502, -4.541064518000419881, 2.621784821874995952 ) ) ;
#14223 = CARTESIAN_POINT ( 'NONE',  ( -2.498395430326213790E-14, 18.46250000000000213, 26.00000000000000000 ) ) ;
#14224 = CARTESIAN_POINT ( 'NONE',  ( 7.387500001229032165, 6.123233995736764310E-16, -4.999999999999998224 ) ) ;
#14225 = CARTESIAN_POINT ( 'NONE',  ( 5.596875000614516260, -3.027376345333614438, 5.243569643749998122 ) ) ;
#14226 = CARTESIAN_POINT ( 'NONE',  ( 23.22187500061451715, -6.054752690667223547, -1.112240025338166033E-15 ) ) ;
#14227 = CARTESIAN_POINT ( 'NONE',  ( 4.761519200037192867, -1.526514057201037611, 4.869786965056912997 ) ) ;
#14228 = CARTESIAN_POINT ( 'NONE',  ( 18.55312500061451431, 0.000000000000000000, 5.243569643749999010 ) ) ;
#14229 = CARTESIAN_POINT ( 'NONE',  ( 24.68437500061451573, 6.421520780324663323E-16, -5.243569643749999010 ) ) ;
#14230 = CARTESIAN_POINT ( 'NONE',  ( -3.756430356249999214, 20.14062499938548356, 27.83122392262697176 ) ) ;
#14231 = CARTESIAN_POINT ( 'NONE',  ( 3.384375000614517237, -4.541064518000419881, 2.621784821874995952 ) ) ;
#14232 = CARTESIAN_POINT ( 'NONE',  ( 1.071796769724489895, 15.81740381056766509, 26.00000000000000355 ) ) ;
#14233 = CARTESIAN_POINT ( 'NONE',  ( 5.896875000614518747, 6.054752690667223547, 3.707466751127219781E-16 ) ) ;
#14234 = CARTESIAN_POINT ( 'NONE',  ( 17.61562500061451786, 3.027376345333611329, 5.243569643749999010 ) ) ;
#14235 = ORIENTED_EDGE ( 'NONE', *, *, #60001, .F. ) ;
#14236 = CARTESIAN_POINT ( 'NONE',  ( 22.83749999999999858, -2.886751345948163738, 4.999999999999939604 ) ) ;
#14237 = CARTESIAN_POINT ( 'NONE',  ( 24.62812500061451715, 6.421520780324663323E-16, -5.243569643749999010 ) ) ;
#14238 = CARTESIAN_POINT ( 'NONE',  ( -3.999999999999999112, 10.66250000122903430, -30.00000000000000000 ) ) ;
#14239 = LINE ( 'NONE', #64851, #7703 ) ;
#14240 = CARTESIAN_POINT ( 'NONE',  ( 13.79999999999999893, 0.000000000000000000, 4.999999999999998224 ) ) ;
#14241 = CARTESIAN_POINT ( 'NONE',  ( 25.38750000122903216, 6.123233995736764310E-16, -4.999999999999998224 ) ) ;
#14242 = CARTESIAN_POINT ( 'NONE',  ( 21.92812500061451431, 6.421520780324663323E-16, -5.243569643749999010 ) ) ;
#14243 = ORIENTED_EDGE ( 'NONE', *, *, #25676, .F. ) ;
#14244 = CARTESIAN_POINT ( 'NONE',  ( 23.09999999999999787, 4.330127018922192761, -2.499999999999997780 ) ) ;
#14245 = CARTESIAN_POINT ( 'NONE',  ( 22.99687500061451573, 6.054752690667223547, 3.707466751127219781E-16 ) ) ;
#14246 = ORIENTED_EDGE ( 'NONE', *, *, #34911, .T. ) ;
#14247 = FACE_OUTER_BOUND ( 'NONE', #20157, .T. ) ;
#14248 = CARTESIAN_POINT ( 'NONE',  ( 13.97812500061451679, 4.541064518000418104, 2.621784821874999949 ) ) ;
#14249 = CARTESIAN_POINT ( 'NONE',  ( 3.740625000614516527, -3.027376345333614438, 5.243569643749998122 ) ) ;
#14250 = CARTESIAN_POINT ( 'NONE',  ( 17.29687500061451644, -4.119189519843965641, -2.378215178125001383 ) ) ;
#14251 = CARTESIAN_POINT ( 'NONE',  ( 25.71562500061451573, 3.027376345333611329, 5.243569643749999010 ) ) ;
#14252 = CARTESIAN_POINT ( 'NONE',  ( 13.68750000122903288, 6.123233995736764310E-16, -4.999999999999998224 ) ) ;
#14253 = CARTESIAN_POINT ( 'NONE',  ( 18.48750000000000071, -2.886751345948125991, -5.000000000000000000 ) ) ;
#14254 = CARTESIAN_POINT ( 'NONE',  ( 26.55000000000000071, -4.330127018922190985, -2.500000000000001332 ) ) ;
#14255 = CARTESIAN_POINT ( 'NONE',  ( 3.225000001229032964, -5.773502691896255534, -1.060575238724906372E-15 ) ) ;
#14256 = CARTESIAN_POINT ( 'NONE',  ( 6.571875000614517681, -6.054752690667223547, -1.112240025338166033E-15 ) ) ;
#14257 = CARTESIAN_POINT ( 'NONE',  ( 19.88437500061451857, 4.541064518000418104, 2.621784821874999949 ) ) ;
#14258 = CARTESIAN_POINT ( 'NONE',  ( 1.071796769724489895, 11.42990381179669868, 26.00000000000000355 ) ) ;
#14259 = VERTEX_POINT ( 'NONE', #67912 ) ;
#14260 = CARTESIAN_POINT ( 'NONE',  ( 29.31562500061451715, 3.027376345333611329, 5.243569643749999010 ) ) ;
#14261 = CARTESIAN_POINT ( 'NONE',  ( 29.67187500061451644, 3.027376345333613106, -5.243569643749998122 ) ) ;
#14262 = CARTESIAN_POINT ( 'NONE',  ( 5.521875000614517859, 3.027376345333611329, 5.243569643749999010 ) ) ;
#14263 = CARTESIAN_POINT ( 'NONE',  ( 15.22500000000000142, -4.330127018922194537, 2.499999999999995559 ) ) ;
#14264 = CARTESIAN_POINT ( 'NONE',  ( 13.15312500061451750, 0.000000000000000000, 5.243569643749999010 ) ) ;
#14265 = CARTESIAN_POINT ( 'NONE',  ( -1.999999999999997113, 15.12500000000000000, -26.53589838486224295 ) ) ;
#14266 = DIRECTION ( 'NONE',  ( -1.000000000000000000, -0.000000000000000000, -0.000000000000000000 ) ) ;
#14267 = DIRECTION ( 'NONE',  ( -0.000000000000000000, -1.000000000000000000, -0.000000000000000000 ) ) ;
#14268 = CARTESIAN_POINT ( 'NONE',  ( 19.20000000122903572, 5.773502691896255534, 3.535250795749688894E-16 ) ) ;
#14269 = CARTESIAN_POINT ( 'NONE',  ( 26.94375000122903430, -2.886751345948088243, 5.000000000000068390 ) ) ;
#14270 = CARTESIAN_POINT ( 'NONE',  ( 17.44687500061451857, -2.746126346562642428, -4.756430356249999214 ) ) ;
#14271 = CARTESIAN_POINT ( 'NONE',  ( 8.090625000614515727, 6.054752690667223547, 3.707466751127219781E-16 ) ) ;
#14272 = CARTESIAN_POINT ( 'NONE',  ( 24.64687500061451431, -3.027376345333610441, -5.243569643749999898 ) ) ;
#14273 = CARTESIAN_POINT ( 'NONE',  ( -4.243569643749997233, 17.64687500061452141, 32.45002607614398471 ) ) ;
#14274 = CARTESIAN_POINT ( 'NONE',  ( 24.64687500061451431, -3.027376345333610441, -5.243569643749999898 ) ) ;
#14275 = CARTESIAN_POINT ( 'NONE',  ( 4.275000000000001243, 4.330127018922191873, 2.499999999999999556 ) ) ;
#14276 = CARTESIAN_POINT ( 'NONE',  ( -0.6945863667395647534, 9.663023495605401081, 26.06076786935073741 ) ) ;
#14277 = CARTESIAN_POINT ( 'NONE',  ( 13.45312500061451466, 4.541064518000418104, -2.621784821874998173 ) ) ;
#14278 = CARTESIAN_POINT ( 'NONE',  ( 5.550000001229032698, -2.886751345948125991, -5.000000000000000000 ) ) ;
#14279 = EDGE_CURVE ( 'NONE', #31892, #68516, #60087, .T. ) ;
#14280 = PRODUCT ( 'pressure gauge', 'pressure gauge', '', ( #60715 ) ) ;
#14281 = CARTESIAN_POINT ( 'NONE',  ( 8.446875000614518569, -3.027376345333610441, -5.243569643749999898 ) ) ;
#14282 = CARTESIAN_POINT ( 'NONE',  ( 2.000000000000001332, 14.86250000122903536, 33.46410161513774995 ) ) ;
#14283 = EDGE_LOOP ( 'NONE', ( #14020, #50633, #18140, #65950 ) ) ;
#14284 = CARTESIAN_POINT ( 'NONE',  ( 10.90312500061451928, 0.000000000000000000, 5.243569643749999010 ) ) ;
#14285 = CARTESIAN_POINT ( 'NONE',  ( 14.33437500061451786, 6.421520780324663323E-16, -5.243569643749999010 ) ) ;
#14286 = LINE ( 'NONE', #2843, #35536 ) ;
#14287 = CARTESIAN_POINT ( 'NONE',  ( 24.26250000122903216, 0.000000000000000000, 4.999999999999998224 ) ) ;
#14288 = CARTESIAN_POINT ( 'NONE',  ( 9.759375000614516793, -4.541064518000417216, -2.621784821875001281 ) ) ;
#14289 = CARTESIAN_POINT ( 'NONE',  ( 12.14062500061451821, 6.054752690667223547, 3.707466751127219781E-16 ) ) ;
#14290 = CARTESIAN_POINT ( 'NONE',  ( 28.10625000122902861, 4.330127018922192761, -2.499999999999997780 ) ) ;
#14291 = CARTESIAN_POINT ( 'NONE',  ( 20.82187500061451857, 3.027376345333611329, 5.243569643749999010 ) ) ;
#14292 = CARTESIAN_POINT ( 'NONE',  ( 26.86875000122903145, 2.886751345948168623, 4.999999999999926281 ) ) ;
#14293 = CARTESIAN_POINT ( 'NONE',  ( 5.250000000000000888, 0.000000000000000000, 4.999999999999998224 ) ) ;
#14294 = CARTESIAN_POINT ( 'NONE',  ( -2.928932188134524939, 4.999999999999996447, 2.928932188134524939 ) ) ;
#14295 = CARTESIAN_POINT ( 'NONE',  ( -4.243569643749999898, 13.52187500061451786, -32.45002607614398471 ) ) ;
#14296 = CARTESIAN_POINT ( 'NONE',  ( 15.27187500061451786, 3.027376345333613106, -5.243569643749998122 ) ) ;
#14297 = CARTESIAN_POINT ( 'NONE',  ( 18.67500000122903714, 2.886751345948129099, -4.999999999999998224 ) ) ;
#14298 = CARTESIAN_POINT ( 'NONE',  ( 13.43437500061451750, 6.421520780324663323E-16, -5.243569643749999010 ) ) ;
#14299 = CARTESIAN_POINT ( 'NONE',  ( -4.243569643749997233, 18.49062500061451431, -27.54997392385601174 ) ) ;
#14300 = CARTESIAN_POINT ( 'NONE',  ( 17.96250000122903501, 0.000000000000000000, 4.999999999999998224 ) ) ;
#14301 = CARTESIAN_POINT ( 'NONE',  ( 11.61562500061451608, 3.027376345333613106, -5.243569643749998122 ) ) ;
#14302 = ORIENTED_EDGE ( 'NONE', *, *, #16136, .T. ) ;
#14303 = CARTESIAN_POINT ( 'NONE',  ( 14.77500000000000036, -4.330127018922194537, 2.499999999999995559 ) ) ;
#14304 = CARTESIAN_POINT ( 'NONE',  ( 4.924325218087134637, -0.8666147624583920850, 4.924325218087160394 ) ) ;
#14305 = CARTESIAN_POINT ( 'NONE',  ( 9.459375000614517859, 4.541064518000418104, -2.621784821874998173 ) ) ;
#14306 = EDGE_CURVE ( 'NONE', #32563, #34347, #61994, .T. ) ;
#14307 = CARTESIAN_POINT ( 'NONE',  ( 4.111889464957033447, 2.844708250062874644, 4.404844785106587501 ) ) ;
#14308 = CARTESIAN_POINT ( 'NONE',  ( 13.20000000122903394, -2.886751345948125991, -5.000000000000000000 ) ) ;
#14309 = CARTESIAN_POINT ( 'NONE',  ( 20.88750000122903572, 6.123233995736764310E-16, -4.999999999999998224 ) ) ;
#14310 = CARTESIAN_POINT ( 'NONE',  ( 18.40312500061451573, 4.541064518000418104, -2.621784821874998173 ) ) ;
#14311 = CARTESIAN_POINT ( 'NONE',  ( 19.97812500061451502, -4.541064518000419881, 2.621784821874995952 ) ) ;
#14312 = CARTESIAN_POINT ( 'NONE',  ( 28.35000000122903430, -2.886751345948129988, 4.999999999999997335 ) ) ;
#14313 = CARTESIAN_POINT ( 'NONE',  ( 24.86250000000000071, 2.886751345948129099, -4.999999999999998224 ) ) ;
#14314 = CARTESIAN_POINT ( 'NONE',  ( 28.42499999999999716, 6.123233995736764310E-16, -4.999999999999998224 ) ) ;
#14315 = CARTESIAN_POINT ( 'NONE',  ( 28.80000000000000071, -4.330127018922190985, -2.500000000000001332 ) ) ;
#14316 = CARTESIAN_POINT ( 'NONE',  ( 28.28437500061451715, 6.421520780324663323E-16, -5.243569643749999010 ) ) ;
#14317 = CARTESIAN_POINT ( 'NONE',  ( 11.58750000000000036, -2.886751345948130876, 4.999999999999996447 ) ) ;
#14318 = CARTESIAN_POINT ( 'NONE',  ( 2.121784821875001281, 14.15937500061451715, -26.32496088578401938 ) ) ;
#14319 = EDGE_CURVE ( 'NONE', #60669, #64001, #56457, .T. ) ;
#14320 = CARTESIAN_POINT ( 'NONE',  ( 3.787500001229033408, 6.123233995736764310E-16, -4.999999999999998224 ) ) ;
#14321 = CARTESIAN_POINT ( 'NONE',  ( 4.349999999999999645, 0.000000000000000000, 4.999999999999998224 ) ) ;
#14322 = CARTESIAN_POINT ( 'NONE',  ( 27.44999999999999929, -4.330127018922190985, -2.500000000000001332 ) ) ;
#14323 = CARTESIAN_POINT ( 'NONE',  ( 7.846875000614518036, -3.027376345333614438, 5.243569643749998122 ) ) ;
#14324 = CARTESIAN_POINT ( 'NONE',  ( 29.24062500061451431, 6.054752690667223547, 3.707466751127219781E-16 ) ) ;
#14325 = CARTESIAN_POINT ( 'NONE',  ( 9.206250001229033586, 4.330127018922192761, -2.499999999999997780 ) ) ;
#14326 = CARTESIAN_POINT ( 'NONE',  ( 2.000000000000001332, 10.36250000122903359, 33.46410161513774995 ) ) ;
#14327 = CARTESIAN_POINT ( 'NONE',  ( 1.510657702057710734E-15, 19.10000000122903430, 26.00000000000000000 ) ) ;
#14328 = CARTESIAN_POINT ( 'NONE',  ( 4.771875000614516971, -6.054752690667223547, -1.112240025338166033E-15 ) ) ;
#14329 = CARTESIAN_POINT ( 'NONE',  ( 9.909375000614517148, 4.541064518000418104, -2.621784821874998173 ) ) ;
#14330 = CARTESIAN_POINT ( 'NONE',  ( 3.337499999999999911, 5.773502691896255534, 3.535250795749688894E-16 ) ) ;
#14331 = CARTESIAN_POINT ( 'NONE',  ( -4.243569643749999898, 13.50312500061459531, 30.00000000000000000 ) ) ;
#14332 = MECHANICAL_DESIGN_GEOMETRIC_PRESENTATION_REPRESENTATION (  '', ( #46204 ), #65071 ) ;
#14333 = CARTESIAN_POINT ( 'NONE',  ( 1.999999999999998668, 18.05000000000000071, 26.53589838486224650 ) ) ;
#14334 =( BOUNDED_CURVE ( )  B_SPLINE_CURVE ( 2, ( #38899, #10090, #15611, #11541, #5996, #72504, #21893 ),
 .UNSPECIFIED., .F., .F. ) 
 B_SPLINE_CURVE_WITH_KNOTS ( ( 3, 2, 2, 3 ),
 ( 0.5583333333333333481, 0.5611111111111111160, 0.5638888888888889950, 0.5666666666666667629 ),
 .UNSPECIFIED. ) 
 CURVE ( )  GEOMETRIC_REPRESENTATION_ITEM ( )  RATIONAL_B_SPLINE_CURVE ( ( 1.000000000000000000, 0.8660254037844387076, 1.000000000000000000, 0.8660254037844387076, 1.000000000000000000, 0.8660254037844333785, 1.000000000000005329 ) ) 
 REPRESENTATION_ITEM ( '' )  );
#14335 = CARTESIAN_POINT ( 'NONE',  ( 4.349999999999999645, 0.000000000000000000, 4.999999999999998224 ) ) ;
#14336 = CARTESIAN_POINT ( 'NONE',  ( 15.08437500061451431, -2.746126346562642428, -4.756430356249999214 ) ) ;
#14337 = CARTESIAN_POINT ( 'NONE',  ( 21.36562500061451431, -6.054752690667223547, -1.112240025338166033E-15 ) ) ;
#14338 = CARTESIAN_POINT ( 'NONE',  ( 11.65312500061451573, 4.541064518000418104, -2.621784821874998173 ) ) ;
#14339 = CARTESIAN_POINT ( 'NONE',  ( 23.59687500061451360, -4.119189519843965641, -2.378215178125001383 ) ) ;
#14340 = CARTESIAN_POINT ( 'NONE',  ( 9.609375000614518214, 0.000000000000000000, 5.243569643749999010 ) ) ;
#14341 = CARTESIAN_POINT ( 'NONE',  ( 25.16249999999999432, -5.773502691896255534, -1.060575238724906372E-15 ) ) ;
#14342 = CARTESIAN_POINT ( 'NONE',  ( 21.07500000122903572, 2.886751345948126879, 4.999999999999999112 ) ) ;
#14343 = CARTESIAN_POINT ( 'NONE',  ( 28.71562500061451573, 3.027376345333613106, -5.243569643749998122 ) ) ;
#14344 = CARTESIAN_POINT ( 'NONE',  ( 15.37500000000000000, 6.123233995736764310E-16, -4.999999999999998224 ) ) ;
#14345 = CARTESIAN_POINT ( 'NONE',  ( 8.671875000614518214, 3.027376345333611329, 5.243569643749999010 ) ) ;
#14346 = CARTESIAN_POINT ( 'NONE',  ( 15.12187500061451750, -6.054752690667223547, -1.112240025338166033E-15 ) ) ;
#14347 = CARTESIAN_POINT ( 'NONE',  ( 27.19687500061451857, -3.027376345333614438, 5.243569643749998122 ) ) ;
#14348 = CARTESIAN_POINT ( 'NONE',  ( 4.303125000614516971, -4.541064518000417216, -2.621784821875001281 ) ) ;
#14349 = CARTESIAN_POINT ( 'NONE',  ( 11.84999999999999964, 4.330127018922192761, -2.499999999999997780 ) ) ;
#14350 = CARTESIAN_POINT ( 'NONE',  ( 21.08437500061451786, 6.421520780324663323E-16, -5.243569643749999010 ) ) ;
#14351 = CARTESIAN_POINT ( 'NONE',  ( 10.65937500061451715, -4.541064518000417216, -2.621784821875001281 ) ) ;
#14352 = CARTESIAN_POINT ( 'NONE',  ( -1.878215178124999163, 13.69062499938548427, 26.74683588394047007 ) ) ;
#14353 = CARTESIAN_POINT ( 'NONE',  ( 23.17500000000000071, 4.330127018922191873, 2.499999999999999556 ) ) ;
#14354 = CARTESIAN_POINT ( 'NONE',  ( -8.484601909799255319E-16, 14.18750000000000000, 34.61880215351700940 ) ) ;
#14355 = CARTESIAN_POINT ( 'NONE',  ( -2.121784821874996840, 12.73437500061451821, -26.32496088578401583 ) ) ;
#14356 = CARTESIAN_POINT ( 'NONE',  ( 25.58437500061451431, 5.824947211148865298E-16, -4.756430356249998326 ) ) ;
#14357 = CARTESIAN_POINT ( 'NONE',  ( 14.87812500061451537, 4.541064518000418104, 2.621784821874999949 ) ) ;
#14358 = CARTESIAN_POINT ( 'NONE',  ( 3.900000000000000799, 0.000000000000000000, 4.999999999999998224 ) ) ;
#14359 = SURFACE_STYLE_FILL_AREA ( #19893 ) ;
#14360 = CARTESIAN_POINT ( 'NONE',  ( 2.000000000000001332, 9.912500001229034297, -26.53589838486224650 ) ) ;
#14361 = CARTESIAN_POINT ( 'NONE',  ( 12.48750000000000249, -2.886751345948129988, 4.999999999999997335 ) ) ;
#14362 = CARTESIAN_POINT ( 'NONE',  ( 3.999999999999999112, 18.08750000122903501, 30.00000000000000000 ) ) ;
#14363 = CARTESIAN_POINT ( 'NONE',  ( 10.72500000122903252, 2.886751345948126879, 4.999999999999999112 ) ) ;
#14364 = CARTESIAN_POINT ( 'NONE',  ( 22.69687500061451857, -3.027376345333614438, 5.243569643749998122 ) ) ;
#14365 = CARTESIAN_POINT ( 'NONE',  ( 15.53437500061451715, -4.541064518000419881, 2.621784821874995952 ) ) ;
#14366 = LINE ( 'NONE', #59421, #36018 ) ;
#14367 = ORIENTED_EDGE ( 'NONE', *, *, #1615, .T. ) ;
#14368 = CARTESIAN_POINT ( 'NONE',  ( 20.24062500061451431, 6.054752690667223547, 3.707466751127219781E-16 ) ) ;
#14369 = CARTESIAN_POINT ( 'NONE',  ( 3.365625000614516082, -6.054752690667223547, -1.112240025338166033E-15 ) ) ;
#14370 = CARTESIAN_POINT ( 'NONE',  ( 18.23437500061451999, -4.541064518000419881, 2.621784821874995952 ) ) ;
#14371 = CARTESIAN_POINT ( 'NONE',  ( 28.05937500061451573, 0.000000000000000000, 5.243569643749999010 ) ) ;
#14372 = CARTESIAN_POINT ( 'NONE',  ( 3.778125000614519280, -4.541064518000419881, 2.621784821874995952 ) ) ;
#14373 = CARTESIAN_POINT ( 'NONE',  ( 19.71562500061451928, 3.027376345333613106, -5.243569643749998122 ) ) ;
#14374 = CARTESIAN_POINT ( 'NONE',  ( -2.121784821874996840, 15.82812500061451644, 33.67503911421598417 ) ) ;
#14375 = CARTESIAN_POINT ( 'NONE',  ( 15.63750000122903216, 4.330127018922191873, 2.499999999999999556 ) ) ;
#14376 = CARTESIAN_POINT ( 'NONE',  ( 11.78437500061451892, 4.119189519843966529, 2.378215178124999607 ) ) ;
#14377 = CARTESIAN_POINT ( 'NONE',  ( 7.003125000614518036, -4.541064518000417216, -2.621784821875001281 ) ) ;
#14378 = CARTESIAN_POINT ( 'NONE',  ( 29.16562500061451502, 3.027376345333613106, -5.243569643749998122 ) ) ;
#14379 = EDGE_CURVE ( 'NONE', #56216, #61496, #32471, .T. ) ;
#14380 = CARTESIAN_POINT ( 'NONE',  ( 22.69687500061451857, -3.027376345333614438, 5.243569643749998122 ) ) ;
#14381 = CARTESIAN_POINT ( 'NONE',  ( 14.35312500061451679, 4.541064518000418104, -2.621784821874998173 ) ) ;
#14382 = CARTESIAN_POINT ( 'NONE',  ( 25.80000000122903714, -2.886751345948125991, -5.000000000000000000 ) ) ;
#14383 = CARTESIAN_POINT ( 'NONE',  ( 22.34062500061451573, -3.027376345333610441, -5.243569643749999898 ) ) ;
#14384 = CARTESIAN_POINT ( 'NONE',  ( 19.17187500061451999, -6.054752690667223547, -1.112240025338166033E-15 ) ) ;
#14385 = CARTESIAN_POINT ( 'NONE',  ( 15.89062500061451289, -3.027376345333614438, 5.243569643749998122 ) ) ;
#14386 = CARTESIAN_POINT ( 'NONE',  ( -3.000416591977282496E-16, 14.34687500061451715, 25.09994784771203058 ) ) ;
#14387 = CARTESIAN_POINT ( 'NONE',  ( 19.34062500061451573, 6.054752690667223547, 3.707466751127219781E-16 ) ) ;
#14388 = ORIENTED_EDGE ( 'NONE', *, *, #38075, .T. ) ;
#14389 = CARTESIAN_POINT ( 'NONE',  ( 24.07499999999999929, 4.330127018922191873, 2.499999999999999556 ) ) ;
#14390 = CARTESIAN_POINT ( 'NONE',  ( -2.828200636599751609E-16, 11.33750000000000036, -34.61880215351700230 ) ) ;
#14391 = DIRECTION ( 'NONE',  ( -1.000000000000000000, -0.000000000000000000, -0.000000000000000000 ) ) ;
#14392 = CARTESIAN_POINT ( 'NONE',  ( 26.50312500061451360, 4.541064518000418104, -2.621784821874998173 ) ) ;
#14393 = CARTESIAN_POINT ( 'NONE',  ( 7.865625000614516971, -6.054752690667223547, -1.112240025338166033E-15 ) ) ;
#14394 = CARTESIAN_POINT ( 'NONE',  ( 19.23750000122903714, 4.330127018922191873, 2.499999999999999556 ) ) ;
#14395 = CARTESIAN_POINT ( 'NONE',  ( 24.70312500061451644, 4.541064518000418104, -2.621784821874998173 ) ) ;
#14396 = CARTESIAN_POINT ( 'NONE',  ( 22.76249999999999574, 2.886751345948126879, 4.999999999999999112 ) ) ;
#14397 = CARTESIAN_POINT ( 'NONE',  ( 28.22812500061451502, 6.421520780324663323E-16, -5.243569643749999010 ) ) ;
#14398 = CARTESIAN_POINT ( 'NONE',  ( 7.603125000614517681, 4.541064518000418104, -2.621784821874998173 ) ) ;
#14399 = ORIENTED_EDGE ( 'NONE', *, *, #23115, .F. ) ;
#14400 = CARTESIAN_POINT ( 'NONE',  ( 23.76562500061451644, 3.027376345333613106, -5.243569643749998122 ) ) ;
#14401 = CARTESIAN_POINT ( 'NONE',  ( 5.690625000614516260, -3.027376345333610441, -5.243569643749999898 ) ) ;
#14402 = PRODUCT_DEFINITION_CONTEXT ( 'detailed design', #29032, 'design' ) ;
#14403 = CARTESIAN_POINT ( 'NONE',  ( 13.13437500061451857, 4.119189519843966529, 2.378215178124999607 ) ) ;
#14404 = CARTESIAN_POINT ( 'NONE',  ( 3.365625000614516082, -6.054752690667223547, -1.112240025338166033E-15 ) ) ;
#14405 = CARTESIAN_POINT ( 'NONE',  ( -1.999999999999997113, 14.33750000122903323, -26.53589838486224295 ) ) ;
#14406 = CARTESIAN_POINT ( 'NONE',  ( -3.999999999999997335, 10.58750000000000213, -27.69059892324149530 ) ) ;
#14407 = CARTESIAN_POINT ( 'NONE',  ( 9.750000000000001776, 0.000000000000000000, 4.999999999999998224 ) ) ;
#14408 = CARTESIAN_POINT ( 'NONE',  ( 10.62187500061451928, -6.054752690667223547, -1.112240025338166033E-15 ) ) ;
#14409 = CARTESIAN_POINT ( 'NONE',  ( 8.737500001229033586, 6.123233995736764310E-16, -4.999999999999998224 ) ) ;
#14410 = CARTESIAN_POINT ( 'NONE',  ( 15.42187500061451821, 3.027376345333611329, 5.243569643749999010 ) ) ;
#14411 = CARTESIAN_POINT ( 'NONE',  ( 14.55000000000000071, 4.330127018922192761, -2.499999999999997780 ) ) ;
#14412 = CARTESIAN_POINT ( 'NONE',  ( 6.796875000614516438, 6.054752690667223547, 3.707466751127219781E-16 ) ) ;
#14413 = DIRECTION ( 'NONE',  ( 0.000000000000000000, 0.000000000000000000, 1.000000000000000000 ) ) ;
#14414 = CARTESIAN_POINT ( 'NONE',  ( 20.13750000000000639, -2.886751345948130876, 4.999999999999996447 ) ) ;
#14415 = CARTESIAN_POINT ( 'NONE',  ( 13.17187500061451999, 3.027376345333611329, 5.243569643749999010 ) ) ;
#14416 = EDGE_LOOP ( 'NONE', ( #41616, #28618, #5305, #58500 ) ) ;
#14417 = EDGE_CURVE ( 'NONE', #20886, #16658, #4880, .T. ) ;
#14418 = CARTESIAN_POINT ( 'NONE',  ( 22.90312500061451573, 4.541064518000418104, -2.621784821874998173 ) ) ;
#14419 = DIRECTION ( 'NONE',  ( 0.000000000000000000, 0.000000000000000000, 1.000000000000000000 ) ) ;
#14420 = EDGE_CURVE ( 'NONE', #38626, #51755, #37426, .T. ) ;
#14421 = DIRECTION ( 'NONE',  ( -0.000000000000000000, -1.000000000000000000, -0.000000000000000000 ) ) ;
#14422 = CARTESIAN_POINT ( 'NONE',  ( 26.70937500061451431, 0.000000000000000000, 5.243569643749999010 ) ) ;
#14423 = CARTESIAN_POINT ( 'NONE',  ( 4.340625000614515727, -3.027376345333610441, -5.243569643749999898 ) ) ;
#14424 = CARTESIAN_POINT ( 'NONE',  ( 23.59687500061451360, -4.119189519843965641, -2.378215178125001383 ) ) ;
#14425 = CARTESIAN_POINT ( 'NONE',  ( 15.83437500061451608, 4.541064518000418104, 2.621784821874999949 ) ) ;
#14426 = CARTESIAN_POINT ( 'NONE',  ( 8.259375000614515017, -5.492252693125287522, -1.008910452111647106E-15 ) ) ;
#14427 = CARTESIAN_POINT ( 'NONE',  ( 26.40000000122902790, 5.773502691896255534, 3.535250795749688894E-16 ) ) ;
#14428 = CARTESIAN_POINT ( 'NONE',  ( 6.796875000614516438, 6.054752690667223547, 3.707466751127219781E-16 ) ) ;
#14429 = CARTESIAN_POINT ( 'NONE',  ( 16.50937500061451502, -4.541064518000417216, -2.621784821875001281 ) ) ;
#14430 = CARTESIAN_POINT ( 'NONE',  ( 21.44999999999999929, 0.000000000000000000, 4.999999999999998224 ) ) ;
#14431 = CARTESIAN_POINT ( 'NONE',  ( 23.51249999999999574, 2.886751345948129099, -4.999999999999998224 ) ) ;
#14432 = CARTESIAN_POINT ( 'NONE',  ( 3.487500001229035362, 4.330127018922191873, 2.499999999999999556 ) ) ;
#14433 = CARTESIAN_POINT ( 'NONE',  ( 27.27187500061451431, -6.054752690667223547, -1.112240025338166033E-15 ) ) ;
#14434 = CARTESIAN_POINT ( 'NONE',  ( -7.967954043666661671E-16, 14.44062499938548427, 34.33755215474603517 ) ) ;
#14435 = CARTESIAN_POINT ( 'NONE',  ( 10.05000000000000071, 4.330127018922192761, -2.499999999999997780 ) ) ;
#14436 = CARTESIAN_POINT ( 'NONE',  ( 8.474999999999999645, -4.330127018922194537, 2.499999999999995559 ) ) ;
#14437 = CARTESIAN_POINT ( 'NONE',  ( 9.009375000614516793, 2.746126346562643317, 4.756430356249998326 ) ) ;
#14438 = CARTESIAN_POINT ( 'NONE',  ( 21.55312500061451431, 4.541064518000418104, -2.621784821874998173 ) ) ;
#14439 = CARTESIAN_POINT ( 'NONE',  ( 10.87500000000000000, 6.123233995736764310E-16, -4.999999999999998224 ) ) ;
#14440 = CARTESIAN_POINT ( 'NONE',  ( 7.528125000614515727, 6.421520780324663323E-16, -5.243569643749999010 ) ) ;
#14441 = CARTESIAN_POINT ( 'NONE',  ( 19.08750000000000213, 5.773502691896255534, 3.535250795749688894E-16 ) ) ;
#14442 = CARTESIAN_POINT ( 'NONE',  ( 18.25312500061451715, -4.541064518000417216, -2.621784821875001281 ) ) ;
#14443 = CARTESIAN_POINT ( 'NONE',  ( 0.000000000000000000, 20.00000000000000000, -30.00000000000000000 ) ) ;
#14444 = VECTOR ( 'NONE', #16641, 1000.000000000000000 ) ;
#14445 = CARTESIAN_POINT ( 'NONE',  ( 23.96250000122903145, -4.330127018922190985, -2.500000000000001332 ) ) ;
#14446 = CARTESIAN_POINT ( 'NONE',  ( 1.878215178125000495, 19.91562499938548569, 26.74683588394047007 ) ) ;
#14447 = CARTESIAN_POINT ( 'NONE',  ( 3.637500000000001954, -2.886751345948125991, -5.000000000000000000 ) ) ;
#14448 = ORIENTED_EDGE ( 'NONE', *, *, #23321, .T. ) ;
#14449 = CARTESIAN_POINT ( 'NONE',  ( 20.24062500061451431, 6.054752690667223547, 3.707466751127219781E-16 ) ) ;
#14450 = CARTESIAN_POINT ( 'NONE',  ( 26.27812500061451573, -4.541064518000419881, 2.621784821874995952 ) ) ;
#14451 = CARTESIAN_POINT ( 'NONE',  ( 25.35937500061451644, 0.000000000000000000, 5.243569643749999010 ) ) ;
#14452 = CARTESIAN_POINT ( 'NONE',  ( 9.150000000000002132, 4.330127018922192761, -2.499999999999997780 ) ) ;
#14453 = CARTESIAN_POINT ( 'NONE',  ( 12.85312500061451502, -4.541064518000417216, -2.621784821875001281 ) ) ;
#14454 = CARTESIAN_POINT ( 'NONE',  ( 26.01562500061451289, 3.027376345333613106, -5.243569643749998122 ) ) ;
#14455 = CARTESIAN_POINT ( 'NONE',  ( 17.85937500061451999, -4.541064518000417216, -2.621784821875001281 ) ) ;
#14456 = CARTESIAN_POINT ( 'NONE',  ( 9.853125000614516793, 4.541064518000418104, -2.621784821874998173 ) ) ;
#14457 = CARTESIAN_POINT ( 'NONE',  ( 22.83750000000000213, -2.886751345948157965, 4.999999999999948486 ) ) ;
#14458 = CARTESIAN_POINT ( 'NONE',  ( -2.121784821874999949, 11.68437500061451750, 26.32496088578401938 ) ) ;
#14459 = ADVANCED_FACE ( 'NONE', ( #63447 ), #681, .F. ) ;
#14460 = CARTESIAN_POINT ( 'NONE',  ( 23.58750000122903145, 6.123233995736764310E-16, -4.999999999999998224 ) ) ;
#14461 = CARTESIAN_POINT ( 'NONE',  ( 20.44687500061451857, -2.746126346562646425, 4.756430356249996549 ) ) ;
#14462 = CARTESIAN_POINT ( 'NONE',  ( 14.46562500061451573, 3.027376345333611329, 5.243569643749999010 ) ) ;
#14463 = CARTESIAN_POINT ( 'NONE',  ( 10.47187500061451715, 3.027376345333611329, 5.243569643749999010 ) ) ;
#14464 = CARTESIAN_POINT ( 'NONE',  ( 8.746875000614515727, -3.027376345333614438, 5.243569643749998122 ) ) ;
#14465 = ORIENTED_EDGE ( 'NONE', *, *, #31222, .T. ) ;
#14466 = CARTESIAN_POINT ( 'NONE',  ( -3.671862074746357063, 9.302863167343950579, 34.74916175131421170 ) ) ;
#14467 = CARTESIAN_POINT ( 'NONE',  ( 22.34062500061451573, -3.027376345333610441, -5.243569643749999898 ) ) ;
#14468 = CARTESIAN_POINT ( 'NONE',  ( 16.09687500061452070, -3.027376345333610441, -5.243569643749999898 ) ) ;
#14469 = CARTESIAN_POINT ( 'NONE',  ( 21.21562500061451573, 3.027376345333611329, 5.243569643749999010 ) ) ;
#14470 = CARTESIAN_POINT ( 'NONE',  ( -2.828200636599751609E-16, 12.68750000000000000, 25.38119784648299770 ) ) ;
#14471 = CARTESIAN_POINT ( 'NONE',  ( 27.55312500061451786, 0.000000000000000000, 5.243569643749999010 ) ) ;
#14472 = CARTESIAN_POINT ( 'NONE',  ( 7.500000001229034652, 5.773502691896255534, 3.535250795749688894E-16 ) ) ;
#14473 = ORIENTED_EDGE ( 'NONE', *, *, #69351, .T. ) ;
#14474 = CARTESIAN_POINT ( 'NONE',  ( 29.55000000000000071, 0.000000000000000000, 4.999999999999998224 ) ) ;
#14475 = CARTESIAN_POINT ( 'NONE',  ( -3.999999999999997335, 17.33749999999999858, -27.69059892324149175 ) ) ;
#14476 = CARTESIAN_POINT ( 'NONE',  ( 24.93750000122903288, 6.123233995736764310E-16, -4.999999999999998224 ) ) ;
#14477 = CARTESIAN_POINT ( 'NONE',  ( 1.878215178124997609, 14.92812499938548321, 33.25316411605952993 ) ) ;
#14478 = CARTESIAN_POINT ( 'NONE',  ( 7.284375000614518036, 4.541064518000418104, 2.621784821874999949 ) ) ;
#14479 = CARTESIAN_POINT ( 'NONE',  ( 4.368115381025522659, 2.433016238755435268, -4.556724453905077965 ) ) ;
#14480 = CARTESIAN_POINT ( 'NONE',  ( 14.24062500061451608, -3.027376345333610441, -5.243569643749999898 ) ) ;
#14481 = CARTESIAN_POINT ( 'NONE',  ( 9.759375000614516793, -4.541064518000417216, -2.621784821875001281 ) ) ;
#14482 = CARTESIAN_POINT ( 'NONE',  ( 26.73750000122903003, 6.123233995736764310E-16, -4.999999999999998224 ) ) ;
#14483 = CARTESIAN_POINT ( 'NONE',  ( 16.20937500061451786, 4.541064518000418104, -2.621784821874998173 ) ) ;
#14484 = CARTESIAN_POINT ( 'NONE',  ( 5.859375000614519102, 4.541064518000418104, -2.621784821874998173 ) ) ;
#14485 = CARTESIAN_POINT ( 'NONE',  ( 0.000000000000000000, 20.00000000000000000, -33.99999999999999289 ) ) ;
#14486 = CARTESIAN_POINT ( 'NONE',  ( 4.790625000614518569, -3.027376345333610441, -5.243569643749999898 ) ) ;
#14487 = CARTESIAN_POINT ( 'NONE',  ( 15.70312500061451644, 4.541064518000418104, -2.621784821874998173 ) ) ;
#14488 = ORIENTED_EDGE ( 'NONE', *, *, #35039, .F. ) ;
#14489 = CARTESIAN_POINT ( 'NONE',  ( 12.44062500061451537, -3.027376345333610441, -5.243569643749999898 ) ) ;
#14490 = CARTESIAN_POINT ( 'NONE',  ( 5.287500001229035185, 4.330127018922191873, 2.499999999999999556 ) ) ;
#14491 = CARTESIAN_POINT ( 'NONE',  ( 11.20312500061451644, 4.541064518000418104, -2.621784821874998173 ) ) ;
#14492 = CARTESIAN_POINT ( 'NONE',  ( 20.29687500061451644, 5.492252693125287522, 3.363034840372157021E-16 ) ) ;
#14493 = CARTESIAN_POINT ( 'NONE',  ( 9.862500000000000711, -5.773502691896255534, -1.060575238724906372E-15 ) ) ;
#14494 = CARTESIAN_POINT ( 'NONE',  ( 4.387500001229033053, 4.330127018922191873, 2.499999999999999556 ) ) ;
#14495 = CARTESIAN_POINT ( 'NONE',  ( 19.16250000000000142, 2.886751345948126879, 4.999999999999999112 ) ) ;
#14496 =( BOUNDED_CURVE ( )  B_SPLINE_CURVE ( 2, ( #37269, #59791, #53160, #36535, #26187, #25826, #42814 ),
 .UNSPECIFIED., .F., .F. ) 
 B_SPLINE_CURVE_WITH_KNOTS ( ( 3, 2, 2, 3 ),
 ( 0.9900000000000002132, 0.9933333333333334014, 0.9966666666666668117, 1.000000000000000000 ),
 .UNSPECIFIED. ) 
 CURVE ( )  GEOMETRIC_REPRESENTATION_ITEM ( )  RATIONAL_B_SPLINE_CURVE ( ( 0.9999999999999911182, 0.8660254037844475894, 1.000000000000000000, 0.8660254037844387076, 1.000000000000000000, 0.8660254037844387076, 1.000000000000000000 ) ) 
 REPRESENTATION_ITEM ( '' )  );
#14497 = CARTESIAN_POINT ( 'NONE',  ( 15.57187500061451679, -6.054752690667223547, -1.112240025338166033E-15 ) ) ;
#14498 = CARTESIAN_POINT ( 'NONE',  ( 16.91250000122903430, 4.330127018922192761, -2.499999999999997780 ) ) ;
#14499 = CARTESIAN_POINT ( 'NONE',  ( 23.09999999999999787, 4.330127018922192761, -2.499999999999997780 ) ) ;
#14500 = CARTESIAN_POINT ( 'NONE',  ( 4.243569643749999010, 17.81562500061451715, -32.45002607614398471 ) ) ;
#14501 = LINE ( 'NONE', #42585, #35905 ) ;
#14502 = CARTESIAN_POINT ( 'NONE',  ( 4.898587196589411843E-16, 20.00000000000000000, 33.99999999999999289 ) ) ;
#14503 = CARTESIAN_POINT ( 'NONE',  ( 29.80312500061451431, 0.000000000000000000, 5.243569643749999010 ) ) ;
#14504 = CARTESIAN_POINT ( 'NONE',  ( 11.86875000122902790, 2.886751345948073588, -5.000000000000094147 ) ) ;
#14505 = CARTESIAN_POINT ( 'NONE',  ( 3.881554241669678884, -3.151751365348489653, -4.190642664303462439 ) ) ;
#14506 = CARTESIAN_POINT ( 'NONE',  ( 16.69687500061451502, 6.054752690667223547, 3.707466751127219781E-16 ) ) ;
#14507 = EDGE_CURVE ( 'NONE', #30573, #42983, #34271, .T. ) ;
#14508 = CARTESIAN_POINT ( 'NONE',  ( 28.72500000000000142, -4.330127018922194537, 2.499999999999995559 ) ) ;
#14509 = CARTESIAN_POINT ( 'NONE',  ( 12.32812500061451821, -4.541064518000419881, 2.621784821874995952 ) ) ;
#14510 = CARTESIAN_POINT ( 'NONE',  ( 7.931250001229031454, 4.330127018922191873, 2.499999999999999556 ) ) ;
#14511 = CARTESIAN_POINT ( 'NONE',  ( 24.49687500061451573, -3.027376345333614438, 5.243569643749998122 ) ) ;
#14512 = CARTESIAN_POINT ( 'NONE',  ( 15.94687500061451502, -4.119189519843965641, -2.378215178125001383 ) ) ;
#14513 = CARTESIAN_POINT ( 'NONE',  ( 10.34062500061451750, 6.054752690667223547, 3.707466751127219781E-16 ) ) ;
#14514 = CARTESIAN_POINT ( 'NONE',  ( 13.80937500061451750, -4.541064518000417216, -2.621784821875001281 ) ) ;
#14515 = ORIENTED_EDGE ( 'NONE', *, *, #3480, .F. ) ;
#14516 = CARTESIAN_POINT ( 'NONE',  ( 23.14687500061451786, -3.027376345333614438, 5.243569643749998122 ) ) ;
#14517 = CARTESIAN_POINT ( 'NONE',  ( 27.14062500061451644, -3.027376345333614438, 5.243569643749998122 ) ) ;
#14518 = CARTESIAN_POINT ( 'NONE',  ( 4.898587196589412829E-16, 27.50000000000000000, 34.00000000000000000 ) ) ;
#14519 = CARTESIAN_POINT ( 'NONE',  ( 8.437500000000000000, -2.886751345948129988, 4.999999999999997335 ) ) ;
#14520 = CARTESIAN_POINT ( 'NONE',  ( 17.43750000122903288, 4.330127018922191873, 2.499999999999999556 ) ) ;
#14521 = CARTESIAN_POINT ( 'NONE',  ( 16.63125000122903074, -4.330127018922194537, 2.499999999999995559 ) ) ;
#14522 = CARTESIAN_POINT ( 'NONE',  ( 8.821875000614515017, 5.824947211148865298E-16, -4.756430356249998326 ) ) ;
#14523 = ORIENTED_EDGE ( 'NONE', *, *, #70232, .T. ) ;
#14524 = CARTESIAN_POINT ( 'NONE',  ( 15.22500000000000142, -4.330127018922194537, 2.499999999999995559 ) ) ;
#14525 = CARTESIAN_POINT ( 'NONE',  ( 18.45000000000000284, -4.330127018922190985, -2.500000000000001332 ) ) ;
#14526 = CARTESIAN_POINT ( 'NONE',  ( 13.75312500061451715, -4.541064518000417216, -2.621784821875001281 ) ) ;
#14527 = VERTEX_POINT ( 'NONE', #24643 ) ;
#14528 = CARTESIAN_POINT ( 'NONE',  ( 3.999999999999998668, 18.57500000122903216, -32.30940107675850470 ) ) ;
#14529 = CARTESIAN_POINT ( 'NONE',  ( 4.243569643749999010, 17.87187500061451573, -32.45002607614398471 ) ) ;
#14530 = CARTESIAN_POINT ( 'NONE',  ( 29.36250000122903003, -4.330127018922190985, -2.500000000000001332 ) ) ;
#14531 = CARTESIAN_POINT ( 'NONE',  ( -3.756430356250000102, 13.31562499938548427, 30.00000000000000000 ) ) ;
#14532 = CARTESIAN_POINT ( 'NONE',  ( 11.47499999999999964, 4.330127018922191873, 2.499999999999999556 ) ) ;
#14533 = CARTESIAN_POINT ( 'NONE',  ( 27.87187500061451217, 4.119189519843966529, 2.378215178124999607 ) ) ;
#14534 = VERTEX_POINT ( 'NONE', #40933 ) ;
#14535 = CARTESIAN_POINT ( 'NONE',  ( 2.121784821874999061, 15.60312500061451857, 26.32496088578401583 ) ) ;
#14536 = CARTESIAN_POINT ( 'NONE',  ( 27.02812500061451573, 4.541064518000418104, 2.621784821874999949 ) ) ;
#14537 = CARTESIAN_POINT ( 'NONE',  ( -1.878215178125001827, 20.14062499938548356, 33.25316411605952283 ) ) ;
#14538 = CARTESIAN_POINT ( 'NONE',  ( 22.69687500061451857, -3.027376345333614438, 5.243569643749998122 ) ) ;
#14539 = CARTESIAN_POINT ( 'NONE',  ( 20.01562500061451644, -6.054752690667223547, -1.112240025338166033E-15 ) ) ;
#14540 = CARTESIAN_POINT ( 'NONE',  ( 2.121784821875001281, 14.10312500061459318, -26.32496088578401938 ) ) ;
#14541 = CARTESIAN_POINT ( 'NONE',  ( 22.76250000122903216, 4.330127018922192761, -2.499999999999997780 ) ) ;
#14542 = CARTESIAN_POINT ( 'NONE',  ( 4.565625000614516260, 3.027376345333611329, 5.243569643749999010 ) ) ;
#14543 = CARTESIAN_POINT ( 'NONE',  ( 27.04687500061450933, 5.492252693125287522, 3.363034840372157021E-16 ) ) ;
#14544 = CARTESIAN_POINT ( 'NONE',  ( 20.39062500061451644, -3.027376345333614438, 5.243569643749998122 ) ) ;
#14545 = CARTESIAN_POINT ( 'NONE',  ( 9.646875000614516082, -2.746126346562646425, 4.756430356249996549 ) ) ;
#14546 = CARTESIAN_POINT ( 'NONE',  ( -1.878215178124999163, 15.49062499938548321, 26.74683588394047007 ) ) ;
#14547 = CARTESIAN_POINT ( 'NONE',  ( 18.72187500061451360, -6.054752690667223547, -1.112240025338166033E-15 ) ) ;
#14548 = CARTESIAN_POINT ( 'NONE',  ( 17.82187500061451502, -6.054752690667223547, -1.112240025338166033E-15 ) ) ;
#14549 = CARTESIAN_POINT ( 'NONE',  ( 23.63437500061451502, -4.541064518000419881, 2.621784821874995952 ) ) ;
#14550 = CARTESIAN_POINT ( 'NONE',  ( -2.121784821874999949, 13.03437500061451715, 26.32496088578401938 ) ) ;
#14551 = CARTESIAN_POINT ( 'NONE',  ( 6.290625000614517681, 6.054752690667223547, 3.707466751127219781E-16 ) ) ;
#14553 =( BOUNDED_CURVE ( )  B_SPLINE_CURVE ( 2, ( #43432, #32708, #72231, #21610, #15698, #4999, #9802 ),
 .UNSPECIFIED., .F., .F. ) 
 B_SPLINE_CURVE_WITH_KNOTS ( ( 3, 2, 2, 3 ),
 ( 0.5666666666666667629, 0.5694444444444445308, 0.5722222222222221877, 0.5749999999999999556 ),
 .UNSPECIFIED. ) 
 CURVE ( )  GEOMETRIC_REPRESENTATION_ITEM ( )  RATIONAL_B_SPLINE_CURVE ( ( 0.9999999999999946709, 0.8660254037844440367, 1.000000000000000000, 0.8660254037844387076, 1.000000000000000000, 0.8660254037844387076, 1.000000000000000000 ) ) 
 REPRESENTATION_ITEM ( '' )  );
#14552 = CARTESIAN_POINT ( 'NONE',  ( 28.97812500061451502, -4.541064518000419881, 2.621784821874995952 ) ) ;
#14554 = EDGE_CURVE ( 'NONE', #67801, #3601, #34638, .T. ) ;
#14555 = CARTESIAN_POINT ( 'NONE',  ( 28.41562500061451502, 3.027376345333611329, 5.243569643749999010 ) ) ;
#14556 = CARTESIAN_POINT ( 'NONE',  ( 4.167140676845648706, 2.763139261668956514, -4.167140676845877856 ) ) ;
#14557 = DIRECTION ( 'NONE',  ( -0.000000000000000000, -1.000000000000000000, -0.000000000000000000 ) ) ;
#14558 = CARTESIAN_POINT ( 'NONE',  ( 8.146875000614516082, 6.054752690667223547, 3.707466751127219781E-16 ) ) ;
#14559 = CARTESIAN_POINT ( 'NONE',  ( 0.000000000000000000, 0.000000000000000000, 0.000000000000000000 ) ) ;
#14560 = CARTESIAN_POINT ( 'NONE',  ( 14.17500000122903536, 2.886751345948129099, -4.999999999999998224 ) ) ;
#14561 = CARTESIAN_POINT ( 'NONE',  ( 10.50000000122903465, -2.886751345948125991, -5.000000000000000000 ) ) ;
#14562 = CARTESIAN_POINT ( 'NONE',  ( 4.865625000614517859, 3.027376345333613106, -5.243569643749998122 ) ) ;
#14563 = CARTESIAN_POINT ( 'NONE',  ( -4.000000000000000888, 16.30624999877096570, 32.30940107675850470 ) ) ;
#14564 = CARTESIAN_POINT ( 'NONE',  ( 19.89375000122903359, -2.886751345948125991, -5.000000000000000000 ) ) ;
#14565 = CARTESIAN_POINT ( 'NONE',  ( 14.14687500061451786, -3.027376345333614438, 5.243569643749998122 ) ) ;
#14566 = CYLINDRICAL_SURFACE ( 'NONE', #31386, 3.999999999999996447 ) ;
#14567 = ORIENTED_EDGE ( 'NONE', *, *, #43413, .F. ) ;
#14568 = CARTESIAN_POINT ( 'NONE',  ( 22.94062500061451715, 6.054752690667223547, 3.707466751127219781E-16 ) ) ;
#14569 = CARTESIAN_POINT ( 'NONE',  ( 7.415625000614516793, -6.054752690667223547, -1.112240025338166033E-15 ) ) ;
#14570 = CARTESIAN_POINT ( 'NONE',  ( 23.40937500061451715, 4.541064518000418104, -2.621784821874998173 ) ) ;
#14571 = CARTESIAN_POINT ( 'NONE',  ( 8.165625000614516793, 3.027376345333611329, 5.243569643749999010 ) ) ;
#14572 = DIRECTION ( 'NONE',  ( 0.000000000000000000, 0.000000000000000000, 1.000000000000000000 ) ) ;
#14573 = CARTESIAN_POINT ( 'NONE',  ( 8.700000001229032165, -2.886751345948125991, -5.000000000000000000 ) ) ;
#14574 = CARTESIAN_POINT ( 'NONE',  ( 22.86562500061451431, 3.027376345333613106, -5.243569643749998122 ) ) ;
#14575 = CARTESIAN_POINT ( 'NONE',  ( -4.243569643749999898, 10.35312500061451857, -30.00000000000000000 ) ) ;
#14576 = CARTESIAN_POINT ( 'NONE',  ( 10.38750000122903572, -4.330127018922194537, 2.499999999999995559 ) ) ;
#14577 = CARTESIAN_POINT ( 'NONE',  ( 20.87812500061451715, -4.541064518000419881, 2.621784821874995952 ) ) ;
#14578 = CARTESIAN_POINT ( 'NONE',  ( 18.89062500061451644, 6.054752690667223547, 3.707466751127219781E-16 ) ) ;
#14579 = CARTESIAN_POINT ( 'NONE',  ( 27.68437500061451573, -4.119189519843968306, 2.378215178124996054 ) ) ;
#14580 = CARTESIAN_POINT ( 'NONE',  ( 17.32499999999999929, 4.330127018922191873, 2.499999999999999556 ) ) ;
#14581 = CARTESIAN_POINT ( 'NONE',  ( 11.73750000122903181, -4.330127018922194537, 2.499999999999995559 ) ) ;
#14582 = CARTESIAN_POINT ( 'NONE',  ( 11.01562500061451821, -6.054752690667223547, -1.112240025338166033E-15 ) ) ;
#14583 = CARTESIAN_POINT ( 'NONE',  ( 12.44062500061451537, -3.027376345333610441, -5.243569643749999898 ) ) ;
#14584 = CARTESIAN_POINT ( 'NONE',  ( 22.98750000122903003, -4.330127018922194537, 2.499999999999995559 ) ) ;
#14585 = CARTESIAN_POINT ( 'NONE',  ( 20.85937500061451644, 0.000000000000000000, 5.243569643749999010 ) ) ;
#14586 = CARTESIAN_POINT ( 'NONE',  ( 3.575968405063141731, 3.494640511729611099, -3.909292473339659235 ) ) ;
#14587 = CARTESIAN_POINT ( 'NONE',  ( 6.300000001229033586, -2.886751345948129988, 4.999999999999997335 ) ) ;
#14588 = CARTESIAN_POINT ( 'NONE',  ( 6.271875000614517859, 3.027376345333613106, -5.243569643749998122 ) ) ;
#14589 = CARTESIAN_POINT ( 'NONE',  ( 24.42187500061451999, 3.027376345333611329, 5.243569643749999010 ) ) ;
#14590 = CARTESIAN_POINT ( 'NONE',  ( 4.746675283896760078, -1.572051564878419683, 4.883304218962898346 ) ) ;
#14591 = CARTESIAN_POINT ( 'NONE',  ( 19.60312500061451502, -4.541064518000417216, -2.621784821875001281 ) ) ;
#14592 = CARTESIAN_POINT ( 'NONE',  ( 24.64687500061451431, -3.027376345333610441, -5.243569643749999898 ) ) ;
#14593 = CARTESIAN_POINT ( 'NONE',  ( -1.878215178124999163, 20.10312499938548569, 26.74683588394047007 ) ) ;
#14594 = CARTESIAN_POINT ( 'NONE',  ( 23.25000000000000000, 0.000000000000000000, 4.999999999999998224 ) ) ;
#14595 = CARTESIAN_POINT ( 'NONE',  ( 27.86250000122903359, 0.000000000000000000, 4.999999999999998224 ) ) ;
#14596 = CARTESIAN_POINT ( 'NONE',  ( 4.284375000614518925, -4.541064518000419881, 2.621784821874995952 ) ) ;
#14597 = CARTESIAN_POINT ( 'NONE',  ( 16.22812500061451857, 4.541064518000418104, 2.621784821874999949 ) ) ;
#14598 = CARTESIAN_POINT ( 'NONE',  ( 12.68437500061451573, 4.541064518000418104, 2.621784821874999949 ) ) ;
#14599 = ORIENTED_EDGE ( 'NONE', *, *, #36502, .T. ) ;
#14600 = CARTESIAN_POINT ( 'NONE',  ( 2.000000000000001332, 17.00000000000000000, -26.53589838486224650 ) ) ;
#14601 = CARTESIAN_POINT ( 'NONE',  ( 24.06562500061451715, -6.054752690667223547, -1.112240025338166033E-15 ) ) ;
#14602 = CARTESIAN_POINT ( 'NONE',  ( 1.071796769724497445, 17.16740381056766651, 26.00000000000000355 ) ) ;
#14603 = CARTESIAN_POINT ( 'NONE',  ( 25.50000000000000000, 0.000000000000000000, 4.999999999999998224 ) ) ;
#14604 = CARTESIAN_POINT ( 'NONE',  ( 14.73749999999999893, -2.886751345948129988, 4.999999999999997335 ) ) ;
#14605 = CARTESIAN_POINT ( 'NONE',  ( 23.92500000122903359, -5.773502691896255534, -1.060575238724906372E-15 ) ) ;
#14606 = CARTESIAN_POINT ( 'NONE',  ( 17.57812500061451644, 4.541064518000418104, 2.621784821874999949 ) ) ;
#14607 = ORIENTED_EDGE ( 'NONE', *, *, #61749, .F. ) ;
#14608 = CARTESIAN_POINT ( 'NONE',  ( 21.93750000000000000, -2.886751345948129988, 4.999999999999997335 ) ) ;
#14609 = CARTESIAN_POINT ( 'NONE',  ( 23.25937500061451857, -4.541064518000417216, -2.621784821875001281 ) ) ;
#14610 = ORIENTED_EDGE ( 'NONE', *, *, #30034, .F. ) ;
#14611 = CARTESIAN_POINT ( 'NONE',  ( 2.964777361493091679, -4.026176250088806086, -3.359304602455296607 ) ) ;
#14612 = CARTESIAN_POINT ( 'NONE',  ( 12.02812500061451573, 6.421520780324663323E-16, -5.243569643749999010 ) ) ;
#14613 = CARTESIAN_POINT ( 'NONE',  ( 3.365625000614516082, -6.054752690667223547, -1.112240025338166033E-15 ) ) ;
#14614 = CARTESIAN_POINT ( 'NONE',  ( 16.02187500061451431, 5.824947211148865298E-16, -4.756430356249998326 ) ) ;
#14615 = CARTESIAN_POINT ( 'NONE',  ( 27.36562500061451786, 3.027376345333613106, -5.243569643749998122 ) ) ;
#14616 = CARTESIAN_POINT ( 'NONE',  ( 19.83750000000000213, -2.886751345948125991, -5.000000000000000000 ) ) ;
#14617 = CARTESIAN_POINT ( 'NONE',  ( 27.07499999999999929, 6.123233995736764310E-16, -4.999999999999998224 ) ) ;
#14618 = DIRECTION ( 'NONE',  ( 1.000000000000000000, 0.000000000000000000, 0.000000000000000000 ) ) ;
#14619 = CARTESIAN_POINT ( 'NONE',  ( 7.546875000614517326, -3.027376345333610441, -5.243569643749999898 ) ) ;
#14620 = CARTESIAN_POINT ( 'NONE',  ( 18.08437500061451431, 4.541064518000418104, 2.621784821874999949 ) ) ;
#14621 = CARTESIAN_POINT ( 'NONE',  ( -1.999999999999997113, 13.88750000122903394, 33.46410161513775705 ) ) ;
#14622 = ORIENTED_EDGE ( 'NONE', *, *, #1071, .T. ) ;
#14623 = CARTESIAN_POINT ( 'NONE',  ( 27.40312500061451573, 4.541064518000418104, -2.621784821874998173 ) ) ;
#14624 = CARTESIAN_POINT ( 'NONE',  ( 28.80937500061451573, 4.541064518000418104, -2.621784821874998173 ) ) ;
#14625 = CARTESIAN_POINT ( 'NONE',  ( 3.046875000614519990, -3.027376345333610441, -5.243569643749999898 ) ) ;
#14626 = CARTESIAN_POINT ( 'NONE',  ( 16.31250000000000000, 2.886751345948129099, -4.999999999999998224 ) ) ;
#14627 = CARTESIAN_POINT ( 'NONE',  ( 10.56562500061451715, -6.054752690667223547, -1.112240025338166033E-15 ) ) ;
#14628 = LINE ( 'NONE', #37168, #38368 ) ;
#14629 = CARTESIAN_POINT ( 'NONE',  ( 28.45312500061451289, 0.000000000000000000, 5.243569643749999010 ) ) ;
#14630 = CARTESIAN_POINT ( 'NONE',  ( 19.05000000122903359, -2.886751345948125991, -5.000000000000000000 ) ) ;
#14631 = CARTESIAN_POINT ( 'NONE',  ( 3.139915822865742445, -3.891420429212240073, 3.139915822865742445 ) ) ;
#14632 = CARTESIAN_POINT ( 'NONE',  ( 18.30937500061451928, -4.119189519843965641, -2.378215178125001383 ) ) ;
#14633 = CARTESIAN_POINT ( 'NONE',  ( 4.153125000614515727, 0.000000000000000000, 5.243569643749999010 ) ) ;
#14634 = CARTESIAN_POINT ( 'NONE',  ( 22.80937500061451573, -4.541064518000417216, -2.621784821875001281 ) ) ;
#14635 = CARTESIAN_POINT ( 'NONE',  ( 2.121784821874999061, 16.10937500061451644, 26.32496088578401583 ) ) ;
#14636 = CARTESIAN_POINT ( 'NONE',  ( 24.60937500061451644, -4.541064518000417216, -2.621784821875001281 ) ) ;
#14637 = CARTESIAN_POINT ( 'NONE',  ( 5.887500000000000178, -2.886751345948125991, -5.000000000000000000 ) ) ;
#14638 = CARTESIAN_POINT ( 'NONE',  ( 2.000000000000001332, 10.81250000122903465, 33.46410161513774995 ) ) ;
#14639 = CARTESIAN_POINT ( 'NONE',  ( 11.80312500061451608, 0.000000000000000000, 5.243569643749999010 ) ) ;
#14640 = CARTESIAN_POINT ( 'NONE',  ( 4.537500001229034297, -4.330127018922194537, 2.499999999999995559 ) ) ;
#14641 = EDGE_CURVE ( 'NONE', #48464, #15624, #49758, .T. ) ;
#14642 = CARTESIAN_POINT ( 'NONE',  ( 9.234375000614518214, -4.541064518000419881, 2.621784821874995952 ) ) ;
#14643 = FACE_OUTER_BOUND ( 'NONE', #60250, .T. ) ;
#14644 = CARTESIAN_POINT ( 'NONE',  ( 9.815625000614518925, 3.027376345333613106, -5.243569643749998122 ) ) ;
#14645 = CARTESIAN_POINT ( 'NONE',  ( 15.30937500061451750, 4.541064518000418104, -2.621784821874998173 ) ) ;
#14646 = CARTESIAN_POINT ( 'NONE',  ( 21.69375000122902719, -2.886751345948181946, -4.999999999999904077 ) ) ;
#14647 = CARTESIAN_POINT ( 'NONE',  ( 22.20000000122903216, -2.886751345948125991, -5.000000000000000000 ) ) ;
#14648 = CARTESIAN_POINT ( 'NONE',  ( 9.496875000614517504, 6.054752690667223547, 3.707466751127219781E-16 ) ) ;
#14649 = CARTESIAN_POINT ( 'NONE',  ( 12.62812500061451537, 4.541064518000418104, 2.621784821874999949 ) ) ;
#14650 = CARTESIAN_POINT ( 'NONE',  ( 27.95625000122903359, -4.330127018922190985, -2.500000000000001332 ) ) ;
#14651 = CARTESIAN_POINT ( 'NONE',  ( 22.62187500061451573, 3.027376345333611329, 5.243569643749999010 ) ) ;
#14652 = CARTESIAN_POINT ( 'NONE',  ( -3.999999999999997335, 12.05000000122903359, -27.69059892324149530 ) ) ;
#14653 = CARTESIAN_POINT ( 'NONE',  ( 0.000000000000000000, 27.50000000000000000, 30.00000000000000000 ) ) ;
#14654 = CARTESIAN_POINT ( 'NONE',  ( 4.243569643749999898, 14.23437500061451821, -30.00000000000000000 ) ) ;
#14655 = CARTESIAN_POINT ( 'NONE',  ( 16.01250000122903216, 4.330127018922192761, -2.499999999999997780 ) ) ;
#14656 = CARTESIAN_POINT ( 'NONE',  ( 9.946875000614516793, 6.054752690667223547, 3.707466751127219781E-16 ) ) ;
#14657 = CARTESIAN_POINT ( 'NONE',  ( 4.243569643749999010, 16.91562500061451502, -32.45002607614398471 ) ) ;
#14658 = CARTESIAN_POINT ( 'NONE',  ( 17.06250000122903288, 0.000000000000000000, 4.999999999999998224 ) ) ;
#14659 = CARTESIAN_POINT ( 'NONE',  ( 11.87812500061451537, -4.541064518000419881, 2.621784821874995952 ) ) ;
#14660 = VECTOR ( 'NONE', #68814, 1000.000000000000000 ) ;
#14661 = ORIENTED_EDGE ( 'NONE', *, *, #73043, .F. ) ;
#14662 = CARTESIAN_POINT ( 'NONE',  ( 16.61250000000000426, -5.773502691896255534, -1.060575238724906372E-15 ) ) ;
#14663 = CARTESIAN_POINT ( 'NONE',  ( 45.00000000000000000, 0.000000000000000000, 0.000000000000000000 ) ) ;
#14664 = CARTESIAN_POINT ( 'NONE',  ( 9.196875000614518569, -3.027376345333614438, 5.243569643749998122 ) ) ;
#14665 = DIRECTION ( 'NONE',  ( 0.000000000000000000, 0.000000000000000000, -1.000000000000000000 ) ) ;
#14666 = CARTESIAN_POINT ( 'NONE',  ( 12.26250000122903394, -4.330127018922190985, -2.500000000000001332 ) ) ;
#14667 = CARTESIAN_POINT ( 'NONE',  ( 20.92500000122903714, 2.886751345948129099, -4.999999999999998224 ) ) ;
#14668 = CARTESIAN_POINT ( 'NONE',  ( 17.09062500061451573, 6.054752690667223547, 3.707466751127219781E-16 ) ) ;
#14669 = CARTESIAN_POINT ( 'NONE',  ( 21.74062500061451431, -3.027376345333614438, 5.243569643749998122 ) ) ;
#14670 = CARTESIAN_POINT ( 'NONE',  ( 28.68750000122903288, 4.330127018922191873, 2.499999999999999556 ) ) ;
#14671 = CARTESIAN_POINT ( 'NONE',  ( 4.153125000614515727, 0.000000000000000000, 5.243569643749999010 ) ) ;
#14672 = CARTESIAN_POINT ( 'NONE',  ( 24.63749999999999574, -2.886751345948129988, 4.999999999999997335 ) ) ;
#14673 = FACE_OUTER_BOUND ( 'NONE', #10103, .T. ) ;
#14674 = CARTESIAN_POINT ( 'NONE',  ( 29.32499999999999929, 6.123233995736764310E-16, -4.999999999999998224 ) ) ;
#14675 = CARTESIAN_POINT ( 'NONE',  ( 28.58437500061451786, -4.541064518000419881, 2.621784821874995952 ) ) ;
#14676 = CARTESIAN_POINT ( 'NONE',  ( 2.000000000000001332, 12.50000000000000000, -26.53589838486224650 ) ) ;
#14677 = CARTESIAN_POINT ( 'NONE',  ( 2.887500001229035274, 6.123233995736764310E-16, -4.999999999999998224 ) ) ;
#14678 = CARTESIAN_POINT ( 'NONE',  ( 3.149999999999999911, -4.330127018922190985, -2.500000000000001332 ) ) ;
#14679 = EDGE_CURVE ( 'NONE', #68777, #17600, #6210, .T. ) ;
#14680 = FACE_OUTER_BOUND ( 'NONE', #55695, .T. ) ;
#14681 = CARTESIAN_POINT ( 'NONE',  ( 8.259375000614518569, 0.000000000000000000, 5.243569643749999010 ) ) ;
#14682 = CARTESIAN_POINT ( 'NONE',  ( 25.37812500061451715, -4.541064518000419881, 2.621784821874995952 ) ) ;
#14684 = EDGE_CURVE ( 'NONE', #24462, #36109, #11754, .T. ) ;
#14683 = CARTESIAN_POINT ( 'NONE',  ( 9.318750001229034297, 2.886751345948126879, 4.999999999999998224 ) ) ;
#14685 = CARTESIAN_POINT ( 'NONE',  ( 1.071796769724491893, 10.34509619066136921, 33.99999999999999289 ) ) ;
#14686 = FACE_OUTER_BOUND ( 'NONE', #12077, .T. ) ;
#14687 = CARTESIAN_POINT ( 'NONE',  ( 4.621875000614516615, 3.027376345333611329, 5.243569643749999010 ) ) ;
#14688 = CARTESIAN_POINT ( 'NONE',  ( 8.634375000614518569, 4.541064518000418104, 2.621784821874999949 ) ) ;
#14689 = CARTESIAN_POINT ( 'NONE',  ( 4.537500000000000533, -2.886751345948125991, -5.000000000000000000 ) ) ;
#14690 = CARTESIAN_POINT ( 'NONE',  ( 4.243569643749999898, 11.47812500061459495, 30.00000000000000000 ) ) ;
#14692 = EDGE_CURVE ( 'NONE', #54008, #30532, #11971, .T. ) ;
#14691 = CARTESIAN_POINT ( 'NONE',  ( 29.84999999999999787, 4.330127018922192761, -2.499999999999997780 ) ) ;
#14693 = CARTESIAN_POINT ( 'NONE',  ( 3.975000000000002753, -4.330127018922194537, 2.499999999999995559 ) ) ;
#14694 = CARTESIAN_POINT ( 'NONE',  ( 15.23437500061451644, 5.492252693125287522, 3.363034840372157021E-16 ) ) ;
#14695 = VERTEX_POINT ( 'NONE', #30195 ) ;
#14696 = CARTESIAN_POINT ( 'NONE',  ( 20.69062500061451715, 6.054752690667223547, 3.707466751127219781E-16 ) ) ;
#14697 = CARTESIAN_POINT ( 'NONE',  ( 10.37812500061451715, 4.541064518000418104, 2.621784821874999949 ) ) ;
#14698 = CARTESIAN_POINT ( 'NONE',  ( 23.25937500061451502, 2.746126346562645981, -4.756430356249997438 ) ) ;
#14699 = CARTESIAN_POINT ( 'NONE',  ( 7.171875000614517326, 3.027376345333613106, -5.243569643749998122 ) ) ;
#14700 = CARTESIAN_POINT ( 'NONE',  ( 23.73749999999999716, -2.886751345948129988, 4.999999999999997335 ) ) ;
#14701 = CARTESIAN_POINT ( 'NONE',  ( 19.08750000122903145, 6.123233995736764310E-16, -4.999999999999998224 ) ) ;
#14702 = CARTESIAN_POINT ( 'NONE',  ( 28.00312500061451715, 0.000000000000000000, 5.243569643749999010 ) ) ;
#14703 = CARTESIAN_POINT ( 'NONE',  ( 4.898587196589412829E-16, 27.50000000000000000, 34.00000000000000000 ) ) ;
#14704 = CARTESIAN_POINT ( 'NONE',  ( 9.346875000614517148, -3.027376345333610441, -5.243569643749999898 ) ) ;
#14705 = CARTESIAN_POINT ( 'NONE',  ( 14.14687500061451786, -3.027376345333614438, 5.243569643749998122 ) ) ;
#14706 = CARTESIAN_POINT ( 'NONE',  ( 24.75937500061451502, 4.541064518000418104, -2.621784821874998173 ) ) ;
#14707 = EDGE_CURVE ( 'NONE', #59214, #23775, #29110, .T. ) ;
#14708 = CARTESIAN_POINT ( 'NONE',  ( 2.000000000000001332, 18.01250000122903572, -26.53589838486224650 ) ) ;
#14709 = CARTESIAN_POINT ( 'NONE',  ( 13.50000000000000178, -4.330127018922190985, -2.500000000000001332 ) ) ;
#14710 = CARTESIAN_POINT ( 'NONE',  ( 19.39687500061451786, 6.054752690667223547, 3.707466751127219781E-16 ) ) ;
#14711 = AXIS2_PLACEMENT_3D ( 'NONE', #46590, #25505, #43603 ) ;
#14712 = CARTESIAN_POINT ( 'NONE',  ( 10.35937500061451644, 4.541064518000418104, -2.621784821874998173 ) ) ;
#14713 = CARTESIAN_POINT ( 'NONE',  ( 1.878215178125000495, 20.02812499938548285, 26.74683588394047007 ) ) ;
#14714 = CARTESIAN_POINT ( 'NONE',  ( 22.53750000000000142, -2.886751345948125991, -5.000000000000000000 ) ) ;
#14715 = CARTESIAN_POINT ( 'NONE',  ( 4.000000000000000000, 15.19999999999999929, 30.00000000000000000 ) ) ;
#14716 = LINE ( 'NONE', #66063, #899 ) ;
#14717 = CARTESIAN_POINT ( 'NONE',  ( 24.45937500061451786, 0.000000000000000000, 4.756430356249998326 ) ) ;
#14718 = CARTESIAN_POINT ( 'NONE',  ( 11.39062500061451644, -3.027376345333614438, 5.243569643749998122 ) ) ;
#14719 = CARTESIAN_POINT ( 'NONE',  ( 5.325000000000000178, -4.330127018922194537, 2.499999999999995559 ) ) ;
#14720 = FACE_OUTER_BOUND ( 'NONE', #15031, .T. ) ;
#14721 = CARTESIAN_POINT ( 'NONE',  ( 11.96250000000000213, 2.886751345948126879, 4.999999999999999112 ) ) ;
#14722 = CARTESIAN_POINT ( 'NONE',  ( -3.999999999999999112, 17.86250000122903359, 30.00000000000000000 ) ) ;
#14723 = CARTESIAN_POINT ( 'NONE',  ( 11.06250000122903288, 4.330127018922192761, -2.499999999999997780 ) ) ;
#14724 = AXIS2_PLACEMENT_3D ( 'NONE', #27563, #21636, #34172 ) ;
#14725 = CARTESIAN_POINT ( 'NONE',  ( 21.75937500061451502, 0.000000000000000000, 5.243569643749999010 ) ) ;
#14726 = CARTESIAN_POINT ( 'NONE',  ( 16.47187500061452070, -6.054752690667223547, -1.112240025338166033E-15 ) ) ;
#14727 = CARTESIAN_POINT ( 'NONE',  ( 25.29375000122902861, -2.886751345948167735, -4.999999999999927169 ) ) ;
#14728 = VERTEX_POINT ( 'NONE', #35729 ) ;
#14729 = CARTESIAN_POINT ( 'NONE',  ( 17.95312500061451644, 4.541064518000418104, -2.621784821874998173 ) ) ;
#14730 = CARTESIAN_POINT ( 'NONE',  ( 29.66250000122903074, 0.000000000000000000, 4.999999999999998224 ) ) ;
#14731 = CARTESIAN_POINT ( 'NONE',  ( 16.43437500061451573, -4.541064518000419881, 2.621784821874995952 ) ) ;
#14732 = CARTESIAN_POINT ( 'NONE',  ( 28.65937500061451715, -4.541064518000417216, -2.621784821875001281 ) ) ;
#14733 = CARTESIAN_POINT ( 'NONE',  ( 4.265625000614517326, -6.054752690667223547, -1.112240025338166033E-15 ) ) ;
#14734 = CARTESIAN_POINT ( 'NONE',  ( 19.45312500061451644, 0.000000000000000000, 5.243569643749999010 ) ) ;
#14735 = CARTESIAN_POINT ( 'NONE',  ( 28.50937500061451502, 0.000000000000000000, 5.243569643749999010 ) ) ;
#14736 = CARTESIAN_POINT ( 'NONE',  ( 4.243569643749999898, 12.34062500061451750, 32.45002607614398471 ) ) ;
#14737 = CARTESIAN_POINT ( 'NONE',  ( 16.08750000122903501, 4.330127018922191873, 2.499999999999999556 ) ) ;
#14738 = CARTESIAN_POINT ( 'NONE',  ( 9.796875000614518214, -2.746126346562641984, -4.756430356249999214 ) ) ;
#14739 = CARTESIAN_POINT ( 'NONE',  ( 6.665625000614517681, 3.027376345333612662, -5.243569643749998122 ) ) ;
#14740 = CARTESIAN_POINT ( 'NONE',  ( 26.54062500061451146, 6.054752690667223547, 3.707466751127219781E-16 ) ) ;
#14741 = DIRECTION ( 'NONE',  ( 0.000000000000000000, 0.000000000000000000, 1.000000000000000000 ) ) ;
#14742 = CARTESIAN_POINT ( 'NONE',  ( 23.67187500061451999, -6.054752690667223547, -1.112240025338166033E-15 ) ) ;
#14743 = CARTESIAN_POINT ( 'NONE',  ( 14.57812500061451644, -4.541064518000419881, 2.621784821874995952 ) ) ;
#14744 = CARTESIAN_POINT ( 'NONE',  ( 22.61250000122903003, -4.330127018922190985, -2.500000000000001332 ) ) ;
#14745 = CARTESIAN_POINT ( 'NONE',  ( 23.99062500061451786, -3.027376345333614438, 5.243569643749998122 ) ) ;
#14746 = CARTESIAN_POINT ( 'NONE',  ( 19.95937500061451786, 0.000000000000000000, 5.243569643749999010 ) ) ;
#14747 = CARTESIAN_POINT ( 'NONE',  ( 12.81562500061451537, -6.054752690667223547, -1.112240025338166033E-15 ) ) ;
#14748 = CARTESIAN_POINT ( 'NONE',  ( -4.243569643749999898, 15.35937500061451644, 30.00000000000000000 ) ) ;
#14749 = CARTESIAN_POINT ( 'NONE',  ( 18.66562500061451146, -6.054752690667223547, -1.112240025338166033E-15 ) ) ;
#14750 = CARTESIAN_POINT ( 'NONE',  ( 28.79062500061451502, 6.054752690667223547, 3.707466751127219781E-16 ) ) ;
#14751 = ORIENTED_EDGE ( 'NONE', *, *, #37851, .F. ) ;
#14752 = CARTESIAN_POINT ( 'NONE',  ( 22.16250000000000142, 2.886751345948129099, -4.999999999999998224 ) ) ;
#14753 = CARTESIAN_POINT ( 'NONE',  ( 2.121784821874999061, 19.70937500061451786, -33.67503911421598417 ) ) ;
#14754 = CARTESIAN_POINT ( 'NONE',  ( 27.62812500061451360, -4.541064518000419881, 2.621784821874995952 ) ) ;
#14755 = CARTESIAN_POINT ( 'NONE',  ( 4.790625000614518569, -3.027376345333610441, -5.243569643749999898 ) ) ;
#14756 = CARTESIAN_POINT ( 'NONE',  ( 20.70000000122903216, -2.886751345948129988, 4.999999999999997335 ) ) ;
#14757 = CARTESIAN_POINT ( 'NONE',  ( 25.79062500061451502, -3.027376345333614438, 5.243569643749998122 ) ) ;
#14758 = CARTESIAN_POINT ( 'NONE',  ( 23.43750000000000000, -2.886751345948125991, -5.000000000000000000 ) ) ;
#14759 = CARTESIAN_POINT ( 'NONE',  ( 27.66562500061451146, -6.054752690667223547, -1.112240025338166033E-15 ) ) ;
#14760 = CARTESIAN_POINT ( 'NONE',  ( 7.303125000614516082, 0.000000000000000000, 5.243569643749999010 ) ) ;
#14761 = EDGE_LOOP ( 'NONE', ( #54032, #64419, #61101, #22985 ) ) ;
#14762 = CARTESIAN_POINT ( 'NONE',  ( 22.71562500061451573, -6.054752690667223547, -1.112240025338166033E-15 ) ) ;
#14763 = CARTESIAN_POINT ( 'NONE',  ( 5.953125000614519102, 0.000000000000000000, 5.243569643749999010 ) ) ;
#14764 = VECTOR ( 'NONE', #22737, 1000.000000000000000 ) ;
#14765 = CARTESIAN_POINT ( 'NONE',  ( 12.79687500061451821, -2.746126346562646425, 4.756430356249996549 ) ) ;
#14766 = CARTESIAN_POINT ( 'NONE',  ( 4.190625000614518925, -3.027376345333614438, 5.243569643749998122 ) ) ;
#14767 = CARTESIAN_POINT ( 'NONE',  ( 1.999999999999998668, 14.56250000122903288, -33.46410161513775705 ) ) ;
#14768 = CARTESIAN_POINT ( 'NONE',  ( 4.898587196589412829E-16, 27.50000000000000000, 34.00000000000000000 ) ) ;
#14769 = CARTESIAN_POINT ( 'NONE',  ( 11.25000000000000000, -4.330127018922190985, -2.500000000000001332 ) ) ;
#14770 =( BOUNDED_CURVE ( )  B_SPLINE_CURVE ( 2, ( #35868, #12618, #68783, #6355, #52508, #68061, #1550 ),
 .UNSPECIFIED., .F., .F. ) 
 B_SPLINE_CURVE_WITH_KNOTS ( ( 3, 2, 2, 3 ),
 ( 0.7600000000000000089, 0.7633333333333333082, 0.7666666666666668295, 0.7700000000000001288 ),
 .UNSPECIFIED. ) 
 CURVE ( )  GEOMETRIC_REPRESENTATION_ITEM ( )  RATIONAL_B_SPLINE_CURVE ( ( 1.000000000000000000, 0.8660254037844387076, 1.000000000000000000, 0.8660254037844387076, 1.000000000000000000, 0.8660254037844342667, 1.000000000000004441 ) ) 
 REPRESENTATION_ITEM ( '' )  );
#14772 = CARTESIAN_POINT ( 'NONE',  ( 11.37187500061451750, 3.027376345333611329, 5.243569643749999010 ) ) ;
#14771 = AXIS2_PLACEMENT_3D ( 'NONE', #1105, #44361, #16614 ) ;
#14773 = CARTESIAN_POINT ( 'NONE',  ( 7.687500001229033764, -4.330127018922194537, 2.499999999999995559 ) ) ;
#14774 = CARTESIAN_POINT ( 'NONE',  ( 15.12187500061451750, -6.054752690667223547, -1.112240025338166033E-15 ) ) ;
#14775 = CARTESIAN_POINT ( 'NONE',  ( 15.63749999999999751, -2.886751345948129988, 4.999999999999997335 ) ) ;
#14776 = CARTESIAN_POINT ( 'NONE',  ( 5.859375000614519102, 4.541064518000418104, -2.621784821874998173 ) ) ;
#14777 = CARTESIAN_POINT ( 'NONE',  ( 16.76249999999999929, 2.886751345948129099, -4.999999999999997335 ) ) ;
#14778 = VECTOR ( 'NONE', #47212, 1000.000000000000000 ) ;
#14779 = CARTESIAN_POINT ( 'NONE',  ( 0.000000000000000000, 20.00000000000000000, -30.00000000000000000 ) ) ;
#14780 = CARTESIAN_POINT ( 'NONE',  ( 11.89687500061451608, -3.027376345333614438, 5.243569643749998122 ) ) ;
#14781 = CARTESIAN_POINT ( 'NONE',  ( 3.709174336338540989, 3.352913023424228811, 4.031500572517469294 ) ) ;
#14782 = CARTESIAN_POINT ( 'NONE',  ( 21.51562500061451644, 3.027376345333613106, -5.243569643749998122 ) ) ;
#14783 = CARTESIAN_POINT ( 'NONE',  ( 4.000000000000000000, 11.63750000000000284, 32.30940107675849760 ) ) ;
#14784 = CARTESIAN_POINT ( 'NONE',  ( 4.243569643749999010, 18.71562500061459389, 27.54997392385601174 ) ) ;
#14785 = CARTESIAN_POINT ( 'NONE',  ( 25.20937500061451431, 4.541064518000418104, -2.621784821874998173 ) ) ;
#14786 = EDGE_CURVE ( 'NONE', #48144, #66704, #72388, .T. ) ;
#14787 = CARTESIAN_POINT ( 'NONE',  ( 29.69999999999999574, -4.330127018922190985, -2.500000000000001332 ) ) ;
#14788 = CARTESIAN_POINT ( 'NONE',  ( 4.903125000614516615, 4.541064518000418104, -2.621784821874998173 ) ) ;
#14789 = CARTESIAN_POINT ( 'NONE',  ( 23.63437500061451502, -2.746126346562642428, -4.756430356249999214 ) ) ;
#14790 = CARTESIAN_POINT ( 'NONE',  ( 13.13437500061451857, 4.541064518000418104, 2.621784821874999949 ) ) ;
#14791 = CARTESIAN_POINT ( 'NONE',  ( 8.784375000614515372, -2.746126346562641984, -4.756430356249999214 ) ) ;
#14792 = CARTESIAN_POINT ( 'NONE',  ( 27.78750000122903074, 4.330127018922191873, 2.499999999999999556 ) ) ;
#14793 = CARTESIAN_POINT ( 'NONE',  ( 5.109375000614518214, 0.000000000000000000, 5.243569643749999010 ) ) ;
#14794 = CARTESIAN_POINT ( 'NONE',  ( 16.32187500061451502, 3.027376345333611329, 5.243569643749999010 ) ) ;
#14795 = CARTESIAN_POINT ( 'NONE',  ( 25.38749999999999929, 5.773502691896255534, 3.535250795749688894E-16 ) ) ;
#14796 = CARTESIAN_POINT ( 'NONE',  ( 3.900000001229034563, 5.773502691896255534, 3.535250795749688894E-16 ) ) ;
#14797 = CARTESIAN_POINT ( 'NONE',  ( 26.10937500061451644, 4.541064518000418104, -2.621784821874998173 ) ) ;
#14798 = CARTESIAN_POINT ( 'NONE',  ( -3.756430356250001434, 13.91562499938548392, 32.16877607737301048 ) ) ;
#14799 = CARTESIAN_POINT ( 'NONE',  ( 29.66249999999999432, -5.773502691896255534, -1.060575238724906372E-15 ) ) ;
#14800 = CARTESIAN_POINT ( 'NONE',  ( 8.887499999999999289, -2.886751345948129988, 4.999999999999997335 ) ) ;
#14801 = CARTESIAN_POINT ( 'NONE',  ( 9.759375000614516793, 2.746126346562645981, -4.756430356249997438 ) ) ;
#14802 = CARTESIAN_POINT ( 'NONE',  ( 22.94062500061451715, 6.054752690667223547, 3.707466751127219781E-16 ) ) ;
#14803 = CARTESIAN_POINT ( 'NONE',  ( 12.22499999999999964, 6.123233995736764310E-16, -4.999999999999998224 ) ) ;
#14804 = CARTESIAN_POINT ( 'NONE',  ( 5.165625000614518569, -6.054752690667223547, -1.112240025338166033E-15 ) ) ;
#14805 = CARTESIAN_POINT ( 'NONE',  ( 18.97499999999999787, 6.123233995736764310E-16, -4.999999999999998224 ) ) ;
#14806 = CARTESIAN_POINT ( 'NONE',  ( 19.41562500061451146, 3.027376345333611329, 5.243569643749999010 ) ) ;
#14807 = CARTESIAN_POINT ( 'NONE',  ( -1.243387493232115393E-14, 16.60624999877096641, 26.00000000000000000 ) ) ;
#14808 = CARTESIAN_POINT ( 'NONE',  ( 22.72500000122903430, 2.886751345948129099, -4.999999999999998224 ) ) ;
#14809 = CARTESIAN_POINT ( 'NONE',  ( 3.756430356249998770, 18.45312499938548356, 32.16877607737301759 ) ) ;
#14810 = CARTESIAN_POINT ( 'NONE',  ( 3.450000000000001510, 0.000000000000000000, 4.999999999999998224 ) ) ;
#14811 = AXIS2_PLACEMENT_3D ( 'NONE', #64534, #63449, #29471 ) ;
#14812 = EDGE_LOOP ( 'NONE', ( #18218, #23002, #62515, #69440 ) ) ;
#14813 = CARTESIAN_POINT ( 'NONE',  ( 20.35312500061451502, 0.000000000000000000, 5.243569643749999010 ) ) ;
#14814 = CARTESIAN_POINT ( 'NONE',  ( 24.14062500061451289, -3.027376345333610441, -5.243569643749999898 ) ) ;
#14815 = CARTESIAN_POINT ( 'NONE',  ( 24.94687500061451502, -3.027376345333614438, 5.243569643749998122 ) ) ;
#14816 = CARTESIAN_POINT ( 'NONE',  ( 8.400000000000000355, 0.000000000000000000, 4.999999999999998224 ) ) ;
#14817 = CARTESIAN_POINT ( 'NONE',  ( 11.99062500061451608, -3.027376345333610441, -5.243569643749999898 ) ) ;
#14818 = CARTESIAN_POINT ( 'NONE',  ( 25.86562500061451431, -6.054752690667223547, -1.112240025338166033E-15 ) ) ;
#14819 = CARTESIAN_POINT ( 'NONE',  ( 17.55937500061451573, 4.541064518000418104, -2.621784821874998173 ) ) ;
#14820 = CARTESIAN_POINT ( 'NONE',  ( 8.053125000614516082, 4.541064518000418104, -2.621784821874998173 ) ) ;
#14821 = CARTESIAN_POINT ( 'NONE',  ( 2.923357432354301455, -4.056350739605543154, 3.322806236625610588 ) ) ;
#14822 = CARTESIAN_POINT ( 'NONE',  ( -1.473776270879187500, 9.872922227264545825, 25.95083297442941017 ) ) ;
#14823 = ADVANCED_FACE ( 'NONE', ( #47188 ), #12410, .T. ) ;
#14824 = CARTESIAN_POINT ( 'NONE',  ( 23.66250000122903430, 4.330127018922192761, -2.499999999999997780 ) ) ;
#14825 = CARTESIAN_POINT ( 'NONE',  ( 20.59687500061451715, -2.746126346562641984, -4.756430356249999214 ) ) ;
#14826 = CARTESIAN_POINT ( 'NONE',  ( 15.21562500061451750, 3.027376345333612662, -5.243569643749998122 ) ) ;
#14827 = CARTESIAN_POINT ( 'NONE',  ( 8.634375000614518569, 4.541064518000418104, 2.621784821874999949 ) ) ;
#14828 = CARTESIAN_POINT ( 'NONE',  ( 7.284375000614518036, 4.541064518000418104, 2.621784821874999949 ) ) ;
#14829 = VERTEX_POINT ( 'NONE', #53691 ) ;
#14830 = CARTESIAN_POINT ( 'NONE',  ( -3.517994946560660807, 9.362281625417800512, 34.86422368405397521 ) ) ;
#14831 = CARTESIAN_POINT ( 'NONE',  ( 22.90312500061451573, 4.541064518000418104, -2.621784821874998173 ) ) ;
#14832 = AXIS2_PLACEMENT_3D ( 'NONE', #42602, #37051, #71412 ) ;
#14833 = CARTESIAN_POINT ( 'NONE',  ( 16.02187500061451786, -6.054752690667223547, -1.112240025338166033E-15 ) ) ;
#14834 = CARTESIAN_POINT ( 'NONE',  ( 21.92812500061451431, 6.421520780324663323E-16, -5.243569643749999010 ) ) ;
#14835 = CARTESIAN_POINT ( 'NONE',  ( 1.999999999999998668, 12.65000000000000213, 26.53589838486224650 ) ) ;
#14836 = CARTESIAN_POINT ( 'NONE',  ( 26.35312500061451857, -4.541064518000417216, -2.621784821875001281 ) ) ;
#14837 = CARTESIAN_POINT ( 'NONE',  ( 7.312500001229033764, -4.330127018922190985, -2.500000000000001332 ) ) ;
#14838 = VECTOR ( 'NONE', #42080, 1000.000000000000000 ) ;
#14839 = VERTEX_POINT ( 'NONE', #3085 ) ;
#14840 = CARTESIAN_POINT ( 'NONE',  ( 29.43750000000000000, 5.773502691896255534, 3.535250795749688894E-16 ) ) ;
#14841 = CARTESIAN_POINT ( 'NONE',  ( -1.999999999999997113, 17.82499999999999929, -26.53589838486224295 ) ) ;
#14842 = CARTESIAN_POINT ( 'NONE',  ( 25.65000000122903145, -2.886751345948129988, 4.999999999999997335 ) ) ;
#14843 = CARTESIAN_POINT ( 'NONE',  ( -1.878215178125001827, 16.20312499938548356, 33.25316411605952283 ) ) ;
#14844 = CARTESIAN_POINT ( 'NONE',  ( 7.209375000614519635, 4.541064518000418104, -2.621784821874998173 ) ) ;
#14845 = CARTESIAN_POINT ( 'NONE',  ( 30.00000000000000000, 0.000000000000000000, 4.999999999999998224 ) ) ;
#14846 = ADVANCED_FACE ( 'NONE', ( #70676 ), #65131, .F. ) ;
#14847 = CARTESIAN_POINT ( 'NONE',  ( 15.96562500061451573, -6.054752690667223547, -1.112240025338166033E-15 ) ) ;
#14848 = CARTESIAN_POINT ( 'NONE',  ( 7.884375000614517681, -4.541064518000419881, 2.621784821874995952 ) ) ;
#14849 = CARTESIAN_POINT ( 'NONE',  ( 27.37500000122903288, 2.886751345948126879, 4.999999999999999112 ) ) ;
#14850 = CARTESIAN_POINT ( 'NONE',  ( 18.38437500061451857, 6.421520780324663323E-16, -5.243569643749999010 ) ) ;
#14851 = CARTESIAN_POINT ( 'NONE',  ( 4.771875000614516971, -6.054752690667223547, -1.112240025338166033E-15 ) ) ;
#14852 = CARTESIAN_POINT ( 'NONE',  ( 7.875000001229034652, 2.886751345948129099, -4.999999999999997335 ) ) ;
#14853 = CARTESIAN_POINT ( 'NONE',  ( 6.403125000614517504, 0.000000000000000000, 5.243569643749999010 ) ) ;
#14854 = CARTESIAN_POINT ( 'NONE',  ( 15.66562500061451857, 3.027376345333613106, -5.243569643749998122 ) ) ;
#14855 = ORIENTED_EDGE ( 'NONE', *, *, #17032, .F. ) ;
#14856 = CARTESIAN_POINT ( 'NONE',  ( 13.52812500061451750, 4.541064518000418104, 2.621784821874999949 ) ) ;
#14857 = CARTESIAN_POINT ( 'NONE',  ( 5.812500001229035540, 0.000000000000000000, 4.999999999999998224 ) ) ;
#14858 = CARTESIAN_POINT ( 'NONE',  ( 8.353125000614518569, -4.541064518000417216, -2.621784821875001281 ) ) ;
#14859 = CARTESIAN_POINT ( 'NONE',  ( 20.89687500061452141, -2.746126346562646425, 4.756430356249996549 ) ) ;
#14860 = CARTESIAN_POINT ( 'NONE',  ( 11.43750000000000000, 5.773502691896255534, 3.535250795749688894E-16 ) ) ;
#14861 = CARTESIAN_POINT ( 'NONE',  ( 4.200000001229033053, -2.886751345948125991, -5.000000000000000000 ) ) ;
#14862 = CARTESIAN_POINT ( 'NONE',  ( 18.41250000000000142, -5.773502691896255534, -1.060575238724906372E-15 ) ) ;
#14863 = CARTESIAN_POINT ( 'NONE',  ( 19.24687500061452283, -3.027376345333610441, -5.243569643749999898 ) ) ;
#14864 = CARTESIAN_POINT ( 'NONE',  ( 16.05000000122903359, 5.773502691896255534, 3.535250795749688894E-16 ) ) ;
#14865 = CARTESIAN_POINT ( 'NONE',  ( 21.22500000000000142, 6.123233995736764310E-16, -4.999999999999998224 ) ) ;
#14866 = CIRCLE ( 'NONE', #39687, 1.500000000000000444 ) ;
#14867 = CARTESIAN_POINT ( 'NONE',  ( -4.243569643749999898, 15.71562500061451573, -32.45002607614398471 ) ) ;
#14868 = CARTESIAN_POINT ( 'NONE',  ( -1.487416814333745711E-14, 16.62500000122903288, -26.00000000000000000 ) ) ;
#14869 = CARTESIAN_POINT ( 'NONE',  ( 1.071796769724488785, 15.95134618820330097, 34.00000000000000000 ) ) ;
#14870 = CARTESIAN_POINT ( 'NONE',  ( 30.00000000000000000, 0.000000000000000000, 4.999999999999998224 ) ) ;
#14871 = CARTESIAN_POINT ( 'NONE',  ( 28.52812500061451573, -4.541064518000419881, 2.621784821874995952 ) ) ;
#14872 = SURFACE_STYLE_FILL_AREA ( #15962 ) ;
#14873 = CARTESIAN_POINT ( 'NONE',  ( 15.68437500061451573, 6.421520780324663323E-16, -5.243569643749999010 ) ) ;
#14874 = EDGE_CURVE ( 'NONE', #55745, #67926, #14889, .T. ) ;
#14875 = CARTESIAN_POINT ( 'NONE',  ( 28.87499999999999645, 6.123233995736764310E-16, -4.999999999999998224 ) ) ;
#14876 = CARTESIAN_POINT ( 'NONE',  ( 10.82812500061451644, 4.541064518000418104, 2.621784821874999949 ) ) ;
#14877 = CARTESIAN_POINT ( 'NONE',  ( 7.443750001229033408, 5.773502691896255534, 3.535250795749688894E-16 ) ) ;
#14878 = CARTESIAN_POINT ( 'NONE',  ( 25.02187500061451431, -6.054752690667223547, -1.112240025338166033E-15 ) ) ;
#14879 = CARTESIAN_POINT ( 'NONE',  ( 16.84687500061451715, -4.119189519843965641, -2.378215178125001383 ) ) ;
#14880 = CARTESIAN_POINT ( 'NONE',  ( 6.965625000614518392, -6.054752690667223547, -1.112240025338166033E-15 ) ) ;
#14881 = CARTESIAN_POINT ( 'NONE',  ( 13.28437500061451715, -4.541064518000419881, 2.621784821874995952 ) ) ;
#14882 = ORIENTED_EDGE ( 'NONE', *, *, #58832, .F. ) ;
#14883 = CARTESIAN_POINT ( 'NONE',  ( 22.99687500061451573, 6.054752690667223547, 3.707466751127219781E-16 ) ) ;
#14884 = CARTESIAN_POINT ( 'NONE',  ( 27.81562500061452070, 3.027376345333613106, -5.243569643749998122 ) ) ;
#14885 = CARTESIAN_POINT ( 'NONE',  ( 25.94999999999999929, 0.000000000000000000, 4.999999999999998224 ) ) ;
#14886 = CARTESIAN_POINT ( 'NONE',  ( 6.975000000000002309, 4.330127018922191873, 2.499999999999999556 ) ) ;
#14887 = CARTESIAN_POINT ( 'NONE',  ( 15.82500000122903216, -5.773502691896255534, -1.060575238724906372E-15 ) ) ;
#14888 = LINE ( 'NONE', #64766, #32510 ) ;
#14889 = LINE ( 'NONE', #37429, #13792 ) ;
#14890 = VERTEX_POINT ( 'NONE', #28526 ) ;
#14891 = CARTESIAN_POINT ( 'NONE',  ( 16.05000000000000071, 0.000000000000000000, 4.999999999999998224 ) ) ;
#14892 = CARTESIAN_POINT ( 'NONE',  ( 18.03749999999999787, -2.886751345948125991, -5.000000000000000000 ) ) ;
#14893 = CARTESIAN_POINT ( 'NONE',  ( 11.57812500061451644, 6.421520780324663323E-16, -5.243569643749999010 ) ) ;
#14894 = ORIENTED_EDGE ( 'NONE', *, *, #57289, .F. ) ;
#14895 = DIRECTION ( 'NONE',  ( -1.000000000000000000, -0.000000000000000000, -0.000000000000000000 ) ) ;
#14896 = CARTESIAN_POINT ( 'NONE',  ( -4.243569643749997233, 17.64687500061452141, -27.54997392385601174 ) ) ;
#14897 = CARTESIAN_POINT ( 'NONE',  ( 4.190625000614518925, -3.027376345333614438, 5.243569643749998122 ) ) ;
#14898 = CARTESIAN_POINT ( 'NONE',  ( 1.878215178124997609, 13.46562499938548285, 33.25316411605952993 ) ) ;
#14899 = CARTESIAN_POINT ( 'NONE',  ( 8.849999999999999645, 0.000000000000000000, 4.999999999999998224 ) ) ;
#14900 = CARTESIAN_POINT ( 'NONE',  ( 16.29375000122903216, -2.886751345948126435, -5.000000000000000000 ) ) ;
#14901 = ORIENTED_EDGE ( 'NONE', *, *, #31908, .F. ) ;
#14902 = CARTESIAN_POINT ( 'NONE',  ( -4.243569643749999898, 14.36562500061451786, 27.54997392385601529 ) ) ;
#14903 = CARTESIAN_POINT ( 'NONE',  ( 27.44062500061451715, 6.054752690667223547, 3.707466751127219781E-16 ) ) ;
#14904 = CARTESIAN_POINT ( 'NONE',  ( 29.25000000122903288, -2.886751345948150860, 4.999999999999960920 ) ) ;
#14905 = CARTESIAN_POINT ( 'NONE',  ( -1.878215178124999163, 19.99062499938548143, 26.74683588394047007 ) ) ;
#14906 = CARTESIAN_POINT ( 'NONE',  ( 24.60937500061451644, -4.541064518000417216, -2.621784821875001281 ) ) ;
#14907 = CARTESIAN_POINT ( 'NONE',  ( 19.22812500061451502, 6.421520780324663323E-16, -5.243569643749999010 ) ) ;
#14908 = CARTESIAN_POINT ( 'NONE',  ( 2.121784821874999061, 12.90312500061459389, -33.67503911421598417 ) ) ;
#14909 = CARTESIAN_POINT ( 'NONE',  ( 22.68750000122903288, 6.123233995736764310E-16, -4.999999999999998224 ) ) ;
#14910 = CARTESIAN_POINT ( 'NONE',  ( 4.828125000614518214, 6.421520780324663323E-16, -5.243569643749999010 ) ) ;
#14911 = CARTESIAN_POINT ( 'NONE',  ( 25.95937500061451431, -4.119189519843965641, -2.378215178125001383 ) ) ;
#14912 = CARTESIAN_POINT ( 'NONE',  ( 20.69062500061451715, 6.054752690667223547, 3.707466751127219781E-16 ) ) ;
#14913 = CARTESIAN_POINT ( 'NONE',  ( 8.296875000614516438, -2.746126346562646425, 4.756430356249996549 ) ) ;
#14914 = CARTESIAN_POINT ( 'NONE',  ( -3.756430356250000102, 16.91562499938548214, 30.00000000000000000 ) ) ;
#14915 = CARTESIAN_POINT ( 'NONE',  ( 14.40937500061451715, 4.541064518000418104, -2.621784821874998173 ) ) ;
#14916 = CARTESIAN_POINT ( 'NONE',  ( 16.65937500061452070, 4.541064518000418104, -2.621784821874998173 ) ) ;
#14917 = CARTESIAN_POINT ( 'NONE',  ( 25.80937500061451928, 0.000000000000000000, 5.243569643749999010 ) ) ;
#14918 = CARTESIAN_POINT ( 'NONE',  ( -4.243569643749999898, 13.52187500061451786, 27.54997392385601529 ) ) ;
#14919 = CARTESIAN_POINT ( 'NONE',  ( 5.690625000614516260, -3.027376345333610441, -5.243569643749999898 ) ) ;
#14920 = CARTESIAN_POINT ( 'NONE',  ( 28.41562500061451502, 3.027376345333611329, 5.243569643749999010 ) ) ;
#14921 = CARTESIAN_POINT ( 'NONE',  ( 2.859375000614519546, 0.000000000000000000, 5.243569643749999010 ) ) ;
#14922 = LINE ( 'NONE', #55555, #33293 ) ;
#14923 = CARTESIAN_POINT ( 'NONE',  ( 3.999999999999999112, 18.87500000000000000, 30.00000000000000000 ) ) ;
#14924 = AXIS2_PLACEMENT_3D ( 'NONE', #17751, #11870, #34391 ) ;
#14925 = CARTESIAN_POINT ( 'NONE',  ( 6.571875000614517681, -6.054752690667223547, -1.112240025338166033E-15 ) ) ;
#14926 = DIRECTION ( 'NONE',  ( 0.000000000000000000, 0.000000000000000000, 1.000000000000000000 ) ) ;
#14927 = CARTESIAN_POINT ( 'NONE',  ( 14.66250000122903252, 4.330127018922192761, -2.499999999999997780 ) ) ;
#14928 = CARTESIAN_POINT ( 'NONE',  ( 9.487500001229033586, -4.330127018922194537, 2.499999999999995559 ) ) ;
#14929 = CARTESIAN_POINT ( 'NONE',  ( 4.903125000614516615, 4.541064518000418104, -2.621784821874998173 ) ) ;
#14930 = CARTESIAN_POINT ( 'NONE',  ( -4.000000000000000888, 15.85624999877096641, 32.30940107675850470 ) ) ;
#14931 = CARTESIAN_POINT ( 'NONE',  ( 21.13125000122903074, -4.330127018922194537, 2.499999999999995559 ) ) ;
#14932 = CARTESIAN_POINT ( 'NONE',  ( 14.74687500061451573, -3.027376345333610441, -5.243569643749999898 ) ) ;
#14933 = CARTESIAN_POINT ( 'NONE',  ( 11.92500000000000071, 4.330127018922191873, 2.499999999999999556 ) ) ;
#14934 = EDGE_LOOP ( 'NONE', ( #31733, #59918, #13812 ) ) ;
#14935 = EDGE_CURVE ( 'NONE', #44045, #2558, #14334, .T. ) ;
#14936 = CARTESIAN_POINT ( 'NONE',  ( 21.77812500061451928, -4.541064518000419881, 2.621784821874995952 ) ) ;
#14937 = CARTESIAN_POINT ( 'NONE',  ( 6.403125000614517504, 0.000000000000000000, 5.243569643749999010 ) ) ;
#14938 = CARTESIAN_POINT ( 'NONE',  ( 24.23437500061451644, 6.421520780324663323E-16, -5.243569643749999010 ) ) ;
#14939 = CARTESIAN_POINT ( 'NONE',  ( 7.003125000614518036, -4.541064518000417216, -2.621784821875001281 ) ) ;
#14940 = DIRECTION ( 'NONE',  ( 0.000000000000000000, 0.000000000000000000, -1.000000000000000000 ) ) ;
#14941 =( BOUNDED_CURVE ( )  B_SPLINE_CURVE ( 2, ( #61661, #11061, #33587, #6246, #67589, #68675, #34307, #45777, #56840 ),
 .UNSPECIFIED., .F., .F. ) 
 B_SPLINE_CURVE_WITH_KNOTS ( ( 3, 2, 2, 2, 3 ),
 ( 0.2717391304347826497, 0.2753623188405797118, 0.2826086956521738913, 0.2898550724637681264, 0.2934782608695652439 ),
 .UNSPECIFIED. ) 
 CURVE ( )  GEOMETRIC_REPRESENTATION_ITEM ( )  RATIONAL_B_SPLINE_CURVE ( ( 0.9330127018922194093, 0.9330127018922198534, 1.000000000000000000, 0.8660254037844387076, 1.000000000000000000, 0.8660254037844387076, 1.000000000000000000, 0.9330127018922188542, 0.9330127018922194093 ) ) 
 REPRESENTATION_ITEM ( '' )  );
#14942 = CARTESIAN_POINT ( 'NONE',  ( 7.387500001229032165, 6.123233995736764310E-16, -4.999999999999998224 ) ) ;
#14943 = CARTESIAN_POINT ( 'NONE',  ( 21.44062500061452070, -3.027376345333610441, -5.243569643749999898 ) ) ;
#14944 = CARTESIAN_POINT ( 'NONE',  ( 2.121784821875001281, 10.95312500061451821, -26.32496088578401938 ) ) ;
#14945 = CARTESIAN_POINT ( 'NONE',  ( 10.80000000122903536, -2.886751345948129988, 4.999999999999997335 ) ) ;
#14946 = CARTESIAN_POINT ( 'NONE',  ( 20.54062500061451502, -3.027376345333610441, -5.243569643749999898 ) ) ;
#14947 = CARTESIAN_POINT ( 'NONE',  ( 16.82812500061451644, -4.541064518000419881, 2.621784821874995952 ) ) ;
#14948 = CARTESIAN_POINT ( 'NONE',  ( 28.88437500061451502, 4.119189519843966529, 2.378215178124999607 ) ) ;
#14949 = CARTESIAN_POINT ( 'NONE',  ( 17.92500000000000071, -4.330127018922194537, 2.499999999999995559 ) ) ;
#14950 = CARTESIAN_POINT ( 'NONE',  ( 11.25000000122903288, -2.886751345948129988, 4.999999999999997335 ) ) ;
#14951 = CARTESIAN_POINT ( 'NONE',  ( 7.865625000614516971, -6.054752690667223547, -1.112240025338166033E-15 ) ) ;
#14952 = CARTESIAN_POINT ( 'NONE',  ( 10.41562500061451679, 3.027376345333611329, 5.243569643749999010 ) ) ;
#14953 = CARTESIAN_POINT ( 'NONE',  ( 22.42500000122903359, 2.886751345948126879, 4.999999999999999112 ) ) ;
#14954 = CARTESIAN_POINT ( 'NONE',  ( 22.43437500061451573, 6.421520780324663323E-16, -5.243569643749999010 ) ) ;
#14955 = CARTESIAN_POINT ( 'NONE',  ( 4.809916128174254624, -1.365542690628744449, -5.062639209831853115 ) ) ;
#14956 = CARTESIAN_POINT ( 'NONE',  ( 4.950000001229033941, -2.886751345948129988, 4.999999999999997335 ) ) ;
#14957 = CARTESIAN_POINT ( 'NONE',  ( 5.971875000614516260, 3.027376345333611329, 5.243569643749999010 ) ) ;
#14958 = CARTESIAN_POINT ( 'NONE',  ( 22.65937500061451715, 0.000000000000000000, 5.243569643749999010 ) ) ;
#14959 = EDGE_CURVE ( 'NONE', #65447, #12584, #462, .T. ) ;
#14960 = CARTESIAN_POINT ( 'NONE',  ( 4.518533959972518943, 2.140970262095818200, -4.684411254032723626 ) ) ;
#14961 = CARTESIAN_POINT ( 'NONE',  ( 19.41562500061451146, 3.027376345333611329, 5.243569643749999010 ) ) ;
#14962 = CARTESIAN_POINT ( 'NONE',  ( 23.85937500061451644, 4.541064518000418104, -2.621784821874998173 ) ) ;
#14963 = CARTESIAN_POINT ( 'NONE',  ( 3.756430356249998770, 18.56562499938548427, 32.16877607737301759 ) ) ;
#14964 = CARTESIAN_POINT ( 'NONE',  ( 3.242103837493086330E-14, 11.00000000122903288, -34.00000000000000000 ) ) ;
#14965 = LINE ( 'NONE', #41589, #26542 ) ;
#14966 = CARTESIAN_POINT ( 'NONE',  ( 5.146875000614517859, -3.027376345333614438, 5.243569643749998122 ) ) ;
#14967 = CARTESIAN_POINT ( 'NONE',  ( 15.77812500061451573, 4.541064518000418104, 2.621784821874999949 ) ) ;
#14968 = CARTESIAN_POINT ( 'NONE',  ( 12.98437500061451821, 6.421520780324663323E-16, -5.243569643749999010 ) ) ;
#14969 = VERTEX_POINT ( 'NONE', #55160 ) ;
#14970 = CARTESIAN_POINT ( 'NONE',  ( 9.262499999999997513, 2.886751345948193936, 4.999999999999883649 ) ) ;
#14971 = CARTESIAN_POINT ( 'NONE',  ( 26.27812500061451573, -4.541064518000419881, 2.621784821874995952 ) ) ;
#14972 = CARTESIAN_POINT ( 'NONE',  ( 3.489066138150112018, 3.581398816609729252, -3.723603497192741862 ) ) ;
#14973 = CARTESIAN_POINT ( 'NONE',  ( -2.000000000000001776, 20.44999999999999929, 33.46410161513775705 ) ) ;
#14974 = CARTESIAN_POINT ( 'NONE',  ( 14.36249999999999893, -5.773502691896255534, -1.060575238724906372E-15 ) ) ;
#14975 = CARTESIAN_POINT ( 'NONE',  ( 24.67500000122903359, 2.886751345948126879, 4.999999999999999112 ) ) ;
#14976 = CARTESIAN_POINT ( 'NONE',  ( 18.14062500061451644, -3.027376345333614438, 5.243569643749998122 ) ) ;
#14977 = ORIENTED_EDGE ( 'NONE', *, *, #54670, .T. ) ;
#14978 = CARTESIAN_POINT ( 'NONE',  ( 21.41250000000000497, 2.886751345948126879, 4.999999999999999112 ) ) ;
#14979 =( BOUNDED_CURVE ( )  B_SPLINE_CURVE ( 2, ( #42068, #70505, #66055, #60135, #31347, #48345, #15076 ),
 .UNSPECIFIED., .F., .F. ) 
 B_SPLINE_CURVE_WITH_KNOTS ( ( 3, 2, 2, 3 ),
 ( 0.7750000000000001332, 0.7777777777777779011, 0.7805555555555556690, 0.7833333333333334370 ),
 .UNSPECIFIED. ) 
 CURVE ( )  GEOMETRIC_REPRESENTATION_ITEM ( )  RATIONAL_B_SPLINE_CURVE ( ( 0.9999999999999946709, 0.8660254037844440367, 1.000000000000000000, 0.8660254037844387076, 1.000000000000000000, 0.8660254037844333785, 1.000000000000005329 ) ) 
 REPRESENTATION_ITEM ( '' )  );
#14980 = CARTESIAN_POINT ( 'NONE',  ( 24.12187500061451217, -6.054752690667223547, -1.112240025338166033E-15 ) ) ;
#14981 = ORIENTED_EDGE ( 'NONE', *, *, #42052, .T. ) ;
#14982 = CARTESIAN_POINT ( 'NONE',  ( 11.20312500061451644, 4.541064518000418104, -2.621784821874998173 ) ) ;
#14983 = CARTESIAN_POINT ( 'NONE',  ( 4.115625000614516082, 3.027376345333611329, 5.243569643749999010 ) ) ;
#14984 = CARTESIAN_POINT ( 'NONE',  ( 13.92187500061451644, 4.119189519843966529, 2.378215178124999607 ) ) ;
#14985 = CARTESIAN_POINT ( 'NONE',  ( 26.87812500061451360, 6.421520780324663323E-16, -5.243569643749999010 ) ) ;
#14986 = CARTESIAN_POINT ( 'NONE',  ( 17.02499999999999858, -4.330127018922194537, 2.499999999999995559 ) ) ;
#14987 = CARTESIAN_POINT ( 'NONE',  ( 26.09999999999999787, -4.330127018922190985, -2.500000000000001332 ) ) ;
#14988 = DIRECTION ( 'NONE',  ( 1.000000000000000000, 0.000000000000000000, 0.000000000000000000 ) ) ;
#14989 = CARTESIAN_POINT ( 'NONE',  ( 7.021875000614518747, -6.054752690667223547, -1.112240025338166033E-15 ) ) ;
#14990 = CARTESIAN_POINT ( 'NONE',  ( 17.89687500061451431, -3.027376345333610441, -5.243569643749999898 ) ) ;
#14991 = CARTESIAN_POINT ( 'NONE',  ( 29.85937500061451644, 0.000000000000000000, 5.243569643749999010 ) ) ;
#14992 = VERTEX_POINT ( 'NONE', #49980 ) ;
#14993 = CARTESIAN_POINT ( 'NONE',  ( 25.52812500061451573, 6.421520780324663323E-16, -5.243569643749999010 ) ) ;
#14994 = CARTESIAN_POINT ( 'NONE',  ( 28.05937500061451573, 0.000000000000000000, 5.243569643749999010 ) ) ;
#14995 = CARTESIAN_POINT ( 'NONE',  ( 3.121875000614518836, 3.027376345333613106, -5.243569643749998122 ) ) ;
#14996 = CARTESIAN_POINT ( 'NONE',  ( 14.62500000000000000, 4.330127018922191873, 2.499999999999999556 ) ) ;
#14997 = CARTESIAN_POINT ( 'NONE',  ( 11.35312500061451679, 0.000000000000000000, 5.243569643749999010 ) ) ;
#14998 = CARTESIAN_POINT ( 'NONE',  ( 15.31875000122903252, -5.773502691896255534, -1.060575238724906372E-15 ) ) ;
#14999 = CARTESIAN_POINT ( 'NONE',  ( 9.656250001229032875, 4.330127018922192761, -2.499999999999997780 ) ) ;
#15000 = CARTESIAN_POINT ( 'NONE',  ( 29.09062500061451217, -3.027376345333610441, -5.243569643749999898 ) ) ;
#15001 = CARTESIAN_POINT ( 'NONE',  ( 15.30000000122903359, -2.886751345948129988, 4.999999999999997335 ) ) ;
#15002 = CARTESIAN_POINT ( 'NONE',  ( 8.643750001229031810, -2.886751345948181946, -4.999999999999904077 ) ) ;
#15003 = CARTESIAN_POINT ( 'NONE',  ( 18.04687500061451999, 5.492252693125287522, 3.363034840372157021E-16 ) ) ;
#15004 = CARTESIAN_POINT ( 'NONE',  ( 5.015625000614518214, 3.027376345333611329, 5.243569643749999010 ) ) ;
#15005 = CARTESIAN_POINT ( 'NONE',  ( 21.42187500061451644, -6.054752690667223547, -1.112240025338166033E-15 ) ) ;
#15006 = CARTESIAN_POINT ( 'NONE',  ( 9.001249775931846008E-16, 16.82187500061451857, 34.90005215228797653 ) ) ;
#15007 = CARTESIAN_POINT ( 'NONE',  ( 23.37187500061451573, 3.027376345333613106, -5.243569643749998122 ) ) ;
#15008 = CARTESIAN_POINT ( 'NONE',  ( 6.262500000000000178, -5.773502691896255534, -1.060575238724906372E-15 ) ) ;
#15009 = CARTESIAN_POINT ( 'NONE',  ( 2.000000000000001332, 11.26250000122903394, 33.46410161513774995 ) ) ;
#15010 = CARTESIAN_POINT ( 'NONE',  ( 13.26562500061451644, -6.054752690667223547, -1.112240025338166033E-15 ) ) ;
#15011 = CARTESIAN_POINT ( 'NONE',  ( 4.500000001229034652, -2.886751345948129988, 4.999999999999997335 ) ) ;
#15012 = CARTESIAN_POINT ( 'NONE',  ( 9.834375000614517859, 6.421520780324663323E-16, -5.243569643749999010 ) ) ;
#15013 = CARTESIAN_POINT ( 'NONE',  ( 9.365625000614519635, 3.027376345333613106, -5.243569643749998122 ) ) ;
#15014 = CARTESIAN_POINT ( 'NONE',  ( 15.00937500061451679, 0.000000000000000000, 5.243569643749999010 ) ) ;
#15015 = DIRECTION ( 'NONE',  ( 0.000000000000000000, 0.000000000000000000, 1.000000000000000000 ) ) ;
#15016 = CARTESIAN_POINT ( 'NONE',  ( 22.12500000122903288, -5.773502691896255534, -1.060575238724906372E-15 ) ) ;
#15017 = CARTESIAN_POINT ( 'NONE',  ( 11.52187500061451608, -6.054752690667223547, -1.112240025338166033E-15 ) ) ;
#15018 = CARTESIAN_POINT ( 'NONE',  ( 12.40312500061451573, -4.541064518000417216, -2.621784821875001281 ) ) ;
#15019 = CARTESIAN_POINT ( 'NONE',  ( 29.11875000122903501, 2.886751345948126879, 4.999999999999999112 ) ) ;
#15020 = CARTESIAN_POINT ( 'NONE',  ( 21.08437500061451786, 6.421520780324663323E-16, -5.243569643749999010 ) ) ;
#15021 = CARTESIAN_POINT ( 'NONE',  ( 25.61250000122903359, 0.000000000000000000, 4.999999999999998224 ) ) ;
#15022 = CARTESIAN_POINT ( 'NONE',  ( -4.243569643749999898, 19.85937500061451644, -30.00000000000000000 ) ) ;
#15023 = AXIS2_PLACEMENT_3D ( 'NONE', #21549, #10114, #16007 ) ;
#15024 = CARTESIAN_POINT ( 'NONE',  ( 3.224120815779399241, 3.821689571648150707, -3.388499519612508060 ) ) ;
#15025 = CARTESIAN_POINT ( 'NONE',  ( 4.243569643749999010, 13.37187500061451750, -32.45002607614398471 ) ) ;
#15026 = CARTESIAN_POINT ( 'NONE',  ( 15.86250000122903181, -4.330127018922190985, -2.500000000000001332 ) ) ;
#15027 = CARTESIAN_POINT ( 'NONE',  ( 9.234375000614518214, -4.541064518000419881, 2.621784821874995952 ) ) ;
#15028 = CARTESIAN_POINT ( 'NONE',  ( 2.121784821875001281, 17.25312500061451715, -26.32496088578401938 ) ) ;
#15029 = CARTESIAN_POINT ( 'NONE',  ( 18.00000000122903288, -2.886751345948129988, 4.999999999999997335 ) ) ;
#15030 = CARTESIAN_POINT ( 'NONE',  ( 9.103125000614515017, 0.000000000000000000, 5.243569643749999010 ) ) ;
#15031 = EDGE_LOOP ( 'NONE', ( #62888, #6370, #64178, #31256 ) ) ;
#15032 = CARTESIAN_POINT ( 'NONE',  ( 16.08749999999999503, -2.886751345948129988, 4.999999999999997335 ) ) ;
#15033 = CARTESIAN_POINT ( 'NONE',  ( 17.84999999999999787, 0.000000000000000000, 4.999999999999998224 ) ) ;
#15034 = CARTESIAN_POINT ( 'NONE',  ( 8.971875000614515372, 3.027376345333612662, -5.243569643749998122 ) ) ;
#15035 = CARTESIAN_POINT ( 'NONE',  ( 4.384576699563885960, -2.403224326949449097, -4.660422238726323663 ) ) ;
#15036 = CARTESIAN_POINT ( 'NONE',  ( 11.32500000122903394, -5.773502691896255534, -1.060575238724906372E-15 ) ) ;
#15037 = CARTESIAN_POINT ( 'NONE',  ( 19.57500000122903216, 2.886751345948129099, -4.999999999999998224 ) ) ;
#15038 = CARTESIAN_POINT ( 'NONE',  ( 14.95312500061451644, 0.000000000000000000, 5.243569643749999010 ) ) ;
#15039 = CARTESIAN_POINT ( 'NONE',  ( 20.24062500061451431, 6.054752690667223547, 3.707466751127219781E-16 ) ) ;
#15040 = CARTESIAN_POINT ( 'NONE',  ( 27.15000000122902790, -2.886751345948125991, -5.000000000000000000 ) ) ;
#15041 = EDGE_CURVE ( 'NONE', #4907, #42330, #6390, .T. ) ;
#15042 = CARTESIAN_POINT ( 'NONE',  ( 3.515625000614516882, 3.027376345333613106, -5.243569643749998122 ) ) ;
#15043 = CARTESIAN_POINT ( 'NONE',  ( 24.26249999999999929, -5.773502691896255534, -1.060575238724906372E-15 ) ) ;
#15044 = CARTESIAN_POINT ( 'NONE',  ( 1.878215178125000495, 14.06562499938548250, 26.74683588394047007 ) ) ;
#15045 = CARTESIAN_POINT ( 'NONE',  ( 28.23750000000000426, -2.886751345948129988, 4.999999999999997335 ) ) ;
#15046 = CARTESIAN_POINT ( 'NONE',  ( 27.38437500061451857, 6.421520780324663323E-16, -5.243569643749999010 ) ) ;
#15047 = CARTESIAN_POINT ( 'NONE',  ( -1.487416814333745711E-14, 16.06250000000000000, 34.00000000000000000 ) ) ;
#15048 = CARTESIAN_POINT ( 'NONE',  ( 11.70000000122903216, -2.886751345948129988, 4.999999999999997335 ) ) ;
#15049 = CARTESIAN_POINT ( 'NONE',  ( 4.125000000000000000, 6.123233995736764310E-16, -4.999999999999998224 ) ) ;
#15050 = EDGE_CURVE ( 'NONE', #42983, #31892, #42611, .T. ) ;
#15051 = CARTESIAN_POINT ( 'NONE',  ( -4.000000000000000000, 18.51874999877096784, 30.00000000000000000 ) ) ;
#15052 = CARTESIAN_POINT ( 'NONE',  ( 7.284375000614518036, 4.541064518000418104, 2.621784821874999949 ) ) ;
#15053 = CARTESIAN_POINT ( 'NONE',  ( 25.15312500061451217, 4.541064518000418104, -2.621784821874998173 ) ) ;
#15054 = CARTESIAN_POINT ( 'NONE',  ( 3.756430356250000102, 13.20312499938548356, 30.00000000000000000 ) ) ;
#15055 = CARTESIAN_POINT ( 'NONE',  ( 22.53749999999999787, -2.886751345948153968, -4.999999999999952038 ) ) ;
#15056 = CARTESIAN_POINT ( 'NONE',  ( -3.999999999999999112, 19.66250000122903430, 30.00000000000000000 ) ) ;
#15057 = CARTESIAN_POINT ( 'NONE',  ( 5.146875000614517859, -3.027376345333614438, 5.243569643749998122 ) ) ;
#15058 = CARTESIAN_POINT ( 'NONE',  ( 7.771875000614516971, 3.027376345333611329, 5.243569643749999010 ) ) ;
#15059 = CARTESIAN_POINT ( 'NONE',  ( 5.212500000000002132, 2.886751345948126879, 4.999999999999999112 ) ) ;
#15060 = AXIS2_PLACEMENT_3D ( 'NONE', #29809, #14267, #18339 ) ;
#15061 = CARTESIAN_POINT ( 'NONE',  ( -4.243569643749999898, 13.05312500061459602, 30.00000000000000000 ) ) ;
#15062 = CARTESIAN_POINT ( 'NONE',  ( 21.60000000000000142, -4.330127018922190985, -2.500000000000001332 ) ) ;
#15063 = CARTESIAN_POINT ( 'NONE',  ( 28.94999999999999929, 4.330127018922192761, -2.499999999999997780 ) ) ;
#15064 = CARTESIAN_POINT ( 'NONE',  ( 3.037500000000002309, -2.886751345948129988, 4.999999999999997335 ) ) ;
#15065 = VERTEX_POINT ( 'NONE', #22613 ) ;
#15066 = CARTESIAN_POINT ( 'NONE',  ( 17.39062500061451644, -3.027376345333610441, -5.243569643749999898 ) ) ;
#15067 = CARTESIAN_POINT ( 'NONE',  ( 11.20312500061451644, 4.541064518000418104, -2.621784821874998173 ) ) ;
#15068 = CARTESIAN_POINT ( 'NONE',  ( 20.55937500061451217, 2.746126346562645981, -4.756430356249997438 ) ) ;
#15069 = CARTESIAN_POINT ( 'NONE',  ( 6.009375000614519458, 0.000000000000000000, 5.243569643749999010 ) ) ;
#15070 = CARTESIAN_POINT ( 'NONE',  ( 22.83749999999999858, -2.886751345948129988, 4.999999999999997335 ) ) ;
#15071 = CARTESIAN_POINT ( 'NONE',  ( 20.47500000122903074, 2.886751345948129099, -4.999999999999998224 ) ) ;
#15072 = CARTESIAN_POINT ( 'NONE',  ( 15.59999999999999964, 0.000000000000000000, 4.999999999999998224 ) ) ;
#15073 = CARTESIAN_POINT ( 'NONE',  ( 10.13437500061451679, -4.541064518000419881, 2.621784821874995952 ) ) ;
#15074 = CARTESIAN_POINT ( 'NONE',  ( 14.63437500061451679, -4.541064518000419881, 2.621784821874995952 ) ) ;
#15075 = CARTESIAN_POINT ( 'NONE',  ( 23.63437500061451502, -4.541064518000419881, 2.621784821874995952 ) ) ;
#15076 = CARTESIAN_POINT ( 'NONE',  ( 8.512500001229033941, 0.000000000000000000, 4.999999999999998224 ) ) ;
#15077 = CARTESIAN_POINT ( 'NONE',  ( 12.59999999999999964, -4.330127018922190985, -2.500000000000001332 ) ) ;
#15078 = CARTESIAN_POINT ( 'NONE',  ( 17.33437500061451431, -4.541064518000419881, 2.621784821874995952 ) ) ;
#15079 = CARTESIAN_POINT ( 'NONE',  ( 9.909375000614517148, 4.541064518000418104, -2.621784821874998173 ) ) ;
#15080 = CARTESIAN_POINT ( 'NONE',  ( -3.756430356249999214, 20.59062499938548640, 27.83122392262697531 ) ) ;
#15081 = CARTESIAN_POINT ( 'NONE',  ( 20.43749999999999645, 5.773502691896255534, 3.535250795749688894E-16 ) ) ;
#15082 = CARTESIAN_POINT ( 'NONE',  ( -1.999999999999999112, 15.80000000000000071, 26.53589838486224650 ) ) ;
#15083 = CARTESIAN_POINT ( 'NONE',  ( 4.243569643749999010, 10.67187500061451644, -32.45002607614398471 ) ) ;
#15084 = CARTESIAN_POINT ( 'NONE',  ( 25.09687500061451715, -2.746126346562642428, -4.756430356249999214 ) ) ;
#15085 = CARTESIAN_POINT ( 'NONE',  ( 11.76562500061451644, 3.027376345333611329, 5.243569643749999010 ) ) ;
#15086 = CARTESIAN_POINT ( 'NONE',  ( 28.69687500061451502, -3.027376345333610441, -5.243569643749999898 ) ) ;
#15087 = CARTESIAN_POINT ( 'NONE',  ( 34.99999999999999289, 2.500000000000000444, 3.499999999999999112 ) ) ;
#15088 = CARTESIAN_POINT ( 'NONE',  ( 1.071796769724491893, 9.895096190661368141, -26.00000000000000355 ) ) ;
#15089 = CARTESIAN_POINT ( 'NONE',  ( 11.47499999999999964, 4.330127018922191873, 2.499999999999999556 ) ) ;
#15090 = CARTESIAN_POINT ( 'NONE',  ( 2.000000000000001332, 18.01250000122903572, 33.46410161513774995 ) ) ;
#15091 = CARTESIAN_POINT ( 'NONE',  ( 11.62500000122903465, 2.886751345948126879, 4.999999999999999112 ) ) ;
#15092 = CARTESIAN_POINT ( 'NONE',  ( 21.49687500061451573, -3.027376345333610441, -5.243569643749999898 ) ) ;
#15093 = CARTESIAN_POINT ( 'NONE',  ( 17.59687500061451715, 6.054752690667223547, 3.707466751127219781E-16 ) ) ;
#15094 = LINE ( 'NONE', #8829, #30116 ) ;
#15095 = ORIENTED_EDGE ( 'NONE', *, *, #2515, .T. ) ;
#15096 = CARTESIAN_POINT ( 'NONE',  ( 18.17812500061451786, -4.541064518000419881, 2.621784821874995952 ) ) ;
#15097 = CARTESIAN_POINT ( 'NONE',  ( 27.82500000122903572, 2.886751345948126879, 4.999999999999999112 ) ) ;
#15098 = CARTESIAN_POINT ( 'NONE',  ( 17.70937500061451431, 0.000000000000000000, 5.243569643749999010 ) ) ;
#15099 = CARTESIAN_POINT ( 'NONE',  ( 4.078125000614517326, 4.541064518000418104, 2.621784821874999949 ) ) ;
#15100 = CARTESIAN_POINT ( 'NONE',  ( 18.51562500061451289, 3.027376345333611329, 5.243569643749999010 ) ) ;
#15101 = CARTESIAN_POINT ( 'NONE',  ( -4.000000000000000000, 15.42500000000000071, 30.00000000000000000 ) ) ;
#15102 = CARTESIAN_POINT ( 'NONE',  ( 28.43437500061451573, 4.541064518000418104, 2.621784821874999949 ) ) ;
#15103 = CARTESIAN_POINT ( 'NONE',  ( 2.121784821874999061, 12.45312500061451821, 26.32496088578401583 ) ) ;
#15104 = CARTESIAN_POINT ( 'NONE',  ( 16.95000000122903216, 5.773502691896255534, 3.535250795749688894E-16 ) ) ;
#15105 = CARTESIAN_POINT ( 'NONE',  ( 9.984375000614518214, 4.119189519843966529, 2.378215178124999607 ) ) ;
#15106 = CARTESIAN_POINT ( 'NONE',  ( 27.74062500061451431, -3.027376345333610441, -5.243569643749999898 ) ) ;
#15107 = FACE_OUTER_BOUND ( 'NONE', #7422, .T. ) ;
#15108 = CARTESIAN_POINT ( 'NONE',  ( 20.03437500061451715, -4.541064518000419881, 2.621784821874995952 ) ) ;
#15109 = CARTESIAN_POINT ( 'NONE',  ( 22.95000000122903216, -2.886751345948129988, 4.999999999999997335 ) ) ;
#15110 = CARTESIAN_POINT ( 'NONE',  ( 22.67812500061451431, -4.541064518000419881, 2.621784821874995952 ) ) ;
#15111 = CARTESIAN_POINT ( 'NONE',  ( 16.99687500061451573, -3.027376345333610441, -5.243569643749999898 ) ) ;
#15112 = CARTESIAN_POINT ( 'NONE',  ( 11.84062500061451750, -3.027376345333614438, 5.243569643749998122 ) ) ;
#15113 = CARTESIAN_POINT ( 'NONE',  ( -2.121784821874996840, 14.53437500061451715, 33.67503911421598417 ) ) ;
#15114 = CARTESIAN_POINT ( 'NONE',  ( 18.74062500061451431, -3.027376345333610441, -5.243569643749999898 ) ) ;
#15115 = CARTESIAN_POINT ( 'NONE',  ( 29.46562500061451573, -6.054752690667223547, -1.112240025338166033E-15 ) ) ;
#15116 = ORIENTED_EDGE ( 'NONE', *, *, #17491, .T. ) ;
#15117 = EDGE_LOOP ( 'NONE', ( #49906, #65000, #40093, #20798 ) ) ;
#15118 = CARTESIAN_POINT ( 'NONE',  ( 22.76249999999999574, 2.886751345948126879, 4.999999999999999112 ) ) ;
#15119 = CARTESIAN_POINT ( 'NONE',  ( 4.243569643749999898, 18.28437500061451715, -30.00000000000000000 ) ) ;
#15120 = CARTESIAN_POINT ( 'NONE',  ( 14.75625000122903252, 0.000000000000000000, 4.999999999999998224 ) ) ;
#15121 = CARTESIAN_POINT ( 'NONE',  ( 24.36562500061451786, 3.027376345333611329, 5.243569643749999010 ) ) ;
#15122 = CARTESIAN_POINT ( 'NONE',  ( 5.315625000614516260, 3.027376345333613106, -5.243569643749998122 ) ) ;
#15123 = CARTESIAN_POINT ( 'NONE',  ( 18.03750000122903430, -4.330127018922194537, 2.499999999999995559 ) ) ;
#15124 = CARTESIAN_POINT ( 'NONE',  ( 23.84062500061451928, 6.054752690667223547, 3.707466751127219781E-16 ) ) ;
#15125 = CARTESIAN_POINT ( 'NONE',  ( 23.17500000000000071, 4.330127018922191873, 2.499999999999999556 ) ) ;
#15126 = CARTESIAN_POINT ( 'NONE',  ( 28.56562500061451715, -6.054752690667223547, -1.112240025338166033E-15 ) ) ;
#15127 = CARTESIAN_POINT ( 'NONE',  ( 8.953125000614518214, 4.541064518000418104, -2.621784821874998173 ) ) ;
#15128 = VERTEX_POINT ( 'NONE', #55521 ) ;
#15129 = CARTESIAN_POINT ( 'NONE',  ( 23.65312500061451573, -4.541064518000417216, -2.621784821875001281 ) ) ;
#15130 = CARTESIAN_POINT ( 'NONE',  ( 4.978125000614518569, 4.541064518000418104, 2.621784821874999949 ) ) ;
#15131 = CARTESIAN_POINT ( 'NONE',  ( 13.35937500061451821, -4.119189519843965641, -2.378215178125001383 ) ) ;
#15132 = CARTESIAN_POINT ( 'NONE',  ( 4.303125000614516971, -4.541064518000417216, -2.621784821875001281 ) ) ;
#15133 = CARTESIAN_POINT ( 'NONE',  ( -2.828200636599751609E-16, 13.25000000122903288, -34.61880215351700230 ) ) ;
#15134 = EDGE_CURVE ( 'NONE', #6811, #66841, #37434, .T. ) ;
#15135 = CARTESIAN_POINT ( 'NONE',  ( 11.06250000000000000, 2.886751345948126879, 4.999999999999999112 ) ) ;
#15136 = CARTESIAN_POINT ( 'NONE',  ( 10.73437500061451644, 6.421520780324663323E-16, -5.243569643749999010 ) ) ;
#15137 = CARTESIAN_POINT ( 'NONE',  ( 6.862500001229034474, -4.330127018922190985, -2.500000000000001332 ) ) ;
#15138 = CARTESIAN_POINT ( 'NONE',  ( 13.47187500061451537, 3.027376345333613106, -5.243569643749998122 ) ) ;
#15139 = CARTESIAN_POINT ( 'NONE',  ( 6.346875000614517148, 6.054752690667223547, 3.707466751127219781E-16 ) ) ;
#15140 = CARTESIAN_POINT ( 'NONE',  ( -4.243569643749997233, 10.39062500061451644, -27.54997392385601174 ) ) ;
#15141 = CARTESIAN_POINT ( 'NONE',  ( 3.467284487300496654, 3.602878009983967900, 3.467284487300496654 ) ) ;
#15142 = CARTESIAN_POINT ( 'NONE',  ( 12.72187500061451537, 3.027376345333611329, 5.243569643749999010 ) ) ;
#15143 = CARTESIAN_POINT ( 'NONE',  ( 3.700875911142169628, 3.362093191700385564, 4.023865622399847020 ) ) ;
#15144 = CARTESIAN_POINT ( 'NONE',  ( 21.02812500061451573, 6.421520780324663323E-16, -5.243569643749999010 ) ) ;
#15145 = CARTESIAN_POINT ( 'NONE',  ( 4.243569643749999898, 10.63437500061451857, 30.00000000000000000 ) ) ;
#15146 = CARTESIAN_POINT ( 'NONE',  ( 20.11875000122903145, 2.886751345948182834, 4.999999999999902300 ) ) ;
#15147 = CARTESIAN_POINT ( 'NONE',  ( 24.34687500061451715, 6.054752690667223547, 3.707466751127219781E-16 ) ) ;
#15148 = CYLINDRICAL_SURFACE ( 'NONE', #72122, 4.999999999999998224 ) ;
#15149 = CARTESIAN_POINT ( 'NONE',  ( 4.565625000614516260, 3.027376345333611329, 5.243569643749999010 ) ) ;
#15150 = CARTESIAN_POINT ( 'NONE',  ( 18.98437500061451289, -2.746126346562646425, 4.756430356249996549 ) ) ;
#15151 = CARTESIAN_POINT ( 'NONE',  ( 19.04062500061451146, -3.027376345333614438, 5.243569643749998122 ) ) ;
#15152 = CARTESIAN_POINT ( 'NONE',  ( 14.52187500061451608, 3.027376345333611329, 5.243569643749999010 ) ) ;
#15153 = CARTESIAN_POINT ( 'NONE',  ( 0.000000000000000000, 27.50000000000000000, 30.00000000000000000 ) ) ;
#15154 = CARTESIAN_POINT ( 'NONE',  ( 27.60000000122903430, -2.886751345948125991, -5.000000000000000000 ) ) ;
#15155 = CARTESIAN_POINT ( 'NONE',  ( 5.371875000614516615, 3.027376345333613106, -5.243569643749998122 ) ) ;
#15156 = CARTESIAN_POINT ( 'NONE',  ( 17.82187500061451502, -6.054752690667223547, -1.112240025338166033E-15 ) ) ;
#15157 = CARTESIAN_POINT ( 'NONE',  ( 15.15000000000000036, 0.000000000000000000, 4.999999999999998224 ) ) ;
#15158 = CARTESIAN_POINT ( 'NONE',  ( 23.40000000000000213, -4.330127018922190985, -2.500000000000001332 ) ) ;
#15159 = CARTESIAN_POINT ( 'NONE',  ( 2.662500001229036073, 0.000000000000000000, 4.999999999999998224 ) ) ;
#15160 = CARTESIAN_POINT ( 'NONE',  ( 24.87187500061451573, 3.027376345333611329, 5.243569643749999010 ) ) ;
#15161 = CARTESIAN_POINT ( 'NONE',  ( 17.22187500061451715, 3.027376345333611329, 5.243569643749999010 ) ) ;
#15162 = CARTESIAN_POINT ( 'NONE',  ( 2.655984681222220721E-16, 13.31562499938548783, 25.66244784525396483 ) ) ;
#15163 = CARTESIAN_POINT ( 'NONE',  ( 21.89999999999999858, 0.000000000000000000, 4.999999999999998224 ) ) ;
#15164 = CARTESIAN_POINT ( 'NONE',  ( 6.937499999999999112, 5.773502691896255534, 3.535250795749688894E-16 ) ) ;
#15165 = CARTESIAN_POINT ( 'NONE',  ( 9.721875000614517148, 5.824947211148865298E-16, -4.756430356249998326 ) ) ;
#15166 = CARTESIAN_POINT ( 'NONE',  ( 19.26562500061451644, 3.027376345333613106, -5.243569643749998122 ) ) ;
#15167 = CARTESIAN_POINT ( 'NONE',  ( 9.187500000000001776, 5.773502691896255534, 3.535250795749688894E-16 ) ) ;
#15168 = CARTESIAN_POINT ( 'NONE',  ( 3.890625000614517326, -3.027376345333610441, -5.243569643749999898 ) ) ;
#15169 = CARTESIAN_POINT ( 'NONE',  ( 18.48750000000000071, -2.886751345948125991, -5.000000000000000000 ) ) ;
#15170 = CARTESIAN_POINT ( 'NONE',  ( 18.85312500061451502, 4.541064518000418104, -2.621784821874998173 ) ) ;
#15171 = LINE ( 'NONE', #61339, #57274 ) ;
#15172 = CARTESIAN_POINT ( 'NONE',  ( 23.28750000122903430, 4.330127018922191873, 2.499999999999999556 ) ) ;
#15173 = DIRECTION ( 'NONE',  ( -1.000000000000000000, -0.000000000000000000, -0.000000000000000000 ) ) ;
#15174 = CARTESIAN_POINT ( 'NONE',  ( 29.03437500061451715, -4.541064518000419881, 2.621784821874995952 ) ) ;
#15175 = ORIENTED_EDGE ( 'NONE', *, *, #28049, .T. ) ;
#15176 = CARTESIAN_POINT ( 'NONE',  ( 16.64062500061451289, 6.054752690667223547, 3.707466751127219781E-16 ) ) ;
#15177 = CARTESIAN_POINT ( 'NONE',  ( 24.55312500061451786, -4.541064518000417216, -2.621784821875001281 ) ) ;
#15178 = CARTESIAN_POINT ( 'NONE',  ( 25.32187500061451857, 3.027376345333611329, 5.243569643749999010 ) ) ;
#15179 = CARTESIAN_POINT ( 'NONE',  ( 8.287499999999999645, 5.773502691896255534, 3.535250795749688894E-16 ) ) ;
#15180 = CARTESIAN_POINT ( 'NONE',  ( 12.36562500061451608, -6.054752690667223547, -1.112240025338166033E-15 ) ) ;
#15181 = CARTESIAN_POINT ( 'NONE',  ( 27.62812500061451360, -4.541064518000419881, 2.621784821874995952 ) ) ;
#15182 = CARTESIAN_POINT ( 'NONE',  ( 17.40937500061451715, -4.541064518000417216, -2.621784821875001281 ) ) ;
#15183 = CARTESIAN_POINT ( 'NONE',  ( 19.69687500061451857, -3.027376345333610441, -5.243569643749999898 ) ) ;
#15184 = DIRECTION ( 'NONE',  ( 0.000000000000000000, 0.000000000000000000, -1.000000000000000000 ) ) ;
#15185 = CARTESIAN_POINT ( 'NONE',  ( -4.243569643749999898, 10.40937500061451892, 30.00000000000000000 ) ) ;
#15186 =( BOUNDED_CURVE ( )  B_SPLINE_CURVE ( 2, ( #35178, #24085, #69174, #1942, #18535, #7466, #29992 ),
 .UNSPECIFIED., .F., .F. ) 
 B_SPLINE_CURVE_WITH_KNOTS ( ( 3, 2, 2, 3 ),
 ( 0.8750000000000000000, 0.8777777777777777679, 0.8805555555555555358, 0.8833333333333333037 ),
 .UNSPECIFIED. ) 
 CURVE ( )  GEOMETRIC_REPRESENTATION_ITEM ( )  RATIONAL_B_SPLINE_CURVE ( ( 1.000000000000000000, 0.8660254037844387076, 1.000000000000000000, 0.8660254037844387076, 1.000000000000000000, 0.8660254037844387076, 1.000000000000000000 ) ) 
 REPRESENTATION_ITEM ( '' )  );
#15187 = CARTESIAN_POINT ( 'NONE',  ( 23.17500000122903359, 2.886751345948129099, -4.999999999999998224 ) ) ;
#15188 = CARTESIAN_POINT ( 'NONE',  ( 16.54687500061451644, -2.746126346562641984, -4.756430356249999214 ) ) ;
#15189 = CARTESIAN_POINT ( 'NONE',  ( 14.27812500061451573, 6.421520780324663323E-16, -5.243569643749999010 ) ) ;
#15190 = CARTESIAN_POINT ( 'NONE',  ( 7.396875000614519635, -3.027376345333614438, 5.243569643749998122 ) ) ;
#15191 = CARTESIAN_POINT ( 'NONE',  ( 8.071875000614518569, 3.027376345333613106, -5.243569643749998122 ) ) ;
#15192 = ORIENTED_EDGE ( 'NONE', *, *, #4728, .F. ) ;
#15193 = CARTESIAN_POINT ( 'NONE',  ( 2.000000000000001332, 13.40000000000000213, 33.46410161513774995 ) ) ;
#15194 = CARTESIAN_POINT ( 'NONE',  ( 19.11562500061451431, -6.054752690667223547, -1.112240025338166033E-15 ) ) ;
#15195 = EDGE_CURVE ( 'NONE', #47001, #28339, #19942, .T. ) ;
#15196 = CARTESIAN_POINT ( 'NONE',  ( 23.55937500061451573, 0.000000000000000000, 5.243569643749999010 ) ) ;
#15197 = CARTESIAN_POINT ( 'NONE',  ( 18.40312500061451573, 4.541064518000418104, -2.621784821874998173 ) ) ;
#15198 = CARTESIAN_POINT ( 'NONE',  ( 8.484601909799253346E-16, 12.01250000000000107, 34.61880215351700230 ) ) ;
#15199 = CARTESIAN_POINT ( 'NONE',  ( 27.92812500061451431, 4.541064518000418104, 2.621784821874999949 ) ) ;
#15200 = CARTESIAN_POINT ( 'NONE',  ( 7.125000001229033764, 2.886751345948126879, 4.999999999999999112 ) ) ;
#15201 = VERTEX_POINT ( 'NONE', #22258 ) ;
#15202 = DIRECTION ( 'NONE',  ( -1.000000000000000000, -0.000000000000000000, -0.000000000000000000 ) ) ;
#15203 = CARTESIAN_POINT ( 'NONE',  ( 3.999999999999999112, 14.37500000000000000, -30.00000000000000000 ) ) ;
#15204 = CARTESIAN_POINT ( 'NONE',  ( 21.18750000122903288, -4.330127018922194537, 2.499999999999995559 ) ) ;
#15205 = CARTESIAN_POINT ( 'NONE',  ( -7.967954043666661671E-16, 13.99062499938548498, 34.33755215474603517 ) ) ;
#15206 = CARTESIAN_POINT ( 'NONE',  ( 7.434375000614519280, -4.541064518000419881, 2.621784821874995952 ) ) ;
#15207 = CARTESIAN_POINT ( 'NONE',  ( 4.411272977760241965, 2.353862934769528348, -4.685547128476531320 ) ) ;
#15208 = CARTESIAN_POINT ( 'NONE',  ( 11.76562500061451644, 3.027376345333611329, 5.243569643749999010 ) ) ;
#15209 = CARTESIAN_POINT ( 'NONE',  ( 7.471875000614519813, -6.054752690667223547, -1.112240025338166033E-15 ) ) ;
#15210 = CARTESIAN_POINT ( 'NONE',  ( 27.26250000122903216, 4.330127018922192761, -2.499999999999997780 ) ) ;
#15211 = CARTESIAN_POINT ( 'NONE',  ( 13.77187500061451786, -6.054752690667223547, -1.112240025338166033E-15 ) ) ;
#15212 = CARTESIAN_POINT ( 'NONE',  ( 5.259375000614518569, -4.541064518000417216, -2.621784821875001281 ) ) ;
#15213 = CARTESIAN_POINT ( 'NONE',  ( 29.55000000000000071, 0.000000000000000000, 4.999999999999998224 ) ) ;
#15214 = CARTESIAN_POINT ( 'NONE',  ( 6.553125000614518747, -4.541064518000417216, -2.621784821875001281 ) ) ;
#15215 = CARTESIAN_POINT ( 'NONE',  ( 14.50312500061451537, 0.000000000000000000, 5.243569643749999010 ) ) ;
#15216 =( BOUNDED_CURVE ( )  B_SPLINE_CURVE ( 2, ( #56821, #39489, #22841, #10318, #45393, #67929, #17302, #34289, #6228 ),
 .UNSPECIFIED., .F., .F. ) 
 B_SPLINE_CURVE_WITH_KNOTS ( ( 3, 2, 2, 2, 3 ),
 ( 0.1630434782608695676, 0.1666666666666666574, 0.1739130434782608647, 0.1811594202898550721, 0.1847826086956521896 ),
 .UNSPECIFIED. ) 
 CURVE ( )  GEOMETRIC_REPRESENTATION_ITEM ( )  RATIONAL_B_SPLINE_CURVE ( ( 0.9330127018922194093, 0.9330127018922196314, 1.000000000000000000, 0.8660254037844387076, 1.000000000000000000, 0.8660254037844387076, 1.000000000000000000, 0.9330127018922190762, 0.9330127018922194093 ) ) 
 REPRESENTATION_ITEM ( '' )  );
#15217 = ORIENTED_EDGE ( 'NONE', *, *, #29254, .T. ) ;
#15218 = CARTESIAN_POINT ( 'NONE',  ( 11.84062500061451750, -3.027376345333614438, 5.243569643749998122 ) ) ;
#15219 = CARTESIAN_POINT ( 'NONE',  ( 5.362500001229033586, 0.000000000000000000, 4.999999999999998224 ) ) ;
#15220 = CARTESIAN_POINT ( 'NONE',  ( 7.978125000614517681, 6.421520780324663323E-16, -5.243569643749999010 ) ) ;
#15221 = CARTESIAN_POINT ( 'NONE',  ( 21.30937500061451573, 0.000000000000000000, 4.756430356249998326 ) ) ;
#15222 = CARTESIAN_POINT ( 'NONE',  ( 9.750000000000001776, 0.000000000000000000, 4.999999999999998224 ) ) ;
#15223 = CARTESIAN_POINT ( 'NONE',  ( 4.537500001229034297, -4.330127018922194537, 2.499999999999995559 ) ) ;
#15224 = CARTESIAN_POINT ( 'NONE',  ( 19.12500000000000000, 4.330127018922191873, 2.499999999999999556 ) ) ;
#15225 = CARTESIAN_POINT ( 'NONE',  ( 18.30937500061451928, -4.541064518000417216, -2.621784821875001281 ) ) ;
#15226 = CARTESIAN_POINT ( 'NONE',  ( 13.46250000122903323, 0.000000000000000000, 4.999999999999998224 ) ) ;
#15227 = CARTESIAN_POINT ( 'NONE',  ( 22.76249999999999574, 2.886751345948126879, 4.999999999999999112 ) ) ;
#15228 =( BOUNDED_CURVE ( )  B_SPLINE_CURVE ( 2, ( #19393, #20127, #26055, #8330, #14231, #53398, #48595 ),
 .UNSPECIFIED., .F., .F. ) 
 B_SPLINE_CURVE_WITH_KNOTS ( ( 3, 2, 2, 3 ),
 ( 0.9769893167920098431, 0.9777777777777777457, 0.9805555555555555136, 0.9812695158790134542 ),
 .UNSPECIFIED. ) 
 CURVE ( )  GEOMETRIC_REPRESENTATION_ITEM ( )  RATIONAL_B_SPLINE_CURVE ( ( 0.9455319771198016365, 0.9619718528080076769, 1.000000000000000000, 0.8660254037844387076, 1.000000000000000000, 0.9655650834222846424, 0.9488314850527816979 ) ) 
 REPRESENTATION_ITEM ( '' )  );
#15229 = CARTESIAN_POINT ( 'NONE',  ( 2.121784821874999061, 17.40312500061451573, -33.67503911421598417 ) ) ;
#15230 = DIRECTION ( 'NONE',  ( 0.000000000000000000, 0.000000000000000000, -1.000000000000000000 ) ) ;
#15231 = CARTESIAN_POINT ( 'NONE',  ( 21.67500000000000071, 6.123233995736764310E-16, -4.999999999999998224 ) ) ;
#15232 = CARTESIAN_POINT ( 'NONE',  ( 18.50625000122903430, -4.330127018922190985, -2.500000000000001332 ) ) ;
#15233 = CARTESIAN_POINT ( 'NONE',  ( 29.31562500061451715, 3.027376345333611329, 5.243569643749999010 ) ) ;
#15234 = EDGE_CURVE ( 'NONE', #15804, #54008, #45007, .T. ) ;
#15235 = DIRECTION ( 'NONE',  ( -1.000000000000000000, -0.000000000000000000, -0.000000000000000000 ) ) ;
#15236 = CARTESIAN_POINT ( 'NONE',  ( 15.90937500061451892, 0.000000000000000000, 5.243569643749999010 ) ) ;
#15237 = CARTESIAN_POINT ( 'NONE',  ( 26.51249999999999929, -5.773502691896255534, -1.060575238724906372E-15 ) ) ;
#15238 = CARTESIAN_POINT ( 'NONE',  ( 12.14062500061451821, 6.054752690667223547, 3.707466751127219781E-16 ) ) ;
#15239 = CARTESIAN_POINT ( 'NONE',  ( 7.631250001229033408, -4.330127018922194537, 2.499999999999995559 ) ) ;
#15240 = CARTESIAN_POINT ( 'NONE',  ( 20.74687500061451573, 6.054752690667223547, 3.707466751127219781E-16 ) ) ;
#15241 = CARTESIAN_POINT ( 'NONE',  ( 14.37187500061451573, 4.119189519843966529, 2.378215178124999607 ) ) ;
#15242 = CARTESIAN_POINT ( 'NONE',  ( 8.353125000614518569, -4.541064518000417216, -2.621784821875001281 ) ) ;
#15243 = CARTESIAN_POINT ( 'NONE',  ( 13.02187500061451608, 3.027376345333613106, -5.243569643749998122 ) ) ;
#15244 = ORIENTED_EDGE ( 'NONE', *, *, #57647, .F. ) ;
#15245 = CARTESIAN_POINT ( 'NONE',  ( 24.19687500061451857, -3.027376345333610441, -5.243569643749999898 ) ) ;
#15246 = CARTESIAN_POINT ( 'NONE',  ( 2.675063744352809358, 4.229653939133389606, -32.98446850650686457 ) ) ;
#15247 = CARTESIAN_POINT ( 'NONE',  ( 28.52812500061451573, -4.541064518000419881, 2.621784821874995952 ) ) ;
#15248 = CARTESIAN_POINT ( 'NONE',  ( 12.22499999999999964, 6.123233995736764310E-16, -4.999999999999998224 ) ) ;
#15249 = CARTESIAN_POINT ( 'NONE',  ( 7.687500000000000000, -2.886751345948125991, -5.000000000000000000 ) ) ;
#15250 = CARTESIAN_POINT ( 'NONE',  ( 16.95000000122903216, 5.773502691896255534, 3.535250795749688894E-16 ) ) ;
#15251 = CARTESIAN_POINT ( 'NONE',  ( 5.810221930991193690E-16, 19.75624999877096499, 26.00000000000000000 ) ) ;
#15252 = CARTESIAN_POINT ( 'NONE',  ( 9.234375000614514661, -2.746126346562642428, -4.756430356249999214 ) ) ;
#15253 = ORIENTED_EDGE ( 'NONE', *, *, #34980, .F. ) ;
#15254 = CARTESIAN_POINT ( 'NONE',  ( 15.82499999999999929, 6.123233995736764310E-16, -4.999999999999998224 ) ) ;
#15255 = CARTESIAN_POINT ( 'NONE',  ( 19.12500000000000000, 4.330127018922191873, 2.499999999999999556 ) ) ;
#15256 = CARTESIAN_POINT ( 'NONE',  ( 11.39062500061451644, -3.027376345333614438, 5.243569643749998122 ) ) ;
#15257 = ORIENTED_EDGE ( 'NONE', *, *, #11681, .T. ) ;
#15258 = CARTESIAN_POINT ( 'NONE',  ( 2.817472997146174052, -4.130598735093008678, -2.817472997146206026 ) ) ;
#15259 = CARTESIAN_POINT ( 'NONE',  ( -4.243569643749999898, 16.70937500061451786, -30.00000000000000000 ) ) ;
#15260 = CARTESIAN_POINT ( 'NONE',  ( 2.878125000614517592, -4.541064518000419881, 2.621784821874995952 ) ) ;
#15261 = CARTESIAN_POINT ( 'NONE',  ( 45.00000000000000000, 0.000000000000000000, 4.999999999999998224 ) ) ;
#15262 = CARTESIAN_POINT ( 'NONE',  ( 10.23750000000000071, -2.886751345948129988, 4.999999999999997335 ) ) ;
#15263 = CARTESIAN_POINT ( 'NONE',  ( 4.167140676845648706, 2.763139261668956514, -4.167140676845877856 ) ) ;
#15264 = VERTEX_POINT ( 'NONE', #38530 ) ;
#15265 = CARTESIAN_POINT ( 'NONE',  ( 2.121784821875001281, 12.75312500061451715, 33.67503911421598417 ) ) ;
#15266 = CARTESIAN_POINT ( 'NONE',  ( 27.85312500061451502, 4.541064518000418104, -2.621784821874998173 ) ) ;
#15267 = CARTESIAN_POINT ( 'NONE',  ( 18.52499999999999858, 6.123233995736764310E-16, -4.999999999999998224 ) ) ;
#15268 = CARTESIAN_POINT ( 'NONE',  ( 3.756430356249998770, 18.90312499938548640, 32.16877607737302469 ) ) ;
#15269 = CARTESIAN_POINT ( 'NONE',  ( 22.39687500061451075, -3.027376345333610441, -5.243569643749999898 ) ) ;
#15270 = CARTESIAN_POINT ( 'NONE',  ( 19.34062500061451573, 6.054752690667223547, 3.707466751127219781E-16 ) ) ;
#15271 = CARTESIAN_POINT ( 'NONE',  ( 9.001249775931846008E-16, 14.06562500061459353, -25.09994784771203058 ) ) ;
#15272 = CARTESIAN_POINT ( 'NONE',  ( 23.36250000122903359, 0.000000000000000000, 4.999999999999998224 ) ) ;
#15273 = CARTESIAN_POINT ( 'NONE',  ( 5.015625000614518214, 3.027376345333611329, 5.243569643749999010 ) ) ;
#15274 = CARTESIAN_POINT ( 'NONE',  ( 24.90937500061451715, 0.000000000000000000, 4.756430356249998326 ) ) ;
#15275 = CARTESIAN_POINT ( 'NONE',  ( 21.14062500061451644, 6.054752690667223547, 3.707466751127219781E-16 ) ) ;
#15276 = CARTESIAN_POINT ( 'NONE',  ( 7.734375000614517326, 4.119189519843966529, 2.378215178124999607 ) ) ;
#15277 = CARTESIAN_POINT ( 'NONE',  ( 2.655984681222220721E-16, 17.25312499938548072, 25.66244784525396483 ) ) ;
#15278 = CARTESIAN_POINT ( 'NONE',  ( 15.12187500061451750, -6.054752690667223547, -1.112240025338166033E-15 ) ) ;
#15279 = CARTESIAN_POINT ( 'NONE',  ( 13.32187500061451502, -6.054752690667223547, -1.112240025338166033E-15 ) ) ;
#15280 = CARTESIAN_POINT ( 'NONE',  ( 23.55937500061451573, 0.000000000000000000, 5.243569643749999010 ) ) ;
#15281 = CARTESIAN_POINT ( 'NONE',  ( 4.243569643749999010, 12.92187500061451999, 27.54997392385601174 ) ) ;
#15282 = CARTESIAN_POINT ( 'NONE',  ( 4.115625000614516082, 3.027376345333611329, 5.243569643749999010 ) ) ;
#15283 = CARTESIAN_POINT ( 'NONE',  ( 29.35312500061451502, 0.000000000000000000, 5.243569643749999010 ) ) ;
#15284 = CARTESIAN_POINT ( 'NONE',  ( 26.69062500061451715, -3.027376345333614438, 5.243569643749998122 ) ) ;
#15285 = CARTESIAN_POINT ( 'NONE',  ( 24.93750000122903288, 6.123233995736764310E-16, -4.999999999999998224 ) ) ;
#15286 = CARTESIAN_POINT ( 'NONE',  ( 3.999999999999998668, 19.81250000000000000, 27.69059892324149175 ) ) ;
#15287 = CARTESIAN_POINT ( 'NONE',  ( 7.096875000614517148, -3.027376345333610441, -5.243569643749999898 ) ) ;
#15288 = PRODUCT_CONTEXT ( 'NONE', #11543, 'mechanical' ) ;
#15289 = CARTESIAN_POINT ( 'NONE',  ( 15.03750000122903252, 6.123233995736764310E-16, -4.999999999999998224 ) ) ;
#15290 = CARTESIAN_POINT ( 'NONE',  ( 8.512500001229033941, 0.000000000000000000, 4.999999999999998224 ) ) ;
#15291 = CARTESIAN_POINT ( 'NONE',  ( 5.428125000614517859, 4.541064518000418104, 2.621784821874999949 ) ) ;
#15292 = CARTESIAN_POINT ( 'NONE',  ( -1.999999999999999112, 15.29374999877096641, 26.53589838486224650 ) ) ;
#15293 = CARTESIAN_POINT ( 'NONE',  ( 17.79375000122903572, 5.773502691896255534, 3.535250795749688894E-16 ) ) ;
#15294 = CARTESIAN_POINT ( 'NONE',  ( 13.50937500061451679, 4.541064518000418104, -2.621784821874998173 ) ) ;
#15295 = CARTESIAN_POINT ( 'NONE',  ( 21.28125000122903288, 6.123233995736764310E-16, -4.999999999999998224 ) ) ;
#15296 = ORIENTED_EDGE ( 'NONE', *, *, #16945, .T. ) ;
#15297 = CARTESIAN_POINT ( 'NONE',  ( 19.90312500061451573, 0.000000000000000000, 5.243569643749999010 ) ) ;
#15298 = CARTESIAN_POINT ( 'NONE',  ( 7.940625000614518036, -3.027376345333610441, -5.243569643749999898 ) ) ;
#15299 = CARTESIAN_POINT ( 'NONE',  ( 24.30937500061451573, 4.541064518000418104, -2.621784821874998173 ) ) ;
#15300 = CARTESIAN_POINT ( 'NONE',  ( 8.578125000614518214, 4.541064518000418104, 2.621784821874999949 ) ) ;
#15301 = CARTESIAN_POINT ( 'NONE',  ( 45.00000000000000000, 0.000000000000000000, 4.999999999999998224 ) ) ;
#15303 = ADVANCED_FACE ( 'NONE', ( #4915, #1187 ), #7805, .F. ) ;
#15302 = CARTESIAN_POINT ( 'NONE',  ( 9.150000001229033231, -2.886751345948125991, -5.000000000000000000 ) ) ;
#15304 = CARTESIAN_POINT ( 'NONE',  ( 23.12812500061451360, -4.541064518000419881, 2.621784821874995952 ) ) ;
#15305 = CARTESIAN_POINT ( 'NONE',  ( -2.828200636599751609E-16, 17.30000000122903359, -34.61880215351700230 ) ) ;
#15306 = CARTESIAN_POINT ( 'NONE',  ( 10.01250000122903394, -4.330127018922190985, -2.500000000000001332 ) ) ;
#15307 = CARTESIAN_POINT ( 'NONE',  ( 19.67812500061451786, 6.421520780324663323E-16, -5.243569643749999010 ) ) ;
#15308 = CARTESIAN_POINT ( 'NONE',  ( 16.07812500061451289, 6.421520780324663323E-16, -5.243569643749999010 ) ) ;
#15309 = CARTESIAN_POINT ( 'NONE',  ( 28.09687500061451360, -2.746126346562646425, 4.756430356249996549 ) ) ;
#15310 = CARTESIAN_POINT ( 'NONE',  ( 14.66249999999999964, 2.886751345948126879, 4.999999999999999112 ) ) ;
#15311 = CARTESIAN_POINT ( 'NONE',  ( 12.00000000122903465, 5.773502691896255534, 3.535250795749688894E-16 ) ) ;
#15312 = CARTESIAN_POINT ( 'NONE',  ( 9.178125000614517859, -4.541064518000419881, 2.621784821874995952 ) ) ;
#15313 =( REPRESENTATION_RELATIONSHIP ('NONE','NONE', #33485, #46217 ) REPRESENTATION_RELATIONSHIP_WITH_TRANSFORMATION ( #501 )SHAPE_REPRESENTATION_RELATIONSHIP( ) );
#15314 = CARTESIAN_POINT ( 'NONE',  ( 12.17812500061451608, 4.541064518000418104, 2.621784821874999949 ) ) ;
#15315 = CARTESIAN_POINT ( 'NONE',  ( 23.32500000122903572, 2.886751345948126879, 4.999999999999999112 ) ) ;
#15316 = CARTESIAN_POINT ( 'NONE',  ( 20.07187500061451857, -6.054752690667223547, -1.112240025338166033E-15 ) ) ;
#15317 = CARTESIAN_POINT ( 'NONE',  ( 7.406250001229033764, 4.330127018922192761, -2.499999999999997780 ) ) ;
#15318 = CARTESIAN_POINT ( 'NONE',  ( 4.200000001229033053, -2.886751345948125991, -5.000000000000000000 ) ) ;
#15319 = CARTESIAN_POINT ( 'NONE',  ( 3.459375000614519635, -4.541064518000417216, -2.621784821875001281 ) ) ;
#15320 = CARTESIAN_POINT ( 'NONE',  ( 22.80937500061451573, -4.541064518000417216, -2.621784821875001281 ) ) ;
#15321 = CARTESIAN_POINT ( 'NONE',  ( -1.999999999999999112, 12.65000000000000213, 26.53589838486224650 ) ) ;
#15322 = CARTESIAN_POINT ( 'NONE',  ( 19.45312500061451644, 0.000000000000000000, 5.243569643749999010 ) ) ;
#15323 = CARTESIAN_POINT ( 'NONE',  ( 23.59687500061451715, -3.027376345333614438, 5.243569643749998122 ) ) ;
#15324 = CARTESIAN_POINT ( 'NONE',  ( -7.967954043666661671E-16, 19.84062499938548285, 34.33755215474603517 ) ) ;
#15325 = CARTESIAN_POINT ( 'NONE',  ( 28.65937500061451715, -4.541064518000417216, -2.621784821875001281 ) ) ;
#15326 = CARTESIAN_POINT ( 'NONE',  ( 5.709375000614517859, -4.541064518000417216, -2.621784821875001281 ) ) ;
#15327 = CARTESIAN_POINT ( 'NONE',  ( 14.27812500061451573, 6.421520780324663323E-16, -5.243569643749999010 ) ) ;
#15328 = CARTESIAN_POINT ( 'NONE',  ( 13.62187500061451750, 3.027376345333611329, 5.243569643749999010 ) ) ;
#15329 = ORIENTED_EDGE ( 'NONE', *, *, #57151, .T. ) ;
#15330 = LINE ( 'NONE', #4637, #32466 ) ;
#15331 = CARTESIAN_POINT ( 'NONE',  ( 25.64062500061451644, 6.054752690667223547, 3.707466751127219781E-16 ) ) ;
#15332 = CARTESIAN_POINT ( 'NONE',  ( 3.999999999999998668, 13.06250000000000000, -32.30940107675850470 ) ) ;
#15333 = CARTESIAN_POINT ( 'NONE',  ( -1.071796769724488563, 11.65490381179670010, -26.00000000000000000 ) ) ;
#15334 = EDGE_CURVE ( 'NONE', #9134, #61283, #11898, .T. ) ;
#15335 = CARTESIAN_POINT ( 'NONE',  ( 14.88750000000000107, -2.886751345948125991, -5.000000000000000000 ) ) ;
#15336 = CARTESIAN_POINT ( 'NONE',  ( 25.05000000122903714, 5.773502691896255534, 3.535250795749688894E-16 ) ) ;
#15337 = CARTESIAN_POINT ( 'NONE',  ( 18.96562500061451573, 3.027376345333611329, 5.243569643749999010 ) ) ;
#15338 = ORIENTED_EDGE ( 'NONE', *, *, #24303, .F. ) ;
#15339 = CARTESIAN_POINT ( 'NONE',  ( 23.25000000000000000, 0.000000000000000000, 4.999999999999998224 ) ) ;
#15340 = CARTESIAN_POINT ( 'NONE',  ( 23.67187500061451999, -6.054752690667223547, -1.112240025338166033E-15 ) ) ;
#15341 = ORIENTED_EDGE ( 'NONE', *, *, #42238, .T. ) ;
#15342 = CARTESIAN_POINT ( 'NONE',  ( 1.071873214313479261, 4.999999999999998224, -1.071873214313479261 ) ) ;
#15343 = CARTESIAN_POINT ( 'NONE',  ( 11.39062500061451644, -3.027376345333614438, 5.243569643749998122 ) ) ;
#15344 = CARTESIAN_POINT ( 'NONE',  ( 4.003125000614518925, 4.541064518000418104, -2.621784821874998173 ) ) ;
#15345 = CARTESIAN_POINT ( 'NONE',  ( 15.08437500061451431, -2.746126346562642428, -4.756430356249999214 ) ) ;
#15346 = CARTESIAN_POINT ( 'NONE',  ( 26.05312500061451431, 4.541064518000418104, -2.621784821874998173 ) ) ;
#15347 = CARTESIAN_POINT ( 'NONE',  ( 17.39999999999999858, 0.000000000000000000, 4.999999999999998224 ) ) ;
#15348 = CARTESIAN_POINT ( 'NONE',  ( 24.86250000000000071, 2.886751345948129099, -4.999999999999998224 ) ) ;
#15349 = CARTESIAN_POINT ( 'NONE',  ( 7.650000001229034119, -2.886751345948130876, 4.999999999999996447 ) ) ;
#15350 = CARTESIAN_POINT ( 'NONE',  ( 6.084375000614518747, -4.541064518000419881, 2.621784821874995952 ) ) ;
#15351 = CARTESIAN_POINT ( 'NONE',  ( 16.62187500061451573, 3.027376345333613106, -5.243569643749998122 ) ) ;
#15352 = CARTESIAN_POINT ( 'NONE',  ( 28.50937500061451502, 0.000000000000000000, 5.243569643749999010 ) ) ;
#15353 = ORIENTED_EDGE ( 'NONE', *, *, #14141, .F. ) ;
#15354 = CARTESIAN_POINT ( 'NONE',  ( 25.97812500061451502, 6.421520780324663323E-16, -5.243569643749999010 ) ) ;
#15355 = CARTESIAN_POINT ( 'NONE',  ( 28.62187500061451573, -6.054752690667223547, -1.112240025338166033E-15 ) ) ;
#15356 = CARTESIAN_POINT ( 'NONE',  ( 3.421875000614516882, -6.054752690667223547, -1.112240025338166033E-15 ) ) ;
#15357 = CARTESIAN_POINT ( 'NONE',  ( 13.38750000000000107, -2.886751345948129988, 4.999999999999997335 ) ) ;
#15358 = CARTESIAN_POINT ( 'NONE',  ( 10.19062500061451892, -3.027376345333610441, -5.243569643749999898 ) ) ;
#15359 = CARTESIAN_POINT ( 'NONE',  ( 9.468750001229032875, -5.773502691896255534, -1.060575238724906372E-15 ) ) ;
#15360 = DIRECTION ( 'NONE',  ( 0.000000000000000000, 0.000000000000000000, -1.000000000000000000 ) ) ;
#15361 = CARTESIAN_POINT ( 'NONE',  ( 28.86562500061451786, 3.027376345333611329, 5.243569643749999010 ) ) ;
#15362 = CARTESIAN_POINT ( 'NONE',  ( 16.20000000122903216, -2.886751345948129988, 4.999999999999997335 ) ) ;
#15363 = CARTESIAN_POINT ( 'NONE',  ( 30.00000000000000000, 0.000000000000000000, 0.000000000000000000 ) ) ;
#15364 = CARTESIAN_POINT ( 'NONE',  ( 16.32187500061451502, 2.746126346562643317, 4.756430356249998326 ) ) ;
#15365 = CARTESIAN_POINT ( 'NONE',  ( 5.690625000614516260, -3.027376345333610441, -5.243569643749999898 ) ) ;
#15366 = CARTESIAN_POINT ( 'NONE',  ( 22.69687500061451857, -3.027376345333614438, 5.243569643749998122 ) ) ;
#15368 = CARTESIAN_POINT ( 'NONE',  ( -4.243569643749999898, 16.25937500061451857, 30.00000000000000000 ) ) ;
#15367 =( BOUNDED_CURVE ( )  B_SPLINE_CURVE ( 2, ( #23590, #50594, #40232, #39144, #57201, #11790, #17320 ),
 .UNSPECIFIED., .F., .F. ) 
 B_SPLINE_CURVE_WITH_KNOTS ( ( 3, 2, 2, 3 ),
 ( 0.2166666666666667296, 0.2194444444444444975, 0.2222222222222222654, 0.2250000000000000611 ),
 .UNSPECIFIED. ) 
 CURVE ( )  GEOMETRIC_REPRESENTATION_ITEM ( )  RATIONAL_B_SPLINE_CURVE ( ( 0.9999999999999973355, 0.8660254037844413721, 1.000000000000000000, 0.8660254037844387076, 1.000000000000000000, 0.8660254037844360431, 1.000000000000002665 ) ) 
 REPRESENTATION_ITEM ( '' )  );
#15369 = CARTESIAN_POINT ( 'NONE',  ( 22.43437500061451573, 6.421520780324663323E-16, -5.243569643749999010 ) ) ;
#15370 = CARTESIAN_POINT ( 'NONE',  ( 4.125000000000000000, 6.123233995736764310E-16, -4.999999999999998224 ) ) ;
#15371 = CARTESIAN_POINT ( 'NONE',  ( -3.999999999999999556, 9.725000001229034297, 27.69059892324149530 ) ) ;
#15372 = CARTESIAN_POINT ( 'NONE',  ( 12.74062500061451786, -3.027376345333614438, 5.243569643749998122 ) ) ;
#15373 = CARTESIAN_POINT ( 'NONE',  ( 5.212500001229032343, 4.330127018922192761, -2.499999999999997780 ) ) ;
#15374 = CARTESIAN_POINT ( 'NONE',  ( 9.196875000614518569, -3.027376345333614438, 5.243569643749998122 ) ) ;
#15375 = CARTESIAN_POINT ( 'NONE',  ( 13.18125000122903323, 6.123233995736764310E-16, -4.999999999999998224 ) ) ;
#15376 = CARTESIAN_POINT ( 'NONE',  ( 9.065625000614517148, 3.027376345333611329, 5.243569643749999010 ) ) ;
#15377 = CARTESIAN_POINT ( 'NONE',  ( 15.08437500061451786, -4.541064518000419881, 2.621784821874995952 ) ) ;
#15378 = CARTESIAN_POINT ( 'NONE',  ( -2.498395430326213790E-14, 18.91249999999999787, 26.00000000000000000 ) ) ;
#15379 = CARTESIAN_POINT ( 'NONE',  ( 21.30000000122903359, -2.886751345948125991, -5.000000000000000000 ) ) ;
#15380 = CARTESIAN_POINT ( 'NONE',  ( 7.621875000614519280, 3.027376345333613106, -5.243569643749998122 ) ) ;
#15381 = CARTESIAN_POINT ( 'NONE',  ( 11.27812500061451573, 4.541064518000418104, 2.621784821874999949 ) ) ;
#15382 = CARTESIAN_POINT ( 'NONE',  ( 26.41875000122903216, 2.886751345948126879, 4.999999999999999112 ) ) ;
#15383 = CARTESIAN_POINT ( 'NONE',  ( 22.32187500061451502, -6.054752690667223547, -1.112240025338166033E-15 ) ) ;
#15384 = LINE ( 'NONE', #3592, #7753 ) ;
#15385 = CARTESIAN_POINT ( 'NONE',  ( -3.457895701286862966, 3.616202803579614322, 32.02583422746450026 ) ) ;
#15386 = EDGE_CURVE ( 'NONE', #62948, #29428, #67665, .T. ) ;
#15387 = CARTESIAN_POINT ( 'NONE',  ( -3.000416591977282496E-16, 12.54687500061451999, -34.90005215228797653 ) ) ;
#15388 = CARTESIAN_POINT ( 'NONE',  ( 14.81250000122903288, 0.000000000000000000, 4.999999999999998224 ) ) ;
#15389 = CARTESIAN_POINT ( 'NONE',  ( -4.243569643749997233, 18.94062500061451715, -27.54997392385601174 ) ) ;
#15390 = CARTESIAN_POINT ( 'NONE',  ( 16.50000000122903288, 5.773502691896255534, 3.535250795749688894E-16 ) ) ;
#15391 = CARTESIAN_POINT ( 'NONE',  ( 10.15312500061451750, -4.541064518000417216, -2.621784821875001281 ) ) ;
#15392 = ORIENTED_EDGE ( 'NONE', *, *, #30954, .F. ) ;
#15393 = CARTESIAN_POINT ( 'NONE',  ( 15.03749999999999964, 5.773502691896255534, 3.535250795749688894E-16 ) ) ;
#15394 = CARTESIAN_POINT ( 'NONE',  ( 10.42500000122903181, -5.773502691896255534, -1.060575238724906372E-15 ) ) ;
#15395 = CARTESIAN_POINT ( 'NONE',  ( 22.49062500061451431, 6.054752690667223547, 3.707466751127219781E-16 ) ) ;
#15396 = CARTESIAN_POINT ( 'NONE',  ( 10.24687500061451573, -3.027376345333610441, -5.243569643749999898 ) ) ;
#15397 = CARTESIAN_POINT ( 'NONE',  ( 4.351407642015760580, -2.462831795607901775, -4.629229178597866756 ) ) ;
#15398 = CARTESIAN_POINT ( 'NONE',  ( 9.300000001229035362, 5.773502691896255534, 3.535250795749688894E-16 ) ) ;
#15399 = CARTESIAN_POINT ( 'NONE',  ( 17.92500000122903359, 2.886751345948126879, 4.999999999999999112 ) ) ;
#15400 = CARTESIAN_POINT ( 'NONE',  ( 15.74062500061451608, 6.054752690667223547, 3.707466751127219781E-16 ) ) ;
#15401 = CARTESIAN_POINT ( 'NONE',  ( 18.44062500061451715, 6.054752690667223547, 3.707466751127219781E-16 ) ) ;
#15402 = CARTESIAN_POINT ( 'NONE',  ( 26.36250000122903003, 4.330127018922192761, -2.499999999999997780 ) ) ;
#15403 = CARTESIAN_POINT ( 'NONE',  ( 29.43750000122903288, 6.123233995736764310E-16, -4.999999999999998224 ) ) ;
#15404 = CARTESIAN_POINT ( 'NONE',  ( 24.60000000000000142, 0.000000000000000000, 4.999999999999998224 ) ) ;
#15405 = CARTESIAN_POINT ( 'NONE',  ( -3.756430356249999214, 14.62812499938548250, 27.83122392262697531 ) ) ;
#15406 = CARTESIAN_POINT ( 'NONE',  ( 25.88437500061451502, -4.541064518000419881, 2.621784821874995952 ) ) ;
#15407 = CARTESIAN_POINT ( 'NONE',  ( -1.071796769724491005, 15.85759618943233207, 26.00000000000000355 ) ) ;
#15408 = CARTESIAN_POINT ( 'NONE',  ( 12.52500000122903145, 2.886751345948126879, 4.999999999999999112 ) ) ;
#15409 = CARTESIAN_POINT ( 'NONE',  ( 3.450000000000001510, 0.000000000000000000, 4.999999999999998224 ) ) ;
#15410 =( BOUNDED_CURVE ( )  B_SPLINE_CURVE ( 2, ( #10924, #61892, #11297, #50459, #39743, #56361, #40102, #62615, #32735, #5751, #28285, #22009, #219, #55272, #4667, #33093, #45277, #67810, #27197, #49732, #72259, #44194, #66725, #38646, #44565, #68535, #18621, #2028, #68894, #1299, #24172, #40824, #52622, #41186, #7194, #17896, #34535, #57065, #12368, #62972, #45998, #23452, #6834, #13438, #30084, #18251, #12727, #58144, #6472, #52260, #23809, #24539, #34903, #46724, #29007, #51544, #945, #63341, #35988, #35263, #46360, #63695, #7550, #51901, #47083, #41540, #57785, #40456, #13086, #69259, #29722, #57430, #35624, #29369, #1663, #69617, #18979, #64058, #12012, #23316, #16326, #67678, #4894, #34404, #45511, #68399, #809, #67326, #27428, #45865, #17760, #27795, #45145, #61398, #40320, #66960, #441, #62842, #12235, #51045, #34765, #5977, #11519, #22951, #72484, #17049, #49960, #39606, #33684, #56932, #28158, #68041, #5253, #16686, #6336, #28507, #11159, #50332, #28867, #44432, #51406, #38879, #55864, #10791, #22594, #33326, #72856, #22238, #56580, #61756, #62127, #34041, #50686, #62482, #39242, #21870, #44793, #56229, #17411, #39968, #5622, #89, #11880, #1532, #12601, #2606, #42135, #6704, #64661, #35133, #46225, #1169, #29237, #19579, #57658, #2250, #30678, #7421, #63568, #58373, #29949, #7064, #29592, #24039, #52129, #68764, #58740, #41055, #14046, #57299, #18122, #46589, #51770, #36224, #52489, #24404, #64293, #23678, #13311, #12956, #8151, #7785, #40687, #63204, #69131, #1900, #18489, #58013, #35493, #46953, #69490, #18849, #53210, #41410, #63926, #35850, #52852, #30322, #47309, #24766, #69843, #19209, #41764, #13680, #25128, #47669, #70204, #54865, #10167, #67774, #72587, #67421, #5354, #28251, #33783, #27163, #60387, #5715, #50782, #60759, #4992, #67062, #39341, #44886, #27892, #50426, #185, #4273, #21603, #38977, #44529, #10890, #32328, #27524, #22690, #50057, #66686, #16783, #61133, #33418, #38229, #56326, #26797, #9795, #61493, #21235, #55238, #38610, #49331, #22334, #45241, #44157, #4633, #66314, #37868, #71863, #43787, #15691, #32701, #49697, #72224, #61853, #16419, #16061, #10530, #55958, #33058, #55597, #21970, #72952, #11261, #40067, #57029, #11978, #6074, #18586, #908, #47047, #17149, #51143, #6435, #7159, #39707, #62225, #68859, #17860, #23416, #24503, #11621, #52586, #542, #6799, #13050, #45608, #18215, #23053, #28970, #35230, #46687, #29688, #69225, #63659, #68142, #51508, #45963, #12693, #34137, #52225, #40788, #17506, #62581, #41151, #51863, #63301, #1992, #35589, #34501, #56676, #68496, #28607, #1265, #40419, #58108, #62936, #23772, #12329, #34865, #1629, #57751, #57392, #7515, #46324, #30046, #24136, #29333, #59569, #37418, #13401, #53308, #70665, #3075, #3816, #59202, #54056, #14879, #71037, #31139, #25603, #20041, #48141, #42596, #65489, #35948, #18943, #65122, #52946, #13780, #70305, #14146, #30418, #47407, #58469, #2343, #64390, #64022, #69937, #19307, #42231, #14512, #20412, #9348, #7882, #37045, #48510, #41860, #24860, #36322, #26337, #53680, #25969, #8983, #58837, #31515, #8247, #30777, #3451, #42960, #41502, #59941, #31881, #54415, #69581, #2707, #25223, #47769, #19678, #64756, #36681, #8610, #21879, #43337, #33336, #67335, #50341, #10441, #4904, #49970, #27440, #55511, #44802, #15241, #71406, #72494, #32243, #66222, #49606, #66594, #9709, #26710, #54776, #44440, #43701, #65859, #49244, #71779, #21513, #66969, #72865, #61765, #37778, #16334, #60298, #55874, #16695, #55148, #15600, #4181, #39253, #33693, #20781, #56239, #21147, #38142, #38889, #5261, #61407, #60666, #10079, #10801, #32610, #4546, #15970, #27075, #72133, #44066, #38520, #61043, #32971, #22248, #27805, #5631, #11169, #48876, #17770, #18130, #50695, #58022, #6713, #28877, #11889, #35503, #22603, #63578, #11529, #40330, #24051, #56590, #29246, #34050, #68051, #46234, #40697, #57667, #34414, #7073, #41064, #56942, #5986, #68774, #1178, #34776, #28516, #12610, #67687, #51056, #63214, #35144, #451, #97, #45155, #22960, #28168, #17058, #62136, #17420, #12965, #29602, #51416, #68408, #52138, #39617, #57308, #6346, #1541, #45520, #51778, #39979, #62491, #818, #23326, #45876, #46598, #69140, #18499, #62851, #12245, #23686, #20323, #36236, #13321, #25513, #53590, #14057, #35860, #65035, #46963, #58383, #48058, #19959, #70215, #30689, #24414, #52862, #37332, #42145, #36961, #70583, #70952, #3365, #69853, #29958, #48426, #42877, #30334, #47679, #63936, #65400, #69499, #2985, #14791, #7432, #18859, #64303, #8524, #36596, #42511, #1909, #19589, #52499, #64672, #58750, #59483, #53220, #14426, #7795, #19220, #8895, #31053, #13692, #2262, #31427, #8160, #25138, #41420, #24776, #47320, #59117, #2617, #53967, #25886, #41774, #44356, #21064, #38805, #50255, #72778, #38430, #49522, #9626, #9990, #16249 ),
 .UNSPECIFIED., .F., .F. ) 
 B_SPLINE_CURVE_WITH_KNOTS ( ( 3, 2, 2, 2, 2, 2, 2, 2, 2, 2, 2, 2, 2, 2, 2, 2, 2, 2, 2, 2, 2, 2, 2, 2, 2, 2, 2, 2, 2, 2, 2, 2, 2, 2, 2, 2, 2, 2, 2, 2, 2, 2, 2, 2, 2, 2, 2, 2, 2, 2, 2, 2, 2, 2, 2, 2, 2, 2, 2, 2, 2, 2, 2, 2, 2, 2, 2, 2, 2, 2, 2, 2, 2, 2, 2, 2, 2, 2, 2, 2, 2, 2, 2, 2, 2, 2, 2, 2, 2, 2, 2, 2, 2, 2, 2, 2, 2, 2, 2, 2, 2, 2, 2, 2, 2, 2, 2, 2, 2, 2, 2, 2, 2, 2, 2, 2, 2, 2, 2, 2, 2, 2, 2, 2, 2, 2, 2, 2, 2, 2, 2, 2, 2, 2, 2, 2, 2, 2, 2, 2, 2, 2, 2, 2, 2, 2, 2, 2, 2, 2, 2, 2, 2, 2, 2, 2, 2, 2, 2, 2, 2, 2, 2, 2, 2, 2, 2, 2, 2, 2, 2, 2, 2, 2, 2, 2, 2, 2, 2, 2, 2, 2, 2, 2, 2, 2, 2, 2, 2, 2, 2, 2, 2, 2, 2, 2, 2, 2, 2, 2, 2, 2, 2, 2, 2, 2, 2, 2, 2, 2, 2, 2, 2, 2, 2, 2, 2, 2, 2, 2, 2, 2, 2, 2, 2, 2, 2, 2, 2, 2, 2, 2, 2, 2, 2, 2, 2, 2, 2, 2, 2, 2, 2, 2, 2, 2, 2, 2, 2, 2, 2, 2, 2, 2, 2, 2, 2, 2, 2, 2, 2, 2, 2, 2, 2, 2, 2, 2, 2, 2, 2, 2, 2, 2, 2, 2, 2, 2, 2, 2, 2, 2, 2, 2, 2, 2, 2, 2, 2, 2, 2, 2, 2, 2, 2, 2, 2, 2, 2, 2, 3 ),
 ( 0.000000000000000000, 0.003333333333333333547, 0.006666666666666667095, 0.01000000000000000021, 0.01333333333333333419, 0.01666666666666666644, 0.02000000000000000042, 0.02333333333333333440, 0.02666666666666666838, 0.02999999999999999889, 0.03333333333333333287, 0.03666666666666666685, 0.04000000000000000083, 0.04333333333333333481, 0.04666666666666666879, 0.05000000000000000278, 0.05333333333333333676, 0.05666666666666666380, 0.05999999999999999778, 0.06333333333333333870, 0.06666666666666666574, 0.07000000000000000666, 0.07333333333333333370, 0.07666666666666666075, 0.08000000000000000167, 0.08333333333333332871, 0.08666666666666666963, 0.08999999999999999667, 0.09333333333333333759, 0.09666666666666666463, 0.1000000000000000056, 0.1033333333333333326, 0.1066666666666666735, 0.1100000000000000006, 0.1133333333333333276, 0.1166666666666666685, 0.1199999999999999956, 0.1233333333333333365, 0.1266666666666666774, 0.1300000000000000044, 0.1333333333333333315, 0.1366666666666666585, 0.1400000000000000133, 0.1433333333333333404, 0.1466666666666666674, 0.1499999999999999944, 0.1533333333333333215, 0.1566666666666666763, 0.1600000000000000033, 0.1633333333333333304, 0.1666666666666666574, 0.1700000000000000122, 0.1733333333333333393, 0.1766666666666666663, 0.1799999999999999933, 0.1833333333333333204, 0.1866666666666666752, 0.1900000000000000022, 0.1933333333333333293, 0.1966666666666666563, 0.2000000000000000111, 0.2033333333333333381, 0.2066666666666666652, 0.2099999999999999922, 0.2133333333333333470, 0.2166666666666666741, 0.2200000000000000011, 0.2233333333333333282, 0.2266666666666666552, 0.2300000000000000100, 0.2333333333333333370, 0.2366666666666666641, 0.2399999999999999911, 0.2433333333333333459, 0.2466666666666666730, 0.2500000000000000000, 0.2533333333333333548, 0.2566666666666666541, 0.2600000000000000089, 0.2633333333333333082, 0.2666666666666666630, 0.2700000000000000178, 0.2733333333333333171, 0.2766666666666666718, 0.2800000000000000266, 0.2833333333333333259, 0.2866666666666666807, 0.2899999999999999800, 0.2933333333333333348, 0.2966666666666666896, 0.2999999999999999889, 0.3033333333333333437, 0.3066666666666666430, 0.3099999999999999978, 0.3133333333333333526, 0.3166666666666666519, 0.3200000000000000067, 0.3233333333333333059, 0.3266666666666666607, 0.3300000000000000155, 0.3333333333333333148, 0.3366666666666666696, 0.3400000000000000244, 0.3433333333333333237, 0.3466666666666666785, 0.3499999999999999778, 0.3533333333333333326, 0.3566666666666666874, 0.3599999999999999867, 0.3633333333333333415, 0.3666666666666666408, 0.3699999999999999956, 0.3733333333333333504, 0.3766666666666666496, 0.3800000000000000044, 0.3833333333333333592, 0.3866666666666666585, 0.3900000000000000133, 0.3933333333333333126, 0.3966666666666666674, 0.4000000000000000222, 0.4033333333333333215, 0.4066666666666666763, 0.4099999999999999756, 0.4133333333333333304, 0.4166666666666666852, 0.4199999999999999845, 0.4233333333333333393, 0.4266666666666666941, 0.4299999999999999933, 0.4333333333333333481, 0.4366666666666666474, 0.4400000000000000022, 0.4433333333333333570, 0.4466666666666666563, 0.4500000000000000111, 0.4533333333333333104, 0.4566666666666666652, 0.4600000000000000200, 0.4633333333333333193, 0.4666666666666666741, 0.4699999999999999734, 0.4733333333333333282, 0.4766666666666666829, 0.4799999999999999822, 0.4833333333333333370, 0.4866666666666666918, 0.4899999999999999911, 0.4933333333333333459, 0.4966666666666666452, 0.5000000000000000000, 0.5033333333333332993, 0.5066666666666667096, 0.5100000000000000089, 0.5133333333333333082, 0.5166666666666667185, 0.5200000000000000178, 0.5233333333333333171, 0.5266666666666666163, 0.5300000000000000266, 0.5333333333333333259, 0.5366666666666666252, 0.5400000000000000355, 0.5433333333333333348, 0.5466666666666666341, 0.5500000000000000444, 0.5533333333333333437, 0.5566666666666666430, 0.5600000000000000533, 0.5633333333333333526, 0.5666666666666666519, 0.5699999999999999512, 0.5733333333333333615, 0.5766666666666666607, 0.5799999999999999600, 0.5833333333333333703, 0.5866666666666666696, 0.5899999999999999689, 0.5933333333333333792, 0.5966666666666666785, 0.5999999999999999778, 0.6033333333333333881, 0.6066666666666666874, 0.6099999999999999867, 0.6133333333333332860, 0.6166666666666666963, 0.6199999999999999956, 0.6233333333333332948, 0.6266666666666667052, 0.6300000000000000044, 0.6333333333333333037, 0.6366666666666667140, 0.6400000000000000133, 0.6433333333333333126, 0.6466666666666666119, 0.6500000000000000222, 0.6533333333333333215, 0.6566666666666666208, 0.6600000000000000311, 0.6633333333333333304, 0.6666666666666666297, 0.6700000000000000400, 0.6733333333333333393, 0.6766666666666666385, 0.6800000000000000488, 0.6833333333333333481, 0.6866666666666666474, 0.6899999999999999467, 0.6933333333333333570, 0.6966666666666666563, 0.6999999999999999556, 0.7033333333333333659, 0.7066666666666666652, 0.7099999999999999645, 0.7133333333333333748, 0.7166666666666666741, 0.7199999999999999734, 0.7233333333333333837, 0.7266666666666666829, 0.7299999999999999822, 0.7333333333333332815, 0.7366666666666666918, 0.7399999999999999911, 0.7433333333333332904, 0.7466666666666667007, 0.7500000000000000000, 0.7533333333333332993, 0.7566666666666667096, 0.7600000000000000089, 0.7633333333333333082, 0.7666666666666667185, 0.7700000000000000178, 0.7733333333333333171, 0.7766666666666666163, 0.7800000000000000266, 0.7833333333333333259, 0.7866666666666666252, 0.7900000000000000355, 0.7933333333333333348, 0.7966666666666666341, 0.8000000000000000444, 0.8033333333333333437, 0.8066666666666666430, 0.8100000000000000533, 0.8133333333333333526, 0.8166666666666666519, 0.8199999999999999512, 0.8233333333333333615, 0.8266666666666666607, 0.8299999999999999600, 0.8333333333333333703, 0.8366666666666666696, 0.8399999999999999689, 0.8433333333333333792, 0.8466666666666666785, 0.8499999999999999778, 0.8533333333333333881, 0.8566666666666666874, 0.8599999999999999867, 0.8633333333333332860, 0.8666666666666666963, 0.8699999999999999956, 0.8733333333333332948, 0.8766666666666667052, 0.8800000000000000044, 0.8833333333333333037, 0.8866666666666667140, 0.8900000000000000133, 0.8933333333333333126, 0.8966666666666666119, 0.9000000000000000222, 0.9033333333333333215, 0.9066666666666666208, 0.9100000000000000311, 0.9133333333333333304, 0.9166666666666666297, 0.9200000000000000400, 0.9233333333333333393, 0.9266666666666666385, 0.9300000000000000488, 0.9333333333333333481, 0.9366666666666666474, 0.9399999999999999467, 0.9433333333333333570, 0.9466666666666666563, 0.9499999999999999556, 0.9533333333333333659, 0.9566666666666666652, 0.9599999999999999645, 0.9633333333333333748, 0.9666666666666666741, 0.9699999999999999734, 0.9733333333333333837, 0.9766666666666666829, 0.9799999999999999822, 0.9833333333333332815, 0.9866666666666666918, 0.9899999999999999911, 0.9933333333333332904, 0.9966666666666667007, 1.000000000000000000 ),
 .UNSPECIFIED. ) 
 CURVE ( )  GEOMETRIC_REPRESENTATION_ITEM ( )  RATIONAL_B_SPLINE_CURVE ( ( 1.000000000000000000, 0.8660254037844387076, 1.000000000000000000, 0.8660254037844387076, 1.000000000000000000, 0.8660254037844387076, 1.000000000000000000, 0.8660254037844387076, 1.000000000000000000, 0.8660254037844387076, 1.000000000000000000, 0.8660254037844387076, 1.000000000000000000, 0.8660254037844387076, 1.000000000000000000, 0.8660254037844387076, 1.000000000000000000, 0.8660254037844387076, 1.000000000000000000, 0.8660254037844387076, 1.000000000000000000, 0.8660254037844387076, 1.000000000000000000, 0.8660254037844387076, 1.000000000000000000, 0.8660254037844387076, 1.000000000000000000, 0.8660254037844387076, 1.000000000000000000, 0.8660254037844387076, 1.000000000000000000, 0.8660254037844387076, 1.000000000000000000, 0.8660254037844387076, 1.000000000000000000, 0.8660254037844387076, 1.000000000000000000, 0.8660254037844387076, 1.000000000000000000, 0.8660254037844387076, 1.000000000000000000, 0.8660254037844387076, 1.000000000000000000, 0.8660254037844387076, 1.000000000000000000, 0.8660254037844387076, 1.000000000000000000, 0.8660254037844387076, 1.000000000000000000, 0.8660254037844387076, 1.000000000000000000, 0.8660254037844387076, 1.000000000000000000, 0.8660254037844387076, 1.000000000000000000, 0.8660254037844387076, 1.000000000000000000, 0.8660254037844387076, 1.000000000000000000, 0.8660254037844387076, 1.000000000000000000, 0.8660254037844387076, 1.000000000000000000, 0.8660254037844387076, 1.000000000000000000, 0.8660254037844387076, 1.000000000000000000, 0.8660254037844387076, 1.000000000000000000, 0.8660254037844387076, 1.000000000000000000, 0.8660254037844387076, 1.000000000000000000, 0.8660254037844387076, 1.000000000000000000, 0.8660254037844387076, 1.000000000000000000, 0.8660254037844387076, 1.000000000000000000, 0.8660254037844387076, 1.000000000000000000, 0.8660254037844387076, 1.000000000000000000, 0.8660254037844387076, 1.000000000000000000, 0.8660254037844387076, 1.000000000000000000, 0.8660254037844387076, 1.000000000000000000, 0.8660254037844387076, 1.000000000000000000, 0.8660254037844387076, 1.000000000000000000, 0.8660254037844387076, 1.000000000000000000, 0.8660254037844387076, 1.000000000000000000, 0.8660254037844387076, 1.000000000000000000, 0.8660254037844387076, 1.000000000000000000, 0.8660254037844387076, 1.000000000000000000, 0.8660254037844387076, 1.000000000000000000, 0.8660254037844387076, 1.000000000000000000, 0.8660254037844387076, 1.000000000000000000, 0.8660254037844387076, 1.000000000000000000, 0.8660254037844387076, 1.000000000000000000, 0.8660254037844387076, 1.000000000000000000, 0.8660254037844387076, 1.000000000000000000, 0.8660254037844387076, 1.000000000000000000, 0.8660254037844387076, 1.000000000000000000, 0.8660254037844387076, 1.000000000000000000, 0.8660254037844387076, 1.000000000000000000, 0.8660254037844387076, 1.000000000000000000, 0.8660254037844387076, 1.000000000000000000, 0.8660254037844387076, 1.000000000000000000, 0.8660254037844387076, 1.000000000000000000, 0.8660254037844387076, 1.000000000000000000, 0.8660254037844387076, 1.000000000000000000, 0.8660254037844387076, 1.000000000000000000, 0.8660254037844387076, 1.000000000000000000, 0.8660254037844387076, 1.000000000000000000, 0.8660254037844387076, 1.000000000000000000, 0.8660254037844387076, 1.000000000000000000, 0.8660254037844387076, 1.000000000000000000, 0.8660254037844387076, 1.000000000000000000, 0.8660254037844387076, 1.000000000000000000, 0.8660254037844387076, 1.000000000000000000, 0.8660254037844387076, 1.000000000000000000, 0.8660254037844387076, 1.000000000000000000, 0.8660254037844387076, 1.000000000000000000, 0.8660254037844387076, 1.000000000000000000, 0.8660254037844387076, 1.000000000000000000, 0.8660254037844387076, 1.000000000000000000, 0.8660254037844387076, 1.000000000000000000, 0.8660254037844387076, 1.000000000000000000, 0.8660254037844387076, 1.000000000000000000, 0.8660254037844387076, 1.000000000000000000, 0.8660254037844387076, 1.000000000000000000, 0.8660254037844387076, 1.000000000000000000, 0.8660254037844387076, 1.000000000000000000, 0.8660254037844387076, 1.000000000000000000, 0.8660254037844387076, 1.000000000000000000, 0.8660254037844387076, 1.000000000000000000, 0.8660254037844387076, 1.000000000000000000, 0.8660254037844387076, 1.000000000000000000, 0.8660254037844387076, 1.000000000000000000, 0.8660254037844387076, 1.000000000000000000, 0.8660254037844387076, 1.000000000000000000, 0.8660254037844387076, 1.000000000000000000, 0.8660254037844387076, 1.000000000000000000, 0.8660254037844387076, 1.000000000000000000, 0.8660254037844387076, 1.000000000000000000, 0.8660254037844387076, 1.000000000000000000, 0.8660254037844387076, 1.000000000000000000, 0.8660254037844387076, 1.000000000000000000, 0.8660254037844387076, 1.000000000000000000, 0.8660254037844387076, 1.000000000000000000, 0.8660254037844387076, 1.000000000000000000, 0.8660254037844387076, 1.000000000000000000, 0.8660254037844387076, 1.000000000000000000, 0.8660254037844387076, 1.000000000000000000, 0.8660254037844387076, 1.000000000000000000, 0.8660254037844387076, 1.000000000000000000, 0.8660254037844387076, 1.000000000000000000, 0.8660254037844387076, 1.000000000000000000, 0.8660254037844387076, 1.000000000000000000, 0.8660254037844387076, 1.000000000000000000, 0.8660254037844387076, 1.000000000000000000, 0.8660254037844387076, 1.000000000000000000, 0.8660254037844387076, 1.000000000000000000, 0.8660254037844387076, 1.000000000000000000, 0.8660254037844387076, 1.000000000000000000, 0.8660254037844387076, 1.000000000000000000, 0.8660254037844387076, 1.000000000000000000, 0.8660254037844387076, 1.000000000000000000, 0.8660254037844387076, 1.000000000000000000, 0.8660254037844387076, 1.000000000000000000, 0.8660254037844387076, 1.000000000000000000, 0.8660254037844387076, 1.000000000000000000, 0.8660254037844387076, 1.000000000000000000, 0.8660254037844387076, 1.000000000000000000, 0.8660254037844387076, 1.000000000000000000, 0.8660254037844387076, 1.000000000000000000, 0.8660254037844387076, 1.000000000000000000, 0.8660254037844387076, 1.000000000000000000, 0.8660254037844387076, 1.000000000000000000, 0.8660254037844387076, 1.000000000000000000, 0.8660254037844387076, 1.000000000000000000, 0.8660254037844387076, 1.000000000000000000, 0.8660254037844387076, 1.000000000000000000, 0.8660254037844387076, 1.000000000000000000, 0.8660254037844387076, 1.000000000000000000, 0.8660254037844387076, 1.000000000000000000, 0.8660254037844387076, 1.000000000000000000, 0.8660254037844387076, 1.000000000000000000, 0.8660254037844387076, 1.000000000000000000, 0.8660254037844387076, 1.000000000000000000, 0.8660254037844387076, 1.000000000000000000, 0.8660254037844387076, 1.000000000000000000, 0.8660254037844387076, 1.000000000000000000, 0.8660254037844387076, 1.000000000000000000, 0.8660254037844387076, 1.000000000000000000, 0.8660254037844387076, 1.000000000000000000, 0.8660254037844387076, 1.000000000000000000, 0.8660254037844387076, 1.000000000000000000, 0.8660254037844387076, 1.000000000000000000, 0.8660254037844387076, 1.000000000000000000, 0.8660254037844387076, 1.000000000000000000, 0.8660254037844387076, 1.000000000000000000, 0.8660254037844387076, 1.000000000000000000, 0.8660254037844387076, 1.000000000000000000, 0.8660254037844387076, 1.000000000000000000, 0.8660254037844387076, 1.000000000000000000, 0.8660254037844387076, 1.000000000000000000, 0.8660254037844387076, 1.000000000000000000, 0.8660254037844387076, 1.000000000000000000, 0.8660254037844387076, 1.000000000000000000, 0.8660254037844387076, 1.000000000000000000, 0.8660254037844387076, 1.000000000000000000, 0.8660254037844387076, 1.000000000000000000, 0.8660254037844387076, 1.000000000000000000, 0.8660254037844387076, 1.000000000000000000, 0.8660254037844387076, 1.000000000000000000, 0.8660254037844387076, 1.000000000000000000, 0.8660254037844387076, 1.000000000000000000, 0.8660254037844387076, 1.000000000000000000, 0.8660254037844387076, 1.000000000000000000, 0.8660254037844387076, 1.000000000000000000, 0.8660254037844387076, 1.000000000000000000, 0.8660254037844387076, 1.000000000000000000, 0.8660254037844387076, 1.000000000000000000, 0.8660254037844387076, 1.000000000000000000, 0.8660254037844387076, 1.000000000000000000, 0.8660254037844387076, 1.000000000000000000, 0.8660254037844387076, 1.000000000000000000, 0.8660254037844387076, 1.000000000000000000, 0.8660254037844387076, 1.000000000000000000, 0.8660254037844387076, 1.000000000000000000, 0.8660254037844387076, 1.000000000000000000, 0.8660254037844387076, 1.000000000000000000, 0.8660254037844387076, 1.000000000000000000, 0.8660254037844387076, 1.000000000000000000, 0.8660254037844387076, 1.000000000000000000, 0.8660254037844387076, 1.000000000000000000, 0.8660254037844387076, 1.000000000000000000, 0.8660254037844387076, 1.000000000000000000, 0.8660254037844387076, 1.000000000000000000, 0.8660254037844387076, 1.000000000000000000, 0.8660254037844387076, 1.000000000000000000, 0.8660254037844387076, 1.000000000000000000, 0.8660254037844387076, 1.000000000000000000, 0.8660254037844387076, 1.000000000000000000, 0.8660254037844387076, 1.000000000000000000, 0.8660254037844387076, 1.000000000000000000, 0.8660254037844387076, 1.000000000000000000, 0.8660254037844387076, 1.000000000000000000, 0.8660254037844387076, 1.000000000000000000, 0.8660254037844387076, 1.000000000000000000, 0.8660254037844387076, 1.000000000000000000, 0.8660254037844387076, 1.000000000000000000, 0.8660254037844387076, 1.000000000000000000, 0.8660254037844387076, 1.000000000000000000, 0.8660254037844387076, 1.000000000000000000, 0.8660254037844387076, 1.000000000000000000, 0.8660254037844387076, 1.000000000000000000, 0.8660254037844387076, 1.000000000000000000, 0.8660254037844387076, 1.000000000000000000, 0.8660254037844387076, 1.000000000000000000, 0.8660254037844387076, 1.000000000000000000, 0.8660254037844387076, 1.000000000000000000, 0.8660254037844387076, 1.000000000000000000, 0.8660254037844387076, 1.000000000000000000, 0.8660254037844387076, 1.000000000000000000, 0.8660254037844387076, 1.000000000000000000, 0.8660254037844387076, 1.000000000000000000, 0.8660254037844387076, 1.000000000000000000, 0.8660254037844387076, 1.000000000000000000, 0.8660254037844387076, 1.000000000000000000, 0.8660254037844387076, 1.000000000000000000, 0.8660254037844387076, 1.000000000000000000, 0.8660254037844387076, 1.000000000000000000, 0.8660254037844387076, 1.000000000000000000, 0.8660254037844387076, 1.000000000000000000, 0.8660254037844387076, 1.000000000000000000, 0.8660254037844387076, 1.000000000000000000, 0.8660254037844387076, 1.000000000000000000, 0.8660254037844387076, 1.000000000000000000, 0.8660254037844387076, 1.000000000000000000, 0.8660254037844387076, 1.000000000000000000, 0.8660254037844387076, 1.000000000000000000, 0.8660254037844387076, 1.000000000000000000, 0.8660254037844387076, 1.000000000000000000, 0.8660254037844387076, 1.000000000000000000, 0.8660254037844387076, 1.000000000000000000, 0.8660254037844387076, 1.000000000000000000, 0.8660254037844387076, 1.000000000000000000, 0.8660254037844387076, 1.000000000000000000, 0.8660254037844387076, 1.000000000000000000, 0.8660254037844387076, 1.000000000000000000, 0.8660254037844387076, 1.000000000000000000, 0.8660254037844387076, 1.000000000000000000, 0.8660254037844387076, 1.000000000000000000, 0.8660254037844387076, 1.000000000000000000, 0.8660254037844387076, 1.000000000000000000, 0.8660254037844387076, 1.000000000000000000, 0.8660254037844387076, 1.000000000000000000, 0.8660254037844387076, 1.000000000000000000, 0.8660254037844387076, 1.000000000000000000, 0.8660254037844387076, 1.000000000000000000, 0.8660254037844387076, 1.000000000000000000, 0.8660254037844387076, 1.000000000000000000, 0.8660254037844387076, 1.000000000000000000, 0.8660254037844387076, 1.000000000000000000, 0.8660254037844387076, 1.000000000000000000, 0.8660254037844387076, 1.000000000000000000, 0.8660254037844387076, 1.000000000000000000, 0.8660254037844387076, 1.000000000000000000, 0.8660254037844387076, 1.000000000000000000, 0.8660254037844387076, 1.000000000000000000, 0.8660254037844387076, 1.000000000000000000, 0.8660254037844387076, 1.000000000000000000, 0.8660254037844387076, 1.000000000000000000, 0.8660254037844387076, 1.000000000000000000, 0.8660254037844387076, 1.000000000000000000, 0.8660254037844387076, 1.000000000000000000, 0.8660254037844387076, 1.000000000000000000, 0.8660254037844387076, 1.000000000000000000, 0.8660254037844387076, 1.000000000000000000, 0.8660254037844387076, 1.000000000000000000, 0.8660254037844387076, 1.000000000000000000, 0.8660254037844387076, 1.000000000000000000, 0.8660254037844387076, 1.000000000000000000, 0.8660254037844387076, 1.000000000000000000, 0.8660254037844387076, 1.000000000000000000, 0.8660254037844387076, 1.000000000000000000, 0.8660254037844387076, 1.000000000000000000, 0.8660254037844387076, 1.000000000000000000, 0.8660254037844387076, 1.000000000000000000, 0.8660254037844387076, 1.000000000000000000, 0.8660254037844387076, 1.000000000000000000, 0.8660254037844387076, 1.000000000000000000, 0.8660254037844387076, 1.000000000000000000, 0.8660254037844387076, 1.000000000000000000, 0.8660254037844387076, 1.000000000000000000, 0.8660254037844387076, 1.000000000000000000, 0.8660254037844387076, 1.000000000000000000, 0.8660254037844387076, 1.000000000000000000, 0.8660254037844387076, 1.000000000000000000, 0.8660254037844387076, 1.000000000000000000, 0.8660254037844387076, 1.000000000000000000 ) ) 
 REPRESENTATION_ITEM ( '' )  );
#15411 = CARTESIAN_POINT ( 'NONE',  ( -3.999999999999999112, 18.48124999877096641, 27.69059892324149530 ) ) ;
#15412 = CARTESIAN_POINT ( 'NONE',  ( 8.184375000614515727, 4.541064518000418104, 2.621784821874999949 ) ) ;
#15413 = CARTESIAN_POINT ( 'NONE',  ( 26.95312500061451644, 4.541064518000418104, -2.621784821874998173 ) ) ;
#15414 = CARTESIAN_POINT ( 'NONE',  ( 5.662499999999998757, 2.886751345948193936, 4.999999999999883649 ) ) ;
#15415 = CARTESIAN_POINT ( 'NONE',  ( 27.50625000122903074, -4.330127018922190985, -2.500000000000001332 ) ) ;
#15416 = CARTESIAN_POINT ( 'NONE',  ( 4.509375000614518569, 4.541064518000418104, -2.621784821874998173 ) ) ;
#15417 = CARTESIAN_POINT ( 'NONE',  ( 8.446875000614518569, -3.027376345333610441, -5.243569643749999898 ) ) ;
#15418 = CARTESIAN_POINT ( 'NONE',  ( 29.37187500061451928, 3.027376345333611329, 5.243569643749999010 ) ) ;
#15419 = CARTESIAN_POINT ( 'NONE',  ( -4.243569643749999898, 12.11562500061459424, 27.54997392385601529 ) ) ;
#15420 = CARTESIAN_POINT ( 'NONE',  ( 22.42500000000000071, -4.330127018922194537, 2.499999999999995559 ) ) ;
#15421 = EDGE_CURVE ( 'NONE', #21571, #72350, #57281, .T. ) ;
#15422 = CARTESIAN_POINT ( 'NONE',  ( 4.387500000000002842, -2.886751345948129988, 4.999999999999997335 ) ) ;
#15423 = ORIENTED_EDGE ( 'NONE', *, *, #37449, .T. ) ;
#15424 = CARTESIAN_POINT ( 'NONE',  ( 18.06562500061451715, 3.027376345333611329, 5.243569643749999010 ) ) ;
#15425 = CARTESIAN_POINT ( 'NONE',  ( 10.60312500061451679, -4.541064518000417216, -2.621784821875001281 ) ) ;
#15426 = CARTESIAN_POINT ( 'NONE',  ( 21.75937500061451502, -5.492252693125287522, -1.008910452111647106E-15 ) ) ;
#15427 = CARTESIAN_POINT ( 'NONE',  ( 7.246875000614518392, 6.054752690667223547, 3.707466751127219781E-16 ) ) ;
#15428 = CARTESIAN_POINT ( 'NONE',  ( 22.64999999999999858, 4.330127018922192761, -2.499999999999997780 ) ) ;
#15429 = CARTESIAN_POINT ( 'NONE',  ( 19.57500000122903216, 2.886751345948129099, -4.999999999999998224 ) ) ;
#15430 = CARTESIAN_POINT ( 'NONE',  ( 10.20937500061451786, -4.541064518000417216, -2.621784821875001281 ) ) ;
#15431 = CARTESIAN_POINT ( 'NONE',  ( 13.09687500061451892, 6.054752690667223547, 3.707466751127219781E-16 ) ) ;
#15432 = CARTESIAN_POINT ( 'NONE',  ( 23.48437500061451644, 4.541064518000418104, 2.621784821874999949 ) ) ;
#15433 = CARTESIAN_POINT ( 'NONE',  ( 4.192336996406676342, -2.724758798235080715, 4.480034832487019614 ) ) ;
#15434 = ORIENTED_EDGE ( 'NONE', *, *, #35065, .F. ) ;
#15435 = CARTESIAN_POINT ( 'NONE',  ( 12.56250000000000178, -5.773502691896255534, -1.060575238724906372E-15 ) ) ;
#15436 = CARTESIAN_POINT ( 'NONE',  ( 18.00937500061451502, 4.541064518000418104, -2.621784821874998173 ) ) ;
#15437 = CARTESIAN_POINT ( 'NONE',  ( 8.259375000614518569, 0.000000000000000000, 5.243569643749999010 ) ) ;
#15438 = CARTESIAN_POINT ( 'NONE',  ( 2.655984681222220721E-16, 15.00312499938548427, 25.66244784525396483 ) ) ;
#15439 = CARTESIAN_POINT ( 'NONE',  ( 20.32499999999999929, 6.123233995736764310E-16, -4.999999999999998224 ) ) ;
#15440 = CARTESIAN_POINT ( 'NONE',  ( -4.000000000000000888, 15.01250000000000107, 32.30940107675850470 ) ) ;
#15441 = CARTESIAN_POINT ( 'NONE',  ( 1.626862140677534273E-15, 9.875000001229034652, -26.00000000000000355 ) ) ;
#15442 = CARTESIAN_POINT ( 'NONE',  ( 22.54687500061451999, 5.492252693125287522, 3.363034840372157021E-16 ) ) ;
#15443 = CARTESIAN_POINT ( 'NONE',  ( 13.60312500061451679, 0.000000000000000000, 5.243569643749999010 ) ) ;
#15444 = CARTESIAN_POINT ( 'NONE',  ( 28.24687500061451573, -3.027376345333610441, -5.243569643749999898 ) ) ;
#15445 = FILL_AREA_STYLE_COLOUR ( '', #54914 ) ;
#15446 = FACE_OUTER_BOUND ( 'NONE', #40806, .T. ) ;
#15447 = CARTESIAN_POINT ( 'NONE',  ( 12.59999999999999964, -4.330127018922190985, -2.500000000000001332 ) ) ;
#15448 = CARTESIAN_POINT ( 'NONE',  ( 8.484601909799253346E-16, 17.07500000122903572, 34.61880215351700230 ) ) ;
#15449 = CARTESIAN_POINT ( 'NONE',  ( 12.30000000122903181, -2.886751345948125991, -5.000000000000000000 ) ) ;
#15450 = CARTESIAN_POINT ( 'NONE',  ( 23.48437500061451644, 4.541064518000418104, 2.621784821874999949 ) ) ;
#15451 = CARTESIAN_POINT ( 'NONE',  ( 15.87187500061451573, 3.027376345333611329, 5.243569643749999010 ) ) ;
#15452 = CARTESIAN_POINT ( 'NONE',  ( -3.999999999999999112, 12.34999999999999964, 30.00000000000000000 ) ) ;
#15453 = ORIENTED_EDGE ( 'NONE', *, *, #48200, .F. ) ;
#15454 = CARTESIAN_POINT ( 'NONE',  ( 16.94062500061451715, -3.027376345333610441, -5.243569643749999898 ) ) ;
#15455 = CARTESIAN_POINT ( 'NONE',  ( 29.62500000122903288, 2.886751345948126879, 4.999999999999999112 ) ) ;
#15456 = CARTESIAN_POINT ( 'NONE',  ( 16.58437500061451786, 6.421520780324663323E-16, -5.243569643749999010 ) ) ;
#15457 = CARTESIAN_POINT ( 'NONE',  ( 5.128125000614516260, -4.541064518000419881, 2.621784821874995952 ) ) ;
#15458 = CARTESIAN_POINT ( 'NONE',  ( 19.04062500061451146, -3.027376345333614438, 5.243569643749998122 ) ) ;
#15459 = CARTESIAN_POINT ( 'NONE',  ( -2.000000000000000000, 16.77500000000000213, -33.46410161513775705 ) ) ;
#15460 = CARTESIAN_POINT ( 'NONE',  ( 29.74687500061451217, 6.054752690667223547, 3.707466751127219781E-16 ) ) ;
#15461 = CARTESIAN_POINT ( 'NONE',  ( -4.243569643749999898, 12.56562500061451715, 27.54997392385601529 ) ) ;
#15462 = CARTESIAN_POINT ( 'NONE',  ( 16.62187500061451573, 3.027376345333613106, -5.243569643749998122 ) ) ;
#15463 = CARTESIAN_POINT ( 'NONE',  ( 15.93750000122903110, 6.123233995736764310E-16, -4.999999999999998224 ) ) ;
#15464 = CARTESIAN_POINT ( 'NONE',  ( 10.77187500061451786, 2.746126346562645981, -4.756430356249997438 ) ) ;
#15465 = CARTESIAN_POINT ( 'NONE',  ( -4.243569643749999898, 19.37187500061451928, -32.45002607614398471 ) ) ;
#15466 = CARTESIAN_POINT ( 'NONE',  ( 20.29687500061451644, 6.054752690667223547, 3.707466751127219781E-16 ) ) ;
#15467 = CARTESIAN_POINT ( 'NONE',  ( 22.53750000122903430, -4.330127018922194537, 2.499999999999995559 ) ) ;
#15468 = EDGE_CURVE ( 'NONE', #3561, #45011, #23695, .T. ) ;
#15469 = CARTESIAN_POINT ( 'NONE',  ( 23.12812500061451360, -4.541064518000419881, 2.621784821874995952 ) ) ;
#15470 = CARTESIAN_POINT ( 'NONE',  ( 15.98437500061451821, -4.541064518000419881, 2.621784821874995952 ) ) ;
#15471 = CARTESIAN_POINT ( 'NONE',  ( 13.15312500061451750, 0.000000000000000000, 5.243569643749999010 ) ) ;
#15472 = CARTESIAN_POINT ( 'NONE',  ( -2.121784821874996840, 15.88437500061451857, 33.67503911421598417 ) ) ;
#15473 = CARTESIAN_POINT ( 'NONE',  ( 17.87812500061451715, 6.421520780324663323E-16, -5.243569643749999010 ) ) ;
#15474 = ORIENTED_EDGE ( 'NONE', *, *, #57411, .F. ) ;
#15475 = ORIENTED_EDGE ( 'NONE', *, *, #53989, .F. ) ;
#15476 = CARTESIAN_POINT ( 'NONE',  ( 22.61250000000000071, 2.886751345948129099, -4.999999999999998224 ) ) ;
#15477 = CARTESIAN_POINT ( 'NONE',  ( 2.121784821874999061, 19.25937500061451857, -33.67503911421598417 ) ) ;
#15478 = DIRECTION ( 'NONE',  ( 1.000000000000000000, 0.000000000000000000, 0.000000000000000000 ) ) ;
#15479 = CARTESIAN_POINT ( 'NONE',  ( 23.76562500061451644, 3.027376345333613106, -5.243569643749998122 ) ) ;
#15480 = AXIS2_PLACEMENT_3D ( 'NONE', #66874, #15508, #25882 ) ;
#15481 = CARTESIAN_POINT ( 'NONE',  ( 4.640625000614518214, -3.027376345333614438, 5.243569643749998122 ) ) ;
#15482 = CARTESIAN_POINT ( 'NONE',  ( 18.33750000122903501, 4.330127018922191873, 2.499999999999999556 ) ) ;
#15483 = CARTESIAN_POINT ( 'NONE',  ( 22.07812500061451644, 4.541064518000418104, 2.621784821874999949 ) ) ;
#15484 = CARTESIAN_POINT ( 'NONE',  ( 23.02499999999999858, 6.123233995736764310E-16, -4.999999999999998224 ) ) ;
#15485 = CARTESIAN_POINT ( 'NONE',  ( 24.47812500061451502, -4.541064518000419881, 2.621784821874995952 ) ) ;
#15486 = CARTESIAN_POINT ( 'NONE',  ( 8.165625000614516793, 3.027376345333611329, 5.243569643749999010 ) ) ;
#15487 = ORIENTED_EDGE ( 'NONE', *, *, #51411, .F. ) ;
#15488 = PRODUCT_DEFINITION_SHAPE ( 'NONE', 'NONE',  #3433 ) ;
#15489 = CARTESIAN_POINT ( 'NONE',  ( 22.75312500061451360, -4.541064518000417216, -2.621784821875001281 ) ) ;
#15490 = CARTESIAN_POINT ( 'NONE',  ( 3.065625000614517592, 3.027376345333613106, -5.243569643749998122 ) ) ;
#15491 = CARTESIAN_POINT ( 'NONE',  ( 12.42187500061451821, -5.492252693125287522, -1.008910452111647106E-15 ) ) ;
#15492 = CARTESIAN_POINT ( 'NONE',  ( 11.02500000122903501, 2.886751345948129099, -4.999999999999997335 ) ) ;
#15493 = CARTESIAN_POINT ( 'NONE',  ( -2.828200636599751609E-16, 12.80000000122903181, -34.61880215351700230 ) ) ;
#15494 = CARTESIAN_POINT ( 'NONE',  ( -5.810221930991193690E-16, 10.43750000000000000, -34.00000000000000000 ) ) ;
#15495 = CARTESIAN_POINT ( 'NONE',  ( 9.787499999999999645, -2.886751345948129988, 4.999999999999997335 ) ) ;
#15496 = CARTESIAN_POINT ( 'NONE',  ( 11.85937500061451644, 0.000000000000000000, 5.243569643749999010 ) ) ;
#15497 = CARTESIAN_POINT ( 'NONE',  ( 5.287500001229035185, 4.330127018922191873, 2.499999999999999556 ) ) ;
#15498 = CARTESIAN_POINT ( 'NONE',  ( 14.74687500061451573, -3.027376345333610441, -5.243569643749999898 ) ) ;
#15499 = CARTESIAN_POINT ( 'NONE',  ( 6.309375000614517504, 4.541064518000418104, -2.621784821874998173 ) ) ;
#15500 = CARTESIAN_POINT ( 'NONE',  ( 16.83749999999999858, 5.773502691896255534, 3.535250795749688401E-16 ) ) ;
#15501 = DIRECTION ( 'NONE',  ( 0.000000000000000000, 0.000000000000000000, -1.000000000000000000 ) ) ;
#15502 = CARTESIAN_POINT ( 'NONE',  ( 11.70937500061451608, 4.541064518000418104, -2.621784821874998173 ) ) ;
#15503 = DIRECTION ( 'NONE',  ( -1.000000000000000000, -0.000000000000000000, -0.000000000000000000 ) ) ;
#15504 = CARTESIAN_POINT ( 'NONE',  ( 21.59062500061451928, 6.054752690667223547, 3.707466751127219781E-16 ) ) ;
#15505 = LINE ( 'NONE', #16598, #43954 ) ;
#15506 = CARTESIAN_POINT ( 'NONE',  ( -3.000416591977282496E-16, 18.79062500061460028, 25.09994784771203058 ) ) ;
#15507 = CARTESIAN_POINT ( 'NONE',  ( 22.65937500061451715, 0.000000000000000000, 5.243569643749999010 ) ) ;
#15508 = DIRECTION ( 'NONE',  ( -1.000000000000000000, -0.000000000000000000, -0.000000000000000000 ) ) ;
#15509 = CARTESIAN_POINT ( 'NONE',  ( 28.65000000122903145, 5.773502691896255534, 3.535250795749688894E-16 ) ) ;
#15510 = CARTESIAN_POINT ( 'NONE',  ( 21.19687500061451502, 0.000000000000000000, 4.756430356249998326 ) ) ;
#15511 = CARTESIAN_POINT ( 'NONE',  ( 24.89062500061451644, -3.027376345333614438, 5.243569643749998122 ) ) ;
#15512 = CARTESIAN_POINT ( 'NONE',  ( 17.24062500061451786, -3.027376345333614438, 5.243569643749998122 ) ) ;
#15513 = CARTESIAN_POINT ( 'NONE',  ( 14.30625000122903145, 0.000000000000000000, 4.999999999999998224 ) ) ;
#15514 = CARTESIAN_POINT ( 'NONE',  ( 15.08437500061451786, -4.541064518000419881, 2.621784821874995952 ) ) ;
#15515 = DIRECTION ( 'NONE',  ( -0.000000000000000000, -1.000000000000000000, -0.000000000000000000 ) ) ;
#15516 = CARTESIAN_POINT ( 'NONE',  ( 27.63750000122903216, 6.123233995736764310E-16, -4.999999999999998224 ) ) ;
#15517 = CARTESIAN_POINT ( 'NONE',  ( 6.196875000614515905, -3.027376345333610441, -5.243569643749999898 ) ) ;
#15518 = CARTESIAN_POINT ( 'NONE',  ( 15.94687500061451502, -3.027376345333614438, 5.243569643749998122 ) ) ;
#15519 = CARTESIAN_POINT ( 'NONE',  ( 16.27499999999999858, 6.123233995736764310E-16, -4.999999999999998224 ) ) ;
#15520 = CARTESIAN_POINT ( 'NONE',  ( 23.09999999999999787, 4.330127018922192761, -2.499999999999997780 ) ) ;
#15521 = CARTESIAN_POINT ( 'NONE',  ( 3.787500001229033408, 6.123233995736764310E-16, -4.999999999999998224 ) ) ;
#15522 = CARTESIAN_POINT ( 'NONE',  ( 25.24687500061451573, 6.054752690667223547, 3.707466751127219781E-16 ) ) ;
#15523 = CARTESIAN_POINT ( 'NONE',  ( 15.45937500061451608, 0.000000000000000000, 5.243569643749999010 ) ) ;
#15524 = CARTESIAN_POINT ( 'NONE',  ( -7.967954043666661671E-16, 13.54062499938548214, 34.33755215474603517 ) ) ;
#15525 = CARTESIAN_POINT ( 'NONE',  ( 27.93750000000000000, -2.886751345948125991, -5.000000000000000000 ) ) ;
#15526 = CARTESIAN_POINT ( 'NONE',  ( 6.037500000000001421, 5.773502691896255534, 3.535250795749688894E-16 ) ) ;
#15527 = CARTESIAN_POINT ( 'NONE',  ( 8.596875000614515372, 0.000000000000000000, 4.756430356249998326 ) ) ;
#15528 = CARTESIAN_POINT ( 'NONE',  ( 20.84062500061451573, -3.027376345333614438, 5.243569643749998122 ) ) ;
#15529 = CARTESIAN_POINT ( 'NONE',  ( 8.887499999999999289, -2.886751345948129988, 4.999999999999997335 ) ) ;
#15530 = CARTESIAN_POINT ( 'NONE',  ( 3.703125000614516882, 0.000000000000000000, 5.243569643749999010 ) ) ;
#15531 = CARTESIAN_POINT ( 'NONE',  ( 18.33749999999999858, -2.886751345948129988, 4.999999999999997335 ) ) ;
#15532 = CARTESIAN_POINT ( 'NONE',  ( -1.071796769724485010, 17.39240381056766083, 34.00000000000000000 ) ) ;
#15533 = CARTESIAN_POINT ( 'NONE',  ( 24.15000000122903145, 5.773502691896255534, 3.535250795749688894E-16 ) ) ;
#15534 = CARTESIAN_POINT ( 'NONE',  ( 3.685019977366418509, 9.302529035819389946, 34.75091536352346111 ) ) ;
#15535 = CARTESIAN_POINT ( 'NONE',  ( 28.39687500061452141, 6.054752690667223547, 3.707466751127219781E-16 ) ) ;
#15536 = EDGE_LOOP ( 'NONE', ( #52738, #18696, #62734, #1739 ) ) ;
#15537 = CARTESIAN_POINT ( 'NONE',  ( 17.42812500061451786, 6.421520780324663323E-16, -5.243569643749999010 ) ) ;
#15538 = CARTESIAN_POINT ( 'NONE',  ( 24.70312500061451644, 4.541064518000418104, -2.621784821874998173 ) ) ;
#15539 = CARTESIAN_POINT ( 'NONE',  ( 24.34687500061451715, 6.054752690667223547, 3.707466751127219781E-16 ) ) ;
#15540 = CARTESIAN_POINT ( 'NONE',  ( 8.550000000000002487, -4.330127018922190985, -2.500000000000001332 ) ) ;
#15541 = CARTESIAN_POINT ( 'NONE',  ( 11.20312500061451644, 4.541064518000418104, -2.621784821874998173 ) ) ;
#15542 = CARTESIAN_POINT ( 'NONE',  ( 27.55312500061451786, 0.000000000000000000, 5.243569643749999010 ) ) ;
#15543 = CARTESIAN_POINT ( 'NONE',  ( 14.25937500061451679, -4.541064518000417216, -2.621784821875001281 ) ) ;
#15544 = CARTESIAN_POINT ( 'NONE',  ( 19.02187500061451786, 3.027376345333611329, 5.243569643749999010 ) ) ;
#15545 = CYLINDRICAL_SURFACE ( 'NONE', #49857, 3.999999999999996447 ) ;
#15546 = CARTESIAN_POINT ( 'NONE',  ( -4.243569643749997233, 18.94062500061451715, 32.45002607614398471 ) ) ;
#15547 = CARTESIAN_POINT ( 'NONE',  ( 22.65000000122903856, -2.886751345948125991, -5.000000000000000000 ) ) ;
#15548 = CARTESIAN_POINT ( 'NONE',  ( 17.89687500061451431, -2.746126346562641984, -4.756430356249999214 ) ) ;
#15549 = CARTESIAN_POINT ( 'NONE',  ( 15.06562500061451892, -6.054752690667223547, -1.112240025338166033E-15 ) ) ;
#15550 = CARTESIAN_POINT ( 'NONE',  ( 8.446875000614518569, -3.027376345333610441, -5.243569643749999898 ) ) ;
#15551 = CARTESIAN_POINT ( 'NONE',  ( 8.296875000614516438, -3.027376345333614438, 5.243569643749998122 ) ) ;
#15552 = ORIENTED_EDGE ( 'NONE', *, *, #65470, .T. ) ;
#15553 = CARTESIAN_POINT ( 'NONE',  ( 28.05937500061451573, 0.000000000000000000, 5.243569643749999010 ) ) ;
#15554 = CARTESIAN_POINT ( 'NONE',  ( 20.16562500061451146, 3.027376345333613106, -5.243569643749998122 ) ) ;
#15555 = CARTESIAN_POINT ( 'NONE',  ( 3.028125000614518392, 6.421520780324663323E-16, -5.243569643749999010 ) ) ;
#15556 = EDGE_CURVE ( 'NONE', #63037, #1518, #64831, .T. ) ;
#15557 = CARTESIAN_POINT ( 'NONE',  ( 3.571875000614517237, 3.027376345333613106, -5.243569643749998122 ) ) ;
#15558 = CARTESIAN_POINT ( 'NONE',  ( 24.72187500061451360, 3.027376345333613106, -5.243569643749998122 ) ) ;
#15559 = CARTESIAN_POINT ( 'NONE',  ( 19.34062500061451573, 6.054752690667223547, 3.707466751127219781E-16 ) ) ;
#15560 = CARTESIAN_POINT ( 'NONE',  ( -3.999999999999999112, 12.80000000000000071, 30.00000000000000000 ) ) ;
#15561 = CARTESIAN_POINT ( 'NONE',  ( 25.75312500061451715, 0.000000000000000000, 5.243569643749999010 ) ) ;
#15562 = CARTESIAN_POINT ( 'NONE',  ( 6.412500001229036073, -4.330127018922190985, -2.500000000000001332 ) ) ;
#15563 = VERTEX_POINT ( 'NONE', #41073 ) ;
#15564 = CARTESIAN_POINT ( 'NONE',  ( 3.037500001229032964, 4.330127018922191873, 2.499999999999999556 ) ) ;
#15565 = CARTESIAN_POINT ( 'NONE',  ( -3.999999999999999556, 14.56250000000000000, -32.30940107675850470 ) ) ;
#15566 = CARTESIAN_POINT ( 'NONE',  ( 22.01250000122903216, 0.000000000000000000, 4.999999999999998224 ) ) ;
#15567 = CARTESIAN_POINT ( 'NONE',  ( 3.756430356250000102, 14.55312499938548321, 30.00000000000000000 ) ) ;
#15568 =( GEOMETRIC_REPRESENTATION_CONTEXT ( 3 ) GLOBAL_UNCERTAINTY_ASSIGNED_CONTEXT ( ( #18835 ) ) GLOBAL_UNIT_ASSIGNED_CONTEXT ( ( #51409, #7067, #812 ) ) REPRESENTATION_CONTEXT ( 'NONE', 'WORKASPACE' ) );
#15569 = CARTESIAN_POINT ( 'NONE',  ( 4.809375000614516615, -4.541064518000417216, -2.621784821875001281 ) ) ;
#15570 = CARTESIAN_POINT ( 'NONE',  ( 29.12812500061451715, 6.421520780324663323E-16, -5.243569643749999010 ) ) ;
#15571 = CARTESIAN_POINT ( 'NONE',  ( 12.10312500061451857, 4.541064518000418104, -2.621784821874998173 ) ) ;
#15572 = CARTESIAN_POINT ( 'NONE',  ( 5.821875000614519458, 3.027376345333613106, -5.243569643749998122 ) ) ;
#15573 = CARTESIAN_POINT ( 'NONE',  ( 23.47500000122903430, -5.773502691896255534, -1.060575238724906372E-15 ) ) ;
#15574 = CARTESIAN_POINT ( 'NONE',  ( 15.83437500061451608, 4.541064518000418104, 2.621784821874999949 ) ) ;
#15575 = CARTESIAN_POINT ( 'NONE',  ( 28.49062500061451431, -3.027376345333614438, 5.243569643749998122 ) ) ;
#15576 = CARTESIAN_POINT ( 'NONE',  ( 29.28749999999999787, -2.886751345948125991, -5.000000000000000000 ) ) ;
#15577 = CARTESIAN_POINT ( 'NONE',  ( 4.228125000614517681, -4.541064518000419881, 2.621784821874995952 ) ) ;
#15578 = CARTESIAN_POINT ( 'NONE',  ( 16.19062500061451715, 6.054752690667223547, 3.707466751127219781E-16 ) ) ;
#15579 = ORIENTED_EDGE ( 'NONE', *, *, #6144, .F. ) ;
#15580 = CARTESIAN_POINT ( 'NONE',  ( 10.67812500061451608, 6.421520780324663323E-16, -5.243569643749999010 ) ) ;
#15581 = CARTESIAN_POINT ( 'NONE',  ( 7.678125000614516082, 4.541064518000418104, 2.621784821874999949 ) ) ;
#15582 = CARTESIAN_POINT ( 'NONE',  ( 18.53437500061451715, 4.119189519843966529, 2.378215178124999607 ) ) ;
#15583 = CARTESIAN_POINT ( 'NONE',  ( 8.362500000000002487, 2.886751345948126879, 4.999999999999999112 ) ) ;
#15584 = CARTESIAN_POINT ( 'NONE',  ( 4.350000001229033408, 5.773502691896255534, 3.535250795749688894E-16 ) ) ;
#15585 = CARTESIAN_POINT ( 'NONE',  ( 18.14999999999999858, 4.330127018922192761, -2.499999999999997780 ) ) ;
#15586 = CARTESIAN_POINT ( 'NONE',  ( 19.65937500061451360, -4.541064518000417216, -2.621784821875001281 ) ) ;
#15587 = CARTESIAN_POINT ( 'NONE',  ( 13.91250000122903252, 0.000000000000000000, 4.999999999999998224 ) ) ;
#15588 = CARTESIAN_POINT ( 'NONE',  ( 21.78750000000000142, 5.773502691896255534, 3.535250795749688894E-16 ) ) ;
#15589 = CARTESIAN_POINT ( 'NONE',  ( -2.121784821874996840, 17.17812500061451786, -26.32496088578401583 ) ) ;
#15590 = CARTESIAN_POINT ( 'NONE',  ( -3.999999999999999112, 13.53124999877096535, 27.69059892324149530 ) ) ;
#15591 = DIRECTION ( 'NONE',  ( -1.000000000000000000, -0.000000000000000000, -0.000000000000000000 ) ) ;
#15592 = LINE ( 'NONE', #3442, #58360 ) ;
#15593 = CARTESIAN_POINT ( 'NONE',  ( 20.13750000122903216, 4.330127018922191873, 2.499999999999999556 ) ) ;
#15594 = CARTESIAN_POINT ( 'NONE',  ( 13.73437500061451821, -4.541064518000419881, 2.621784821874995952 ) ) ;
#15595 = CARTESIAN_POINT ( 'NONE',  ( 26.55000000000000071, -4.330127018922190985, -2.500000000000001332 ) ) ;
#15596 = EDGE_CURVE ( 'NONE', #32725, #34653, #2065, .T. ) ;
#15597 = CARTESIAN_POINT ( 'NONE',  ( 12.29062500061451857, -3.027376345333614438, 5.243569643749998122 ) ) ;
#15598 = CARTESIAN_POINT ( 'NONE',  ( 26.97187500061451360, 4.119189519843966529, 2.378215178124999607 ) ) ;
#15599 = CARTESIAN_POINT ( 'NONE',  ( 21.98437500061451644, 6.421520780324663323E-16, -5.243569643749999010 ) ) ;
#15600 = CARTESIAN_POINT ( 'NONE',  ( 13.43437500061451750, 5.492252693125287522, 3.363034840372157021E-16 ) ) ;
#15601 = EDGE_CURVE ( 'NONE', #60669, #32563, #14770, .T. ) ;
#15602 = CARTESIAN_POINT ( 'NONE',  ( 8.203125000614518214, 0.000000000000000000, 5.243569643749999010 ) ) ;
#15603 = CARTESIAN_POINT ( 'NONE',  ( 13.58437500061451786, 4.541064518000418104, 2.621784821874999949 ) ) ;
#15604 = ORIENTED_EDGE ( 'NONE', *, *, #65676, .F. ) ;
#15605 = CARTESIAN_POINT ( 'NONE',  ( 22.84687500061451715, -3.027376345333610441, -5.243569643749999898 ) ) ;
#15606 = DIRECTION ( 'NONE',  ( -1.000000000000000000, -0.000000000000000000, -0.000000000000000000 ) ) ;
#15607 =( BOUNDED_CURVE ( )  B_SPLINE_CURVE ( 2, ( #15251, #65499, #49254, #20791, #3460, #43710, #4555, #49616, #14156 ),
 .UNSPECIFIED., .F., .F. ) 
 B_SPLINE_CURVE_WITH_KNOTS ( ( 3, 2, 2, 2, 3 ),
 ( 0.8472222222222222099, 0.8518518518518518601, 0.8611111111111111605, 0.8703703703703703498, 0.8750000000000000000 ),
 .UNSPECIFIED. ) 
 CURVE ( )  GEOMETRIC_REPRESENTATION_ITEM ( )  RATIONAL_B_SPLINE_CURVE ( ( 0.9330127018922194093, 0.9330127018922194093, 1.000000000000000000, 0.8660254037844387076, 1.000000000000000000, 0.8660254037844387076, 1.000000000000000000, 0.9330127018922194093, 0.9330127018922194093 ) ) 
 REPRESENTATION_ITEM ( '' )  );
#15608 = CARTESIAN_POINT ( 'NONE',  ( 4.575000000000002842, 6.123233995736764310E-16, -4.999999999999998224 ) ) ;
#15609 = CARTESIAN_POINT ( 'NONE',  ( 18.11250000122903359, -4.330127018922190985, -2.500000000000001332 ) ) ;
#15610 = CARTESIAN_POINT ( 'NONE',  ( -3.999999999999999112, 17.86250000122903359, -30.00000000000000000 ) ) ;
#15611 = CARTESIAN_POINT ( 'NONE',  ( 14.51250000122903394, -4.330127018922190985, -2.500000000000001332 ) ) ;
#15612 = ORIENTED_EDGE ( 'NONE', *, *, #22319, .F. ) ;
#15613 = CARTESIAN_POINT ( 'NONE',  ( 14.47499999999999964, 6.123233995736764310E-16, -4.999999999999998224 ) ) ;
#15614 = CARTESIAN_POINT ( 'NONE',  ( 17.55000000000000071, -4.330127018922190985, -2.500000000000001332 ) ) ;
#15615 = CARTESIAN_POINT ( 'NONE',  ( 14.13750000122903394, 6.123233995736764310E-16, -4.999999999999998224 ) ) ;
#15616 = CARTESIAN_POINT ( 'NONE',  ( 10.97812500061451679, -4.541064518000419881, 2.621784821874995952 ) ) ;
#15617 = ORIENTED_EDGE ( 'NONE', *, *, #69599, .F. ) ;
#15618 = CARTESIAN_POINT ( 'NONE',  ( 9.528763966825557376E-15, 17.07500000122903572, -26.00000000000000000 ) ) ;
#15619 = CARTESIAN_POINT ( 'NONE',  ( -4.243569643749997233, 17.19687500061451502, -27.54997392385601174 ) ) ;
#15620 = CARTESIAN_POINT ( 'NONE',  ( 4.003125000614518925, 4.541064518000418104, -2.621784821874998173 ) ) ;
#15621 = CARTESIAN_POINT ( 'NONE',  ( 2.655984681222220721E-16, 15.00312499938548605, 25.66244784525396483 ) ) ;
#15622 = CARTESIAN_POINT ( 'NONE',  ( 11.02500000000000036, 4.330127018922191873, 2.499999999999999556 ) ) ;
#15623 = DIRECTION ( 'NONE',  ( -0.000000000000000000, -1.000000000000000000, -0.000000000000000000 ) ) ;
#15624 = VERTEX_POINT ( 'NONE', #18139 ) ;
#15625 = CARTESIAN_POINT ( 'NONE',  ( 23.24062500061451786, -3.027376345333610441, -5.243569643749999898 ) ) ;
#15626 = CARTESIAN_POINT ( 'NONE',  ( 3.631995133754550853, 3.436488000706471535, 3.917251957431123088 ) ) ;
#15627 = CARTESIAN_POINT ( 'NONE',  ( -1.878215178125001827, 19.69062499938548072, 33.25316411605952283 ) ) ;
#15628 = CARTESIAN_POINT ( 'NONE',  ( 21.27187500061451786, 3.027376345333611329, 5.243569643749999010 ) ) ;
#15629 = EDGE_CURVE ( 'NONE', #8998, #45106, #27518, .T. ) ;
#15630 = CARTESIAN_POINT ( 'NONE',  ( 18.92812500061451431, 4.541064518000418104, 2.621784821874999949 ) ) ;
#15631 = CARTESIAN_POINT ( 'NONE',  ( -2.121784821874996840, 13.57812500061459460, -26.32496088578401583 ) ) ;
#15632 = CARTESIAN_POINT ( 'NONE',  ( 24.48750000122903359, 6.123233995736764310E-16, -4.999999999999998224 ) ) ;
#15633 = CARTESIAN_POINT ( 'NONE',  ( 3.778125000614519280, -4.541064518000419881, 2.621784821874995952 ) ) ;
#15634 = CARTESIAN_POINT ( 'NONE',  ( 24.04687500061451644, -2.746126346562646425, 4.756430356249996549 ) ) ;
#15635 = CARTESIAN_POINT ( 'NONE',  ( 22.60312500061451857, 0.000000000000000000, 5.243569643749999010 ) ) ;
#15636 = CARTESIAN_POINT ( 'NONE',  ( 8.184375000614515727, 4.119189519843966529, 2.378215178124999607 ) ) ;
#15637 = CARTESIAN_POINT ( 'NONE',  ( -1.878215178125001827, 18.34062499938548285, 33.25316411605952283 ) ) ;
#15638 = CARTESIAN_POINT ( 'NONE',  ( 14.63437500061451679, -4.541064518000419881, 2.621784821874995952 ) ) ;
#15639 = CARTESIAN_POINT ( 'NONE',  ( 15.19687500061451857, -3.027376345333610441, -5.243569643749999898 ) ) ;
#15640 = CARTESIAN_POINT ( 'NONE',  ( 23.33437500061451786, 6.421520780324663323E-16, -5.243569643749999010 ) ) ;
#15641 = ORIENTED_EDGE ( 'NONE', *, *, #19119, .F. ) ;
#15642 = CARTESIAN_POINT ( 'NONE',  ( -2.121784821874996840, 11.38437500061451679, 33.67503911421598417 ) ) ;
#15643 = DIRECTION ( 'NONE',  ( -1.000000000000000000, -0.000000000000000000, -0.000000000000000000 ) ) ;
#15644 = CARTESIAN_POINT ( 'NONE',  ( 26.99062500061451431, 6.054752690667223547, 3.707466751127219781E-16 ) ) ;
#15645 =( BOUNDED_CURVE ( )  B_SPLINE_CURVE ( 2, ( #28361, #50897, #297, #22806, #45358, #63779, #23896 ),
 .UNSPECIFIED., .F., .F. ) 
 B_SPLINE_CURVE_WITH_KNOTS ( ( 3, 2, 2, 3 ),
 ( 0.5200000000000000178, 0.5233333333333333171, 0.5266666666666666163, 0.5300000000000000266 ),
 .UNSPECIFIED. ) 
 CURVE ( )  GEOMETRIC_REPRESENTATION_ITEM ( )  RATIONAL_B_SPLINE_CURVE ( ( 1.000000000000000000, 0.8660254037844387076, 1.000000000000000000, 0.8660254037844387076, 1.000000000000000000, 0.8660254037844387076, 1.000000000000000000 ) ) 
 REPRESENTATION_ITEM ( '' )  );
#15646 = CARTESIAN_POINT ( 'NONE',  ( 27.59062500061451573, -3.027376345333614438, 5.243569643749998122 ) ) ;
#15647 = CARTESIAN_POINT ( 'NONE',  ( 23.30625000122903145, 0.000000000000000000, 4.999999999999998224 ) ) ;
#15648 = CARTESIAN_POINT ( 'NONE',  ( -2.828200636599751609E-16, 19.88749999999999929, 25.38119784648299770 ) ) ;
#15649 = CARTESIAN_POINT ( 'NONE',  ( 6.609375000614519102, -4.541064518000417216, -2.621784821875001281 ) ) ;
#15650 = PRODUCT_CONTEXT ( 'NONE', #46934, 'mechanical' ) ;
#15651 = CARTESIAN_POINT ( 'NONE',  ( 13.35000000122903430, 5.773502691896255534, 3.535250795749688894E-16 ) ) ;
#15652 = CARTESIAN_POINT ( 'NONE',  ( 9.750000001229032875, 5.773502691896255534, 3.535250795749688894E-16 ) ) ;
#15653 = CARTESIAN_POINT ( 'NONE',  ( 29.47500000122903430, 2.886751345948129099, -4.999999999999998224 ) ) ;
#15654 = CARTESIAN_POINT ( 'NONE',  ( 4.000000000000000000, 16.04374999877096641, 30.00000000000000000 ) ) ;
#15655 = CARTESIAN_POINT ( 'NONE',  ( 19.40625000122902932, -4.330127018922190985, -2.500000000000001332 ) ) ;
#15656 = CARTESIAN_POINT ( 'NONE',  ( 12.38437500061451857, -4.541064518000419881, 2.621784821874995952 ) ) ;
#15657 = CARTESIAN_POINT ( 'NONE',  ( 2.000000000000001332, 17.56250000122903288, 33.46410161513774995 ) ) ;
#15658 = EDGE_LOOP ( 'NONE', ( #39621, #31530, #30148, #694 ) ) ;
#15659 = CARTESIAN_POINT ( 'NONE',  ( 19.34062500061451573, 6.054752690667223547, 3.707466751127219781E-16 ) ) ;
#15660 = CARTESIAN_POINT ( 'NONE',  ( 14.89687500061451786, 6.054752690667223547, 3.707466751127219781E-16 ) ) ;
#15661 = CARTESIAN_POINT ( 'NONE',  ( 6.028125000614517504, -4.541064518000419881, 2.621784821874995952 ) ) ;
#15662 = CARTESIAN_POINT ( 'NONE',  ( 20.97187500061451715, -6.054752690667223547, -1.112240025338166033E-15 ) ) ;
#15663 = CARTESIAN_POINT ( 'NONE',  ( 5.390625000614518214, 6.054752690667223547, 3.707466751127219781E-16 ) ) ;
#15664 = CYLINDRICAL_SURFACE ( 'NONE', #34433, 4.999999999999998224 ) ;
#15665 = CARTESIAN_POINT ( 'NONE',  ( 8.475000001229034297, 2.886751345948126879, 4.999999999999999112 ) ) ;
#15666 = EDGE_CURVE ( 'NONE', #30697, #34725, #16714, .T. ) ;
#15667 = CARTESIAN_POINT ( 'NONE',  ( 22.11562500061451786, 3.027376345333611329, 5.243569643749999010 ) ) ;
#15668 = CARTESIAN_POINT ( 'NONE',  ( -3.999999999999999556, 18.72500000122903074, -32.30940107675850470 ) ) ;
#15669 = CARTESIAN_POINT ( 'NONE',  ( 6.825000001229034829, -5.773502691896255534, -1.060575238724906372E-15 ) ) ;
#15670 =( BOUNDED_CURVE ( )  B_SPLINE_CURVE ( 2, ( #11318, #11677, #22028, #22747, #33839, #34193, #6129 ),
 .UNSPECIFIED., .F., .F. ) 
 B_SPLINE_CURVE_WITH_KNOTS ( ( 3, 2, 2, 3 ),
 ( 0.7583333333333333037, 0.7611111111111110716, 0.7638888888888889506, 0.7666666666666668295 ),
 .UNSPECIFIED. ) 
 CURVE ( )  GEOMETRIC_REPRESENTATION_ITEM ( )  RATIONAL_B_SPLINE_CURVE ( ( 1.000000000000000000, 0.8660254037844387076, 1.000000000000000000, 0.8660254037844387076, 1.000000000000000000, 0.8660254037844333785, 1.000000000000005329 ) ) 
 REPRESENTATION_ITEM ( '' )  );
#15671 = CARTESIAN_POINT ( 'NONE',  ( 18.51562500061451289, 3.027376345333611329, 5.243569643749999010 ) ) ;
#15672 = CARTESIAN_POINT ( 'NONE',  ( 14.61562500061451608, -6.054752690667223547, -1.112240025338166033E-15 ) ) ;
#15673 = CARTESIAN_POINT ( 'NONE',  ( 28.65937500061451715, -4.119189519843965641, -2.378215178125001383 ) ) ;
#15674 = CARTESIAN_POINT ( 'NONE',  ( 16.76249999999999929, 2.886751345948129099, -4.999999999999998224 ) ) ;
#15675 = CARTESIAN_POINT ( 'NONE',  ( 11.21250000122903501, 0.000000000000000000, 4.999999999999998224 ) ) ;
#15676 = CARTESIAN_POINT ( 'NONE',  ( 7.228125000614517681, 4.541064518000418104, 2.621784821874999949 ) ) ;
#15677 = CARTESIAN_POINT ( 'NONE',  ( 11.50312500061451892, -4.541064518000417216, -2.621784821875001281 ) ) ;
#15678 = CARTESIAN_POINT ( 'NONE',  ( 21.56250000122903288, 0.000000000000000000, 4.999999999999998224 ) ) ;
#15679 = CARTESIAN_POINT ( 'NONE',  ( 2.121784821875001281, 14.60937500061451821, -26.32496088578401938 ) ) ;
#15680 = CARTESIAN_POINT ( 'NONE',  ( 20.22187500061451715, 3.027376345333613106, -5.243569643749998122 ) ) ;
#15681 = CARTESIAN_POINT ( 'NONE',  ( 5.810221930991193690E-16, 14.35624999877096464, 26.00000000000000000 ) ) ;
#15682 = CARTESIAN_POINT ( 'NONE',  ( 5.287500001229035185, 4.330127018922191873, 2.499999999999999556 ) ) ;
#15683 = CARTESIAN_POINT ( 'NONE',  ( 3.721875000614518036, 3.027376345333611329, 5.243569643749999010 ) ) ;
#15684 = CARTESIAN_POINT ( 'NONE',  ( 19.88437500061451857, 4.541064518000418104, 2.621784821874999949 ) ) ;
#15685 = CARTESIAN_POINT ( 'NONE',  ( 14.02499999999999858, 6.123233995736764310E-16, -4.999999999999998224 ) ) ;
#15686 = CARTESIAN_POINT ( 'NONE',  ( 19.15312500061451573, -4.541064518000417216, -2.621784821875001281 ) ) ;
#15687 = CARTESIAN_POINT ( 'NONE',  ( 12.91875000122903394, 2.886751345948126879, 4.999999999999999112 ) ) ;
#15688 = CARTESIAN_POINT ( 'NONE',  ( 10.95000000000000107, 4.330127018922192761, -2.499999999999997780 ) ) ;
#15689 = DIRECTION ( 'NONE',  ( 0.000000000000000000, 0.000000000000000000, -1.000000000000000000 ) ) ;
#15690 = CARTESIAN_POINT ( 'NONE',  ( 28.20937500061451786, -4.541064518000417216, -2.621784821875001281 ) ) ;
#15691 = CARTESIAN_POINT ( 'NONE',  ( 20.10937500061451289, 2.746126346562645981, -4.756430356249997438 ) ) ;
#15692 = CARTESIAN_POINT ( 'NONE',  ( 14.72812500061451679, 6.421520780324663323E-16, -5.243569643749999010 ) ) ;
#15693 = CARTESIAN_POINT ( 'NONE',  ( 14.03437500061451715, 4.541064518000418104, 2.621784821874999949 ) ) ;
#15694 = EDGE_LOOP ( 'NONE', ( #53929, #7935, #15854, #16422 ) ) ;
#15695 = CARTESIAN_POINT ( 'NONE',  ( 22.27500000122903145, 2.886751345948095793, -5.000000000000055067 ) ) ;
#15696 = CARTESIAN_POINT ( 'NONE',  ( 23.31562500061451715, 3.027376345333613106, -5.243569643749998122 ) ) ;
#15697 = CARTESIAN_POINT ( 'NONE',  ( 3.999999999999998668, 17.11250000000000071, 27.69059892324149530 ) ) ;
#15698 = CARTESIAN_POINT ( 'NONE',  ( 14.55000000000000071, 4.330127018922192761, -2.499999999999997780 ) ) ;
#15699 = CARTESIAN_POINT ( 'NONE',  ( 13.12500000000000178, 6.123233995736764310E-16, -4.999999999999998224 ) ) ;
#15700 = CARTESIAN_POINT ( 'NONE',  ( 24.41250000122903430, -4.330127018922190985, -2.500000000000001332 ) ) ;
#15701 = CARTESIAN_POINT ( 'NONE',  ( 17.69062500061451715, -3.027376345333614438, 5.243569643749998122 ) ) ;
#15702 = EDGE_LOOP ( 'NONE', ( #21492, #69876, #2088, #60520 ) ) ;
#15703 = CARTESIAN_POINT ( 'NONE',  ( 21.30000000000000071, 4.330127018922192761, -2.499999999999997780 ) ) ;
#15704 = EDGE_CURVE ( 'NONE', #6439, #18523, #71327, .T. ) ;
#15705 = CARTESIAN_POINT ( 'NONE',  ( 22.73437500061451644, -4.541064518000419881, 2.621784821874995952 ) ) ;
#15706 = ORIENTED_EDGE ( 'NONE', *, *, #3447, .T. ) ;
#15707 = DIRECTION ( 'NONE',  ( 0.000000000000000000, 0.000000000000000000, 1.000000000000000000 ) ) ;
#15708 = CARTESIAN_POINT ( 'NONE',  ( 9.853125000614516793, 4.541064518000418104, -2.621784821874998173 ) ) ;
#15709 = DIRECTION ( 'NONE',  ( 1.000000000000000000, 0.000000000000000000, 0.000000000000000000 ) ) ;
#15710 = CARTESIAN_POINT ( 'NONE',  ( 13.20937500061451431, -5.492252693125287522, -1.008910452111647106E-15 ) ) ;
#15711 = CARTESIAN_POINT ( 'NONE',  ( 16.91250000000000142, 2.886751345948126879, 4.999999999999999112 ) ) ;
#15712 = CARTESIAN_POINT ( 'NONE',  ( 24.89999999999999858, 4.330127018922192761, -2.499999999999997780 ) ) ;
#15713 = CARTESIAN_POINT ( 'NONE',  ( -2.121784821874999949, 19.27812500061451573, 26.32496088578401938 ) ) ;
#15714 = CARTESIAN_POINT ( 'NONE',  ( 4.996875000614516615, 6.054752690667223547, 3.707466751127219781E-16 ) ) ;
#15715 = CARTESIAN_POINT ( 'NONE',  ( 16.35937500061451644, 0.000000000000000000, 5.243569643749999010 ) ) ;
#15716 = CARTESIAN_POINT ( 'NONE',  ( 27.72187500061451715, -6.054752690667223547, -1.112240025338166033E-15 ) ) ;
#15717 = ORIENTED_EDGE ( 'NONE', *, *, #19271, .T. ) ;
#15718 = CARTESIAN_POINT ( 'NONE',  ( 25.94062500061451715, -3.027376345333610441, -5.243569643749999898 ) ) ;
#15719 = CARTESIAN_POINT ( 'NONE',  ( 27.90937500061451715, 4.541064518000418104, -2.621784821874998173 ) ) ;
#15720 = CYLINDRICAL_SURFACE ( 'NONE', #54587, 3.999999999999996447 ) ;
#15721 = CARTESIAN_POINT ( 'NONE',  ( 13.35000000000000142, 0.000000000000000000, 4.999999999999998224 ) ) ;
#15722 = CARTESIAN_POINT ( 'NONE',  ( 11.09062500061451573, -3.027376345333610441, -5.243569643749999898 ) ) ;
#15723 = CARTESIAN_POINT ( 'NONE',  ( 1.071796769724491227, 17.48615380933863506, 26.00000000000000000 ) ) ;
#15724 = CARTESIAN_POINT ( 'NONE',  ( 7.237499999999998934, -2.886751345948193048, -4.999999999999883649 ) ) ;
#15725 = CARTESIAN_POINT ( 'NONE',  ( 28.37812500061451715, 4.541064518000418104, 2.621784821874999949 ) ) ;
#15726 = CARTESIAN_POINT ( 'NONE',  ( 15.78750000122903430, -4.330127018922194537, 2.499999999999995559 ) ) ;
#15727 = CARTESIAN_POINT ( 'NONE',  ( 3.176339285701963888, -3.861459405730729433, 3.176339285701963888 ) ) ;
#15728 = CARTESIAN_POINT ( 'NONE',  ( 14.10937500061451644, 0.000000000000000000, 4.756430356249998326 ) ) ;
#15729 = CARTESIAN_POINT ( 'NONE',  ( 4.490625000614516971, 6.054752690667223547, 3.707466751127219781E-16 ) ) ;
#15730 = CARTESIAN_POINT ( 'NONE',  ( 21.90937500061451715, -4.541064518000417216, -2.621784821875001281 ) ) ;
#15731 = CARTESIAN_POINT ( 'NONE',  ( -3.000416591977282496E-16, 17.04687500061451644, 25.09994784771203058 ) ) ;
#15732 = CARTESIAN_POINT ( 'NONE',  ( 21.19687500061451502, 6.054752690667223547, 3.707466751127219781E-16 ) ) ;
#15733 = CARTESIAN_POINT ( 'NONE',  ( 28.58437500061451786, -4.541064518000419881, 2.621784821874995952 ) ) ;
#15734 = CARTESIAN_POINT ( 'NONE',  ( 4.243569643749999898, 18.24687500061451928, 32.45002607614398471 ) ) ;
#15735 = CARTESIAN_POINT ( 'NONE',  ( 11.31562500061451892, 3.027376345333611329, 5.243569643749999010 ) ) ;
#15736 = CARTESIAN_POINT ( 'NONE',  ( -3.999999999999999112, 15.16250000122903252, 30.00000000000000000 ) ) ;
#15737 = CARTESIAN_POINT ( 'NONE',  ( 6.759375000614516793, 4.541064518000418104, -2.621784821874998173 ) ) ;
#15738 = CARTESIAN_POINT ( 'NONE',  ( 3.999999999999999112, 15.72500000000000320, -30.00000000000000000 ) ) ;
#15739 = CARTESIAN_POINT ( 'NONE',  ( 8.878125000614515372, 6.421520780324663323E-16, -5.243569643749999010 ) ) ;
#15740 = CARTESIAN_POINT ( 'NONE',  ( 13.32187500061451502, -6.054752690667223547, -1.112240025338166033E-15 ) ) ;
#15741 = CARTESIAN_POINT ( 'NONE',  ( -3.999999999999999112, 18.98749999999999716, 27.69059892324149530 ) ) ;
#15742 = CARTESIAN_POINT ( 'NONE',  ( 21.75000000122903288, -2.886751345948125991, -5.000000000000000000 ) ) ;
#15743 = CARTESIAN_POINT ( 'NONE',  ( 8.146875000614516082, 6.054752690667223547, 3.707466751127219781E-16 ) ) ;
#15744 = CARTESIAN_POINT ( 'NONE',  ( 10.97812500061451679, -4.541064518000419881, 2.621784821874995952 ) ) ;
#15745 = CARTESIAN_POINT ( 'NONE',  ( 26.00625000122903074, 0.000000000000000000, 4.999999999999998224 ) ) ;
#15746 = CARTESIAN_POINT ( 'NONE',  ( 22.35937500061451644, -4.541064518000417216, -2.621784821875001281 ) ) ;
#15747 = DIRECTION ( 'NONE',  ( -1.000000000000000000, -0.000000000000000000, -0.000000000000000000 ) ) ;
#15748 = EDGE_CURVE ( 'NONE', #23263, #39486, #22327, .T. ) ;
#15749 = CARTESIAN_POINT ( 'NONE',  ( -1.092898315830470590, 4.886665047895962566, 33.85754803517728817 ) ) ;
#15750 = CARTESIAN_POINT ( 'NONE',  ( 29.59687500061451715, -3.027376345333610441, -5.243569643749999898 ) ) ;
#15751 = CARTESIAN_POINT ( 'NONE',  ( -2.121784821874996840, 11.38437500061451679, -26.32496088578401583 ) ) ;
#15752 = CARTESIAN_POINT ( 'NONE',  ( 16.27500000122903501, -5.773502691896255534, -1.060575238724906372E-15 ) ) ;
#15753 = CARTESIAN_POINT ( 'NONE',  ( -2.121784821874996840, 14.47812500061451679, -26.32496088578401583 ) ) ;
#15754 = CARTESIAN_POINT ( 'NONE',  ( 18.60000000122903430, -2.886751345948125991, -5.000000000000000000 ) ) ;
#15755 = CARTESIAN_POINT ( 'NONE',  ( 11.05312500061451608, -4.541064518000417216, -2.621784821875001281 ) ) ;
#15756 = ORIENTED_EDGE ( 'NONE', *, *, #42670, .T. ) ;
#15757 = CARTESIAN_POINT ( 'NONE',  ( 13.46249999999999858, -5.773502691896255534, -1.060575238724906372E-15 ) ) ;
#15758 = CARTESIAN_POINT ( 'NONE',  ( 1.626862140677534273E-15, 13.81250000000000000, 34.00000000000000000 ) ) ;
#15759 = CARTESIAN_POINT ( 'NONE',  ( 22.19062500061451715, -3.027376345333614438, 5.243569643749998122 ) ) ;
#15760 = CARTESIAN_POINT ( 'NONE',  ( 10.17187500061451999, -6.054752690667223547, -1.112240025338166033E-15 ) ) ;
#15761 = CARTESIAN_POINT ( 'NONE',  ( -5.810221930991193690E-16, 14.15000000122903145, 26.00000000000000355 ) ) ;
#15762 = EDGE_CURVE ( 'NONE', #2558, #64110, #39401, .T. ) ;
#15763 = CARTESIAN_POINT ( 'NONE',  ( 11.21250000122903501, 0.000000000000000000, 4.999999999999998224 ) ) ;
#15764 = CARTESIAN_POINT ( 'NONE',  ( 17.66250000122903430, -4.330127018922190985, -2.500000000000001332 ) ) ;
#15765 = CARTESIAN_POINT ( 'NONE',  ( 15.36562500061451608, 3.027376345333611329, 5.243569643749999010 ) ) ;
#15766 = CARTESIAN_POINT ( 'NONE',  ( 18.51562500061451289, 3.027376345333611329, 5.243569643749999010 ) ) ;
#15767 = CARTESIAN_POINT ( 'NONE',  ( 26.40000000122902790, 5.773502691896255534, 3.535250795749688894E-16 ) ) ;
#15768 = CARTESIAN_POINT ( 'NONE',  ( 29.25000000122903288, -2.886751345948129988, 4.999999999999997335 ) ) ;
#15769 = CARTESIAN_POINT ( 'NONE',  ( 23.66250000000000142, 2.886751345948126879, 4.999999999999999112 ) ) ;
#15770 = CARTESIAN_POINT ( 'NONE',  ( 3.756430356250000546, 13.57812499938548711, 27.83122392262697886 ) ) ;
#15771 = CARTESIAN_POINT ( 'NONE',  ( 24.68437500061451573, 6.421520780324663323E-16, -5.243569643749999010 ) ) ;
#15772 = CARTESIAN_POINT ( 'NONE',  ( 11.77500000000000036, 6.123233995736764310E-16, -4.999999999999998224 ) ) ;
#15773 = CARTESIAN_POINT ( 'NONE',  ( 11.77500000122903501, -5.773502691896255534, -1.060575238724906372E-15 ) ) ;
#15774 = EDGE_CURVE ( 'NONE', #26800, #29126, #35052, .T. ) ;
#15775 = CARTESIAN_POINT ( 'NONE',  ( 29.40937500061451715, 0.000000000000000000, 5.243569643749999010 ) ) ;
#15776 = CARTESIAN_POINT ( 'NONE',  ( -4.000000000000000888, 18.55624999877096570, 32.30940107675850470 ) ) ;
#15777 = CARTESIAN_POINT ( 'NONE',  ( 5.596875000614516260, -3.027376345333614438, 5.243569643749998122 ) ) ;
#15778 = CARTESIAN_POINT ( 'NONE',  ( 25.56562500061452070, 3.027376345333613106, -5.243569643749998122 ) ) ;
#15779 = CARTESIAN_POINT ( 'NONE',  ( -1.878215178125001827, 13.05312499938548321, 33.25316411605952283 ) ) ;
#15780 = CARTESIAN_POINT ( 'NONE',  ( -1.626862140677534273E-15, 20.03749999999999787, 34.00000000000000000 ) ) ;
#15781 = CARTESIAN_POINT ( 'NONE',  ( 10.92187500061451644, 3.027376345333611329, 5.243569643749999010 ) ) ;
#15782 = CARTESIAN_POINT ( 'NONE',  ( 4.247151432104769420, -2.638504256727666863, 4.531370421416291983 ) ) ;
#15783 = CARTESIAN_POINT ( 'NONE',  ( 28.79062500061451502, 6.054752690667223547, 3.707466751127219781E-16 ) ) ;
#15784 = CARTESIAN_POINT ( 'NONE',  ( 9.646875000614516082, -3.027376345333614438, 5.243569643749998122 ) ) ;
#15785 = CARTESIAN_POINT ( 'NONE',  ( 28.05937500061451573, 0.000000000000000000, 5.243569643749999010 ) ) ;
#15786 = EDGE_CURVE ( 'NONE', #40370, #60188, #39834, .T. ) ;
#15787 = CARTESIAN_POINT ( 'NONE',  ( 4.243569643749999010, 12.41562500061459673, 27.54997392385601174 ) ) ;
#15788 = CARTESIAN_POINT ( 'NONE',  ( 21.15000000000000213, -4.330127018922190985, -2.500000000000001332 ) ) ;
#15789 = ORIENTED_EDGE ( 'NONE', *, *, #34218, .T. ) ;
#15790 = CARTESIAN_POINT ( 'NONE',  ( 29.43750000000000000, 5.773502691896255534, 3.535250795749688894E-16 ) ) ;
#15791 =( BOUNDED_SURFACE ( )  B_SPLINE_SURFACE ( 1, 2, ( 
 ( #4441, #26969, #21404, #31033, #70565, #43961, #59097, #8503, #711, #44694, #27692, #67941, #45771, #16587, #73116, #4797, #10694, #27331, #22498, #49863, #50230, #28410, #55764, #56485, #61656, #38782, #23218, #17314, #51307, #15861, #39874, #50946, #67226, #45048, #39138, #5877, #38406, #60929, #32866, #56129, #11055, #33583, #28768, #5522, #72386, #21767, #66858, #62386, #50588, #67583, #10332, #11785, #16229, #345, #55402, #6240, #28060, #5157, #33942, #22851, #61300, #16949, #72755, #44329, #33225, #39502, #11425, #22140, #62026, #45405, #34301, #56833, #40960, #68668, #69031, #35036, #35758, #34667, #18032, #40588, #8054, #25034, #63108, #12508, #24311, #23585, #41671, #46858, #19116, #57196, #57564, #41317, #62749, #36127, #46130, #30588, #53114, #7686, #46492, #63475, #12863, #2158, #2512, #6967, #18392, #29498, #58279, #6611, #52034, #1437, #68307, #17666, #23943, #35394, #69398, #57920, #64194, #18753, #13581, #29139, #7327, #63827, #12142, #58646, #29858, #40227, #51672, #30223, #52394, #1801, #13219, #24670, #1077, #52756, #47216, #69748, #43775, #72213, #66302, #38217, #15679, #55947, #67051, #2876, #66673, #30943, #38597, #31315, #48316, #21591, #53484, #8781, #14318, #25407, #13952, #55226, #60744, #21223, #55586, #42406, #47950, #42041, #36490, #59009, #10155, #33409, #5343, #3250, #59370, #27513, #47577, #70839, #32687, #8413, #64928, #70478, #4621, #19855, #53859, #61124, #36854, #16048, #27150, #25777, #70107, #50047, #10876, #19483, #72574, #10519, #49684, #44145, #33047, #4981, #64564, #21960, #44516, #16410, #38965, #61482, #40776, #23041, #39329, #33772, #5704, #51851, #62570, #6424, #12682, #6788, #28239, #62925, #57740, #18206, #529, #17136, #45952, #40407, #50771, #51132, #11609, #27882, #63289, #56666, #23403, #56314, #45598, #22322, #34127, #35219, #68129, #29322, #57019, #1255, #174, #6062, #23759, #68482, #17846, #17495, #67762, #50416, #12319, #57381, #46312, #45229, #61843, #11248, #22679, #28957, #39695, #68847, #11965, #34854, #40056, #28596, #34490, #51496, #72940, #62214, #44875, #896, #67410, #16772, #7146, #52934, #64744, #46675, #13039, #25211, #19666 ),
 ( #2696, #41850, #24849, #24491, #47758, #59189, #1616, #70295, #30765, #13769, #31128, #14134, #64011, #64378, #69570, #29677, #20028, #24125, #2331, #52574, #36310, #47035, #47395, #1982, #58459, #69926, #42220, #42584, #36670, #69215, #8599, #18931, #37034, #30406, #58825, #41491, #13391, #8235, #35936, #18573, #53296, #25592, #7870, #53669, #48130, #3061, #41140, #19295, #63648, #35576, #70654, #65110, #58097, #14500, #52213, #7503, #30035, #20401, #71023, #43688, #48863, #42949, #44055, #71766, #15229, #21502, #66211, #21136, #9698, #66958, #15589, #59558, #10430, #4170, #31503, #26700, #38131, #21868, #8972, #60653, #3439, #32231, #31868, #10068, #3803, #54766, #54403, #37767, #49233, #4536, #72482, #55138, #48498, #27064, #71395, #16324, #32599, #49595, #20769, #43325, #72120, #60286, #65477, #66581, #4892, #65846, #15958, #27427, #32961, #14867, #26326, #25958, #37406, #38508, #61032, #59929, #55497, #49958, #44430, #54043, #9336, #50330, #22948, #28156, #22236, #23314, #51043, #67676, #807, #45509, #439, #62125, #46223, #68040, #38877, #62841, #56578, #10789, #5975, #17409, #1167, #61396, #39966, #40318, #62480, #12233, #44792, #45143, #34762, #34402, #56930, #11517, #5620, #23676, #6334, #68397, #57297, #56227, #72854, #67324, #16684, #11878, #50684, #6702, #28865, #51404, #28505, #17046, #34039, #39604, #29235, #39240, #33324, #45863, #61754, #17758, #55862, #51768, #68762, #5251, #11156, #27793, #33683, #87, #22592, #36584, #18120, #24764, #59104, #69129, #47307, #13678, #52850, #35847, #35491, #36222, #70201, #12599, #8149, #41761, #69842, #42133, #2604, #1898, #2248, #7419, #40684, #31040, #64290, #35131, #8511, #18487, #53576, #2974, #30676, #69488, #13309, #58372, #25125, #25502, #53208, #58738, #19207, #7783, #47667, #30320, #19577, #64659, #48047, #63202, #46587, #14044, #1530, #57656, #24402, #18847, #7062, #24037, #52487, #58011, #41053, #29590, #52128, #63566, #63924, #12954, #29947, #46951, #41408, #36950, #59470, #15140, #55409, #4804, #26240, #9248, #49505, #27337, #71301, #54676, #8880, #65386, #31415, #4079, #53955, #31783, #9973, #37319, #38042, #43237, #20311 ) ),
 .UNSPECIFIED., .F., .F., .F. ) 
 B_SPLINE_SURFACE_WITH_KNOTS ( ( 2, 2 ),
 ( 3, 2, 2, 2, 2, 2, 2, 2, 2, 2, 2, 2, 2, 2, 2, 2, 2, 2, 2, 2, 2, 2, 2, 2, 2, 2, 2, 2, 2, 2, 2, 2, 2, 2, 2, 2, 2, 2, 2, 2, 2, 2, 2, 2, 2, 2, 2, 2, 2, 2, 2, 2, 2, 2, 2, 2, 2, 2, 2, 2, 2, 2, 2, 2, 2, 2, 2, 2, 2, 2, 2, 2, 2, 2, 2, 2, 2, 2, 2, 2, 2, 2, 2, 2, 2, 2, 2, 2, 2, 2, 2, 2, 2, 2, 2, 2, 2, 2, 2, 2, 2, 2, 2, 2, 2, 2, 2, 2, 2, 2, 2, 2, 2, 2, 2, 2, 2, 2, 2, 2, 2, 2, 2, 2, 2, 2, 2, 2, 2, 2, 2, 2, 2, 2, 2, 3 ),
 ( 0.000000000000000000, 1.000000000000000000 ),
 ( 0.000000000000000000, 0.007246376811594202987, 0.01449275362318840597, 0.02173913043478260809, 0.02898550724637681195, 0.03623188405797101580, 0.04347826086956521618, 0.05072463768115942351, 0.05797101449275362389, 0.06521739130434782428, 0.07246376811594203160, 0.07971014492753622505, 0.08695652173913043237, 0.09420289855072463969, 0.1014492753623188470, 0.1086956521739130405, 0.1159420289855072478, 0.1231884057971014551, 0.1304347826086956486, 0.1376811594202898559, 0.1449275362318840632, 0.1521739130434782705, 0.1594202898550724501, 0.1666666666666666574, 0.1739130434782608647, 0.1811594202898550721, 0.1884057971014492794, 0.1956521739130434867, 0.2028985507246376940, 0.2101449275362318736, 0.2173913043478260809, 0.2246376811594202882, 0.2318840579710144956, 0.2391304347826087029, 0.2463768115942029102, 0.2536231884057971175, 0.2608695652173912971, 0.2681159420289855322, 0.2753623188405797118, 0.2826086956521738913, 0.2898550724637681264, 0.2971014492753623060, 0.3043478260869565410, 0.3115942028985507206, 0.3188405797101449002, 0.3260869565217391353, 0.3333333333333333148, 0.3405797101449275499, 0.3478260869565217295, 0.3550724637681159646, 0.3623188405797101441, 0.3695652173913043237, 0.3768115942028985588, 0.3840579710144927383, 0.3913043478260869734, 0.3985507246376811530, 0.4057971014492753881, 0.4130434782608695676, 0.4202898550724637472, 0.4275362318840579823, 0.4347826086956521618, 0.4420289855072463969, 0.4492753623188405765, 0.4565217391304347561, 0.4637681159420289911, 0.4710144927536231707, 0.4782608695652174058, 0.4855072463768115854, 0.4927536231884058204, 0.5000000000000000000, 0.5072463768115942351, 0.5144927536231883591, 0.5217391304347825942, 0.5289855072463768293, 0.5362318840579710644, 0.5434782608695651884, 0.5507246376811594235, 0.5579710144927536586, 0.5652173913043477826, 0.5724637681159420177, 0.5797101449275362528, 0.5869565217391304879, 0.5942028985507246119, 0.6014492753623188470, 0.6086956521739130821, 0.6159420289855072062, 0.6231884057971014412, 0.6304347826086956763, 0.6376811594202898004, 0.6449275362318840354, 0.6521739130434782705, 0.6594202898550725056, 0.6666666666666666297, 0.6739130434782608647, 0.6811594202898550998, 0.6884057971014492239, 0.6956521739130434590, 0.7028985507246376940, 0.7101449275362319291, 0.7173913043478260532, 0.7246376811594202882, 0.7318840579710145233, 0.7391304347826086474, 0.7463768115942028825, 0.7536231884057971175, 0.7608695652173913526, 0.7681159420289854767, 0.7753623188405797118, 0.7826086956521739468, 0.7898550724637680709, 0.7971014492753623060, 0.8043478260869565410, 0.8115942028985507761, 0.8188405797101449002, 0.8260869565217391353, 0.8333333333333333703, 0.8405797101449274944, 0.8478260869565217295, 0.8550724637681159646, 0.8623188405797101996, 0.8695652173913043237, 0.8768115942028985588, 0.8840579710144927938, 0.8913043478260869179, 0.8985507246376811530, 0.9057971014492753881, 0.9130434782608695121, 0.9202898550724637472, 0.9275362318840579823, 0.9347826086956522174, 0.9420289855072463414, 0.9492753623188405765, 0.9565217391304348116, 0.9637681159420289356, 0.9662082893573751274, 0.9758703722509488587 ),
 .UNSPECIFIED. ) 
 GEOMETRIC_REPRESENTATION_ITEM ( )  RATIONAL_B_SPLINE_SURFACE ( (
 ( 1.000000000000000000, 0.8660254037844387076, 1.000000000000000000, 0.8660254037844387076, 1.000000000000000000, 0.8660254037844387076, 1.000000000000000000, 0.8660254037844387076, 1.000000000000000000, 0.8660254037844387076, 1.000000000000000000, 0.8660254037844387076, 1.000000000000000000, 0.8660254037844387076, 1.000000000000000000, 0.8660254037844387076, 1.000000000000000000, 0.8660254037844387076, 1.000000000000000000, 0.8660254037844387076, 1.000000000000000000, 0.8660254037844387076, 1.000000000000000000, 0.8660254037844387076, 1.000000000000000000, 0.8660254037844387076, 1.000000000000000000, 0.8660254037844387076, 1.000000000000000000, 0.8660254037844387076, 1.000000000000000000, 0.8660254037844387076, 1.000000000000000000, 0.8660254037844387076, 1.000000000000000000, 0.8660254037844387076, 1.000000000000000000, 0.8660254037844387076, 1.000000000000000000, 0.8660254037844387076, 1.000000000000000000, 0.8660254037844387076, 1.000000000000000000, 0.8660254037844387076, 1.000000000000000000, 0.8660254037844387076, 1.000000000000000000, 0.8660254037844387076, 1.000000000000000000, 0.8660254037844387076, 1.000000000000000000, 0.8660254037844387076, 1.000000000000000000, 0.8660254037844387076, 1.000000000000000000, 0.8660254037844387076, 1.000000000000000000, 0.8660254037844387076, 1.000000000000000000, 0.8660254037844387076, 1.000000000000000000, 0.8660254037844387076, 1.000000000000000000, 0.8660254037844387076, 1.000000000000000000, 0.8660254037844387076, 1.000000000000000000, 0.8660254037844387076, 1.000000000000000000, 0.8660254037844387076, 1.000000000000000000, 0.8660254037844387076, 1.000000000000000000, 0.8660254037844387076, 1.000000000000000000, 0.8660254037844387076, 1.000000000000000000, 0.8660254037844387076, 1.000000000000000000, 0.8660254037844387076, 1.000000000000000000, 0.8660254037844387076, 1.000000000000000000, 0.8660254037844387076, 1.000000000000000000, 0.8660254037844387076, 1.000000000000000000, 0.8660254037844387076, 1.000000000000000000, 0.8660254037844387076, 1.000000000000000000, 0.8660254037844387076, 1.000000000000000000, 0.8660254037844387076, 1.000000000000000000, 0.8660254037844387076, 1.000000000000000000, 0.8660254037844387076, 1.000000000000000000, 0.8660254037844387076, 1.000000000000000000, 0.8660254037844387076, 1.000000000000000000, 0.8660254037844387076, 1.000000000000000000, 0.8660254037844387076, 1.000000000000000000, 0.8660254037844387076, 1.000000000000000000, 0.8660254037844387076, 1.000000000000000000, 0.8660254037844387076, 1.000000000000000000, 0.8660254037844387076, 1.000000000000000000, 0.8660254037844387076, 1.000000000000000000, 0.8660254037844387076, 1.000000000000000000, 0.8660254037844387076, 1.000000000000000000, 0.8660254037844387076, 1.000000000000000000, 0.8660254037844387076, 1.000000000000000000, 0.8660254037844387076, 1.000000000000000000, 0.8660254037844387076, 1.000000000000000000, 0.8660254037844387076, 1.000000000000000000, 0.8660254037844387076, 1.000000000000000000, 0.8660254037844387076, 1.000000000000000000, 0.8660254037844387076, 1.000000000000000000, 0.8660254037844387076, 1.000000000000000000, 0.8660254037844387076, 1.000000000000000000, 0.8660254037844387076, 1.000000000000000000, 0.8660254037844387076, 1.000000000000000000, 0.8660254037844387076, 1.000000000000000000, 0.8660254037844387076, 1.000000000000000000, 0.8660254037844387076, 1.000000000000000000, 0.8660254037844387076, 1.000000000000000000, 0.8660254037844387076, 1.000000000000000000, 0.8660254037844387076, 1.000000000000000000, 0.8660254037844387076, 1.000000000000000000, 0.8660254037844387076, 1.000000000000000000, 0.8660254037844387076, 1.000000000000000000, 0.8660254037844387076, 1.000000000000000000, 0.8660254037844387076, 1.000000000000000000, 0.8660254037844387076, 1.000000000000000000, 0.8660254037844387076, 1.000000000000000000, 0.8660254037844387076, 1.000000000000000000, 0.8660254037844387076, 1.000000000000000000, 0.8660254037844387076, 1.000000000000000000, 0.8660254037844387076, 1.000000000000000000, 0.8660254037844387076, 1.000000000000000000, 0.8660254037844387076, 1.000000000000000000, 0.8660254037844387076, 1.000000000000000000, 0.8660254037844387076, 1.000000000000000000, 0.8660254037844387076, 1.000000000000000000, 0.8660254037844387076, 1.000000000000000000, 0.8660254037844387076, 1.000000000000000000, 0.8660254037844387076, 1.000000000000000000, 0.8660254037844387076, 1.000000000000000000, 0.8660254037844387076, 1.000000000000000000, 0.8660254037844387076, 1.000000000000000000, 0.8660254037844387076, 1.000000000000000000, 0.8660254037844387076, 1.000000000000000000, 0.8660254037844387076, 1.000000000000000000, 0.8660254037844387076, 1.000000000000000000, 0.8660254037844387076, 1.000000000000000000, 0.8660254037844387076, 1.000000000000000000, 0.8660254037844387076, 1.000000000000000000, 0.8660254037844387076, 1.000000000000000000, 0.8660254037844387076, 1.000000000000000000, 0.8660254037844387076, 1.000000000000000000, 0.8660254037844387076, 1.000000000000000000, 0.8660254037844387076, 1.000000000000000000, 0.8660254037844387076, 1.000000000000000000, 0.8660254037844387076, 1.000000000000000000, 0.8660254037844387076, 1.000000000000000000, 0.8660254037844387076, 1.000000000000000000, 0.8660254037844387076, 1.000000000000000000, 0.8660254037844387076, 1.000000000000000000, 0.8660254037844387076, 1.000000000000000000, 0.8660254037844387076, 1.000000000000000000, 0.8660254037844387076, 1.000000000000000000, 0.8660254037844387076, 1.000000000000000000, 0.8660254037844387076, 1.000000000000000000, 0.8660254037844387076, 1.000000000000000000, 0.8660254037844387076, 1.000000000000000000, 0.8660254037844387076, 1.000000000000000000, 0.8660254037844387076, 1.000000000000000000, 0.8660254037844387076, 1.000000000000000000, 0.8660254037844387076, 1.000000000000000000, 0.8660254037844387076, 1.000000000000000000, 0.8660254037844387076, 1.000000000000000000, 0.8660254037844387076, 1.000000000000000000, 0.8660254037844387076, 1.000000000000000000, 0.9548848677736607726, 0.9401542295229587953, 0.9401542295229587953, 0.9401542295229587953),
 ( 1.000000000000000000, 0.8660254037844387076, 1.000000000000000000, 0.8660254037844387076, 1.000000000000000000, 0.8660254037844387076, 1.000000000000000000, 0.8660254037844387076, 1.000000000000000000, 0.8660254037844387076, 1.000000000000000000, 0.8660254037844387076, 1.000000000000000000, 0.8660254037844387076, 1.000000000000000000, 0.8660254037844387076, 1.000000000000000000, 0.8660254037844387076, 1.000000000000000000, 0.8660254037844387076, 1.000000000000000000, 0.8660254037844387076, 1.000000000000000000, 0.8660254037844387076, 1.000000000000000000, 0.8660254037844387076, 1.000000000000000000, 0.8660254037844387076, 1.000000000000000000, 0.8660254037844387076, 1.000000000000000000, 0.8660254037844387076, 1.000000000000000000, 0.8660254037844387076, 1.000000000000000000, 0.8660254037844387076, 1.000000000000000000, 0.8660254037844387076, 1.000000000000000000, 0.8660254037844387076, 1.000000000000000000, 0.8660254037844387076, 1.000000000000000000, 0.8660254037844387076, 1.000000000000000000, 0.8660254037844387076, 1.000000000000000000, 0.8660254037844387076, 1.000000000000000000, 0.8660254037844387076, 1.000000000000000000, 0.8660254037844387076, 1.000000000000000000, 0.8660254037844387076, 1.000000000000000000, 0.8660254037844387076, 1.000000000000000000, 0.8660254037844387076, 1.000000000000000000, 0.8660254037844387076, 1.000000000000000000, 0.8660254037844387076, 1.000000000000000000, 0.8660254037844387076, 1.000000000000000000, 0.8660254037844387076, 1.000000000000000000, 0.8660254037844387076, 1.000000000000000000, 0.8660254037844387076, 1.000000000000000000, 0.8660254037844387076, 1.000000000000000000, 0.8660254037844387076, 1.000000000000000000, 0.8660254037844387076, 1.000000000000000000, 0.8660254037844387076, 1.000000000000000000, 0.8660254037844387076, 1.000000000000000000, 0.8660254037844387076, 1.000000000000000000, 0.8660254037844387076, 1.000000000000000000, 0.8660254037844387076, 1.000000000000000000, 0.8660254037844387076, 1.000000000000000000, 0.8660254037844387076, 1.000000000000000000, 0.8660254037844387076, 1.000000000000000000, 0.8660254037844387076, 1.000000000000000000, 0.8660254037844387076, 1.000000000000000000, 0.8660254037844387076, 1.000000000000000000, 0.8660254037844387076, 1.000000000000000000, 0.8660254037844387076, 1.000000000000000000, 0.8660254037844387076, 1.000000000000000000, 0.8660254037844387076, 1.000000000000000000, 0.8660254037844387076, 1.000000000000000000, 0.8660254037844387076, 1.000000000000000000, 0.8660254037844387076, 1.000000000000000000, 0.8660254037844387076, 1.000000000000000000, 0.8660254037844387076, 1.000000000000000000, 0.8660254037844387076, 1.000000000000000000, 0.8660254037844387076, 1.000000000000000000, 0.8660254037844387076, 1.000000000000000000, 0.8660254037844387076, 1.000000000000000000, 0.8660254037844387076, 1.000000000000000000, 0.8660254037844387076, 1.000000000000000000, 0.8660254037844387076, 1.000000000000000000, 0.8660254037844387076, 1.000000000000000000, 0.8660254037844387076, 1.000000000000000000, 0.8660254037844387076, 1.000000000000000000, 0.8660254037844387076, 1.000000000000000000, 0.8660254037844387076, 1.000000000000000000, 0.8660254037844387076, 1.000000000000000000, 0.8660254037844387076, 1.000000000000000000, 0.8660254037844387076, 1.000000000000000000, 0.8660254037844387076, 1.000000000000000000, 0.8660254037844387076, 1.000000000000000000, 0.8660254037844387076, 1.000000000000000000, 0.8660254037844387076, 1.000000000000000000, 0.8660254037844387076, 1.000000000000000000, 0.8660254037844387076, 1.000000000000000000, 0.8660254037844387076, 1.000000000000000000, 0.8660254037844387076, 1.000000000000000000, 0.8660254037844387076, 1.000000000000000000, 0.8660254037844387076, 1.000000000000000000, 0.8660254037844387076, 1.000000000000000000, 0.8660254037844387076, 1.000000000000000000, 0.8660254037844387076, 1.000000000000000000, 0.8660254037844387076, 1.000000000000000000, 0.8660254037844387076, 1.000000000000000000, 0.8660254037844387076, 1.000000000000000000, 0.8660254037844387076, 1.000000000000000000, 0.8660254037844387076, 1.000000000000000000, 0.8660254037844387076, 1.000000000000000000, 0.8660254037844387076, 1.000000000000000000, 0.8660254037844387076, 1.000000000000000000, 0.8660254037844387076, 1.000000000000000000, 0.8660254037844387076, 1.000000000000000000, 0.8660254037844387076, 1.000000000000000000, 0.8660254037844387076, 1.000000000000000000, 0.8660254037844387076, 1.000000000000000000, 0.8660254037844387076, 1.000000000000000000, 0.8660254037844387076, 1.000000000000000000, 0.8660254037844387076, 1.000000000000000000, 0.8660254037844387076, 1.000000000000000000, 0.8660254037844387076, 1.000000000000000000, 0.8660254037844387076, 1.000000000000000000, 0.8660254037844387076, 1.000000000000000000, 0.8660254037844387076, 1.000000000000000000, 0.8660254037844387076, 1.000000000000000000, 0.8660254037844387076, 1.000000000000000000, 0.8660254037844387076, 1.000000000000000000, 0.8660254037844387076, 1.000000000000000000, 0.8660254037844387076, 1.000000000000000000, 0.8660254037844387076, 1.000000000000000000, 0.8660254037844387076, 1.000000000000000000, 0.8660254037844387076, 1.000000000000000000, 0.8660254037844387076, 1.000000000000000000, 0.8660254037844387076, 1.000000000000000000, 0.8660254037844387076, 1.000000000000000000, 0.8660254037844387076, 1.000000000000000000, 0.8660254037844387076, 1.000000000000000000, 0.8660254037844387076, 1.000000000000000000, 0.8660254037844387076, 1.000000000000000000, 0.8660254037844387076, 1.000000000000000000, 0.8660254037844387076, 1.000000000000000000, 0.8660254037844387076, 1.000000000000000000, 0.8660254037844387076, 1.000000000000000000, 0.8660254037844387076, 1.000000000000000000, 0.8660254037844387076, 1.000000000000000000, 0.8660254037844387076, 1.000000000000000000, 0.8660254037844387076, 1.000000000000000000, 0.8660254037844387076, 1.000000000000000000, 0.8660254037844387076, 1.000000000000000000, 0.8660254037844387076, 1.000000000000000000, 0.9548848677736607726, 0.9401542295229587953, 0.9401542295229587953, 0.9401542295229587953) ) ) 
 REPRESENTATION_ITEM ( '' )  SURFACE ( )  );
#15792 = CARTESIAN_POINT ( 'NONE',  ( 4.949999999999999289, -4.330127018922190985, -2.500000000000001332 ) ) ;
#15793 = ORIENTED_EDGE ( 'NONE', *, *, #13955, .F. ) ;
#15794 = CARTESIAN_POINT ( 'NONE',  ( 19.07812500061451644, -4.541064518000419881, 2.621784821874995952 ) ) ;
#15795 = CARTESIAN_POINT ( 'NONE',  ( 11.54062500061451857, -3.027376345333610441, -5.243569643749999898 ) ) ;
#15796 = CARTESIAN_POINT ( 'NONE',  ( 20.70937500061451786, 2.746126346562643317, 4.756430356249998326 ) ) ;
#15797 = CARTESIAN_POINT ( 'NONE',  ( 7.734375000614517326, 4.541064518000418104, 2.621784821874999949 ) ) ;
#15798 = CARTESIAN_POINT ( 'NONE',  ( 19.31250000122903288, 0.000000000000000000, 4.999999999999998224 ) ) ;
#15799 = CARTESIAN_POINT ( 'NONE',  ( 23.96250000122903145, -4.330127018922190985, -2.500000000000001332 ) ) ;
#15800 = CARTESIAN_POINT ( 'NONE',  ( 6.459375000614518747, 0.000000000000000000, 5.243569643749999010 ) ) ;
#15801 = CARTESIAN_POINT ( 'NONE',  ( 14.74687500061451573, -3.027376345333610441, -5.243569643749999898 ) ) ;
#15802 = CARTESIAN_POINT ( 'NONE',  ( 24.08437500061451786, -4.541064518000419881, 2.621784821874995952 ) ) ;
#15803 = CARTESIAN_POINT ( 'NONE',  ( 1.071796769724484344, 15.74509619066136956, -25.99999999999999645 ) ) ;
#15804 = VERTEX_POINT ( 'NONE', #70223 ) ;
#15805 = CARTESIAN_POINT ( 'NONE',  ( 12.37500000000000000, 4.330127018922191873, 2.499999999999999556 ) ) ;
#15806 = CARTESIAN_POINT ( 'NONE',  ( 17.22187500061451715, 3.027376345333611329, 5.243569643749999010 ) ) ;
#15807 = CARTESIAN_POINT ( 'NONE',  ( 9.984375000614518214, 4.541064518000418104, 2.621784821874999949 ) ) ;
#15808 = CARTESIAN_POINT ( 'NONE',  ( 1.878215178124997609, 15.71562499938548108, 33.25316411605952993 ) ) ;
#15809 = CARTESIAN_POINT ( 'NONE',  ( 21.15000000000000213, -4.330127018922190985, -2.500000000000001332 ) ) ;
#15810 = CARTESIAN_POINT ( 'NONE',  ( 2.000000000000000444, 17.07499999999999929, 26.53589838486224650 ) ) ;
#15811 = CARTESIAN_POINT ( 'NONE',  ( -1.071796769724490339, 17.13259618943233420, 26.00000000000000000 ) ) ;
#15812 = CARTESIAN_POINT ( 'NONE',  ( 23.03437500061451715, 4.119189519843966529, 2.378215178124999607 ) ) ;
#15813 = CARTESIAN_POINT ( 'NONE',  ( 12.74062500061451786, -3.027376345333614438, 5.243569643749998122 ) ) ;
#15814 = CARTESIAN_POINT ( 'NONE',  ( 28.80937500061451573, 4.541064518000418104, -2.621784821874998173 ) ) ;
#15815 = LINE ( 'NONE', #71620, #50226 ) ;
#15816 = CARTESIAN_POINT ( 'NONE',  ( 9.712500000000002132, 2.886751345948126879, 4.999999999999999112 ) ) ;
#15817 = CARTESIAN_POINT ( 'NONE',  ( 2.000000000000001332, 15.76250000122903216, 33.46410161513774995 ) ) ;
#15818 = CARTESIAN_POINT ( 'NONE',  ( 12.56250000122903465, 0.000000000000000000, 4.999999999999998224 ) ) ;
#15819 = CARTESIAN_POINT ( 'NONE',  ( 22.80937500061451573, -4.541064518000417216, -2.621784821875001281 ) ) ;
#15820 = CARTESIAN_POINT ( 'NONE',  ( 15.15937500061451715, -4.541064518000417216, -2.621784821875001281 ) ) ;
#15821 = CARTESIAN_POINT ( 'NONE',  ( 3.999999999999999112, 16.73750000122903359, 30.00000000000000000 ) ) ;
#15822 = ORIENTED_EDGE ( 'NONE', *, *, #67839, .F. ) ;
#15823 = AXIS2_PLACEMENT_3D ( 'NONE', #72302, #56041, #56402 ) ;
#15824 = CARTESIAN_POINT ( 'NONE',  ( 16.52812500061451573, 6.421520780324663323E-16, -5.243569643749999010 ) ) ;
#15825 = CARTESIAN_POINT ( 'NONE',  ( 28.80000000122903003, -2.886751345948129988, 4.999999999999997335 ) ) ;
#15826 = CARTESIAN_POINT ( 'NONE',  ( 14.74687500061451573, -3.027376345333610441, -5.243569643749999898 ) ) ;
#15827 = CARTESIAN_POINT ( 'NONE',  ( 1.391695283777659053, 9.904653401742692154, -24.16020628980599483 ) ) ;
#15828 = CARTESIAN_POINT ( 'NONE',  ( 19.56562500061451715, -6.054752690667223547, -1.112240025338166033E-15 ) ) ;
#15829 = CARTESIAN_POINT ( 'NONE',  ( 3.999999999999998668, 16.66250000000000142, -32.30940107675850470 ) ) ;
#15830 = CARTESIAN_POINT ( 'NONE',  ( 27.64687500061452141, -3.027376345333614438, 5.243569643749998122 ) ) ;
#15831 = CARTESIAN_POINT ( 'NONE',  ( 9.001249775931846008E-16, 12.71562500061451750, 34.90005215228797653 ) ) ;
#15832 = CARTESIAN_POINT ( 'NONE',  ( 16.47187500061452070, -6.054752690667223547, -1.112240025338166033E-15 ) ) ;
#15833 = CARTESIAN_POINT ( 'NONE',  ( 15.37500000122903465, -5.773502691896255534, -1.060575238724906372E-15 ) ) ;
#15834 = CARTESIAN_POINT ( 'NONE',  ( 10.17187500061451999, -5.492252693125287522, -1.008910452111647106E-15 ) ) ;
#15835 = CARTESIAN_POINT ( 'NONE',  ( 4.243569643749999898, 18.28437500061451715, -30.00000000000000000 ) ) ;
#15836 = CARTESIAN_POINT ( 'NONE',  ( 20.10937500061451289, -4.541064518000417216, -2.621784821875001281 ) ) ;
#15837 = CARTESIAN_POINT ( 'NONE',  ( 23.66250000122903430, 4.330127018922192761, -2.499999999999997780 ) ) ;
#15838 = CARTESIAN_POINT ( 'NONE',  ( 16.02187500061451786, -6.054752690667223547, -1.112240025338166033E-15 ) ) ;
#15839 = CARTESIAN_POINT ( 'NONE',  ( 11.72812500061451857, 4.541064518000418104, 2.621784821874999949 ) ) ;
#15840 = CARTESIAN_POINT ( 'NONE',  ( -2.121784821874999949, 13.03437500061451715, 26.32496088578401938 ) ) ;
#15841 = CARTESIAN_POINT ( 'NONE',  ( 17.24062500061451786, -3.027376345333614438, 5.243569643749998122 ) ) ;
#15842 = ORIENTED_EDGE ( 'NONE', *, *, #22474, .F. ) ;
#15843 = VERTEX_POINT ( 'NONE', #19597 ) ;
#15844 = CARTESIAN_POINT ( 'NONE',  ( 19.72499999999999787, -4.330127018922194537, 2.499999999999995559 ) ) ;
#15845 = CARTESIAN_POINT ( 'NONE',  ( 17.51249999999999929, -5.773502691896255534, -1.060575238724906372E-15 ) ) ;
#15846 = CARTESIAN_POINT ( 'NONE',  ( 23.69062500061451004, -3.027376345333610441, -5.243569643749999898 ) ) ;
#15847 = CARTESIAN_POINT ( 'NONE',  ( 6.065625000614516260, -6.054752690667223547, -1.112240025338166033E-15 ) ) ;
#15848 = CARTESIAN_POINT ( 'NONE',  ( 17.28750000122903430, 6.123233995736764310E-16, -4.999999999999998224 ) ) ;
#15849 = CARTESIAN_POINT ( 'NONE',  ( 23.12812500061451360, -4.541064518000419881, 2.621784821874995952 ) ) ;
#15850 = CARTESIAN_POINT ( 'NONE',  ( 22.94999999999999929, -4.330127018922190985, -2.500000000000001332 ) ) ;
#15851 = CARTESIAN_POINT ( 'NONE',  ( 26.24062500061451431, -3.027376345333614438, 5.243569643749998122 ) ) ;
#15852 = CARTESIAN_POINT ( 'NONE',  ( 4.678125000614516971, -4.541064518000419881, 2.621784821874995952 ) ) ;
#15853 =( BOUNDED_SURFACE ( )  B_SPLINE_SURFACE ( 1, 2, ( 
 ( #3264, #43887, #37965, #42781, #14691, #60860, #71592, #66413, #71217, #60121, #65674, #55332, #49793, #49064, #36867, #15790, #38331, #4001, #26154, #10263, #65301, #20594, #48694, #32428, #25792, #32795, #60486, #43152, #15063, #72318, #20966, #21699, #37600, #32065, #54597, #44256, #66788, #9892, #59385, #48330, #70855, #20229, #54965, #5449, #38712, #57125, #29069, #39070, #56418, #72687, #6536, #5088, #11715, #51605, #1005, #61231, #22785, #23512, #67872, #50519, #46061, #5809, #641, #34597, #17601, #50877, #45337, #50157, #16517, #6170, #17244, #55692, #10625, #39804, #22069, #28699, #23150, #33875, #62320, #67157, #44628, #34232, #73047, #28340, #275, #61953, #45704, #22429, #68237, #16160, #33155, #27623, #61584, #56766, #40160, #67514, #10987, #51238, #62680, #12075, #33508, #56057, #27989, #44976, #16878, #39432, #11357, #24598, #18317, #46422, #47146, #40888, #29786, #13146, #52322, #58208, #17957, #53412, #57848, #57494, #70035, #1725, #25331, #7980, #35686, #24237, #13881, #47504, #18682, #7612, #2438, #63034, #69677, #46787, #19408, #12789, #19043, #40519, #34967, #12433, #41245, #68595, #69322, #63757, #35326, #41967, #30149, #6898, #52681, #2089, #23874, #41601, #64120, #68960, #64488, #63404, #36420, #30516, #2804, #29429, #51966, #1365, #7258, #13506, #36052, #58573, #53043, #24960, #58936, #8343, #30872, #31976, #3915, #54512, #4645, #55250, #64856, #9080, #70406, #48978, #15339, #54152, #26437, #36782, #14244, #19781, #10178, #3178, #65959, #21247, #71133, #3546, #71507, #20506, #71875, #26069, #20883, #48241, #60399, #42331, #20141, #42696, #53782, #70766, #25705, #4283, #59298, #8708, #47877, #43437, #48608, #31616, #31241, #65218, #32713, #14608, #37516, #43801, #37145, #37879, #59672, #43063, #9807, #26809, #32340, #49343, #65588, #66326, #60771, #14978, #60037, #54878, #15703, #38242, #9448, #11635, #66701, #33070, #45255, #22703, #38990, #10902, #33796, #38623, #27905, #72601, #72965, #67074, #68156, #50071, #56339, #27539, #21615, #39721, #67788, #72237, #56688, #5729, #28619, #34151, #17162, #62239, #17519, #21984, #62595, #6087, #33430, #198, #44170, #16797, #11991, #39354, #55973, #50795, #5367, #44543, #51156, #16432, #557, #23067, #34514, #49709, #16073, #61147, #61505, #10542, #50440, #22347, #44899, #45622, #40080, #57043, #55609, #11275, #28264, #27175, #5005, #67435, #61868, #40802, #28984, #7529, #47061, #12706, #13063, #68510, #23430, #51522, #41875, #34878, #24517, #52960, #29701, #35243, #30062, #52238, #30432, #57764, #58121, #6812, #18957, #921, #51878, #1277, #12343, #29346, #57407, #35964, #45976, #17873, #36337, #52600, #7173, #63315, #13797, #40432, #64404, #62949, #69238, #2357, #23786, #2006, #46338, #68872, #69595, #58485, #41517, #7895, #1643, #24874, #19321, #24149, #18228, #64036, #13415, #35602, #46702, #47421, #18600, #41164, #69951, #6449, #63673, #42608, #65503, #70317, #59582, #31152, #31527, #25616, #26723, #8623, #14891, #59215, #53322, #71418, #26349, #30791, #15254, #37431, #60312, #65873, #48888, #20795, #49258, #53693, #21160, #3828, #65133, #31893, #2721, #48522, #43713, #71049, #14524, #37791, #8995, #58851, #3463, #37058, #14159, #54067, #25983, #9722, #25237, #59953, #20424, #32255, #3087, #9360, #47783, #19692, #42245, #42972, #15613, #54429, #43351, #48152, #54788, #70678, #4194, #64769, #20053, #71791, #66235, #36693, #8261, #39265, #44079, #15982, #62148, #72878, #28179, #72506, #61420, #66982, #56602, #5998, #27819, #38155, #67698, #5643, #28529, #34061, #27452, #60678, #51067, #464, #61055, #5274, #21524, #22972, #27087, #33705, #45534, #68063, #10092, #44813, #32622, #16709, #21895, #55162, #50352, #22616, #4559, #39630, #22260, #67347, #72146, #38532, #50707, #61777, #49619, #66607, #11181, #10454, #110, #45167, #55886, #56252, #32983, #55523, #17070, #44452, #11544, #4917, #10814, #49982, #16346, #38901, #33348, #30344, #47330, #7807, #58033, #41431, #68785, #52872, #41075, #12977, #69509, #13332, #2270, #35514, #23338, #62861, #7443, #46974, #46608, #40340, #68419, #69151, #12256, #51788, #35155, #1189, #7084, #39989, #24786, #6724, #6357, #18869, #23697, #17431, #29969, #57679, #46245, #35870, #63947, #52510, #63589, #24062, #45887, #1920, #56953, #17781, #24425, #58394, #29258, #18141, #18510, #28889, #40708, #34787, #63226, #57320, #62502, #12620, #11900, #29613, #34425, #51428, #830, #52149, #1552, #25896, #71328, #3737, #59866, #9270, #37701, #64682, #32170, #14800, #53601, #42887, #64313, #59493, #54703, #8906, #25523, #48799, #19967, #69863, #14436, #2995, #25149, #20334, #48066, #70225, #20703, #42155, #43261, #31805, #4108, #19229, #36246, #30698, #14067, #13703, #19599, #36606, #42520, #37343, #65782, #9636, #58760, #53977, #48436, #3375, #26636, #41783, #8170, #31063, #53230, #70961, #54343, #70592, #65410, #2627, #47689, #59127, #8534, #65046, #26262, #15164, #36970, #31437, #60222, #21803, #1022, #55438, #27728, #49533, #61691, #43626, #21436, #43993, #55073, #72057, #4473, #6553, #66148, #71703, #6914, #50266, #49895, #32898, #57512, #15526, #12452, #32536, #38817, #46078, #27003, #72791, #66515, #15895, #67262, #29086, #39175, #51621, #4830, #23528, #63051, #27364, #38442, #11090, #16620, #21075, #68613, #5190, #17974, #56162, #33618, #40535, #34984, #60968, #49172, #38068, #72420, #22174, #60592, #61332, #10001, #10730, #44367, #10368, #66894, #16262, #33262, #55800, #44727, #53061, #35703, #29803, #8360, #1741, #2821, #41985, #36800, #51982, #68977, #63420, #24255, #23891, #52339, #46803, #2105, #47523, #30889, #42350, #18334, #13523, #58591, #36071, #59315, #29444, #46438, #63774, #1381, #30534, #70052, #58224, #7998, #40907, #12806, #35342, #64873, #57865, #19425 ),
 ( #2455, #30166, #13162, #7274, #69339, #14261, #18698, #19060, #25349, #41262, #24978, #7629, #52699, #64506, #58952, #13898, #53431, #24616, #47895, #47163, #69695, #41618, #36438, #70423, #19798, #64137, #66341, #48260, #14624, #26826, #4301, #20522, #65606, #15355, #20159, #9464, #54166, #54528, #48624, #49724, #31633, #37897, #9096, #3195, #54894, #59689, #65234, #60415, #14994, #20899, #48994, #3931, #15719, #43080, #60786, #72251, #21628, #38638, #44186, #49360, #32727, #60053, #66716, #32356, #71890, #10192, #4660, #16090, #21263, #37163, #3563, #43817, #38257, #9824, #26085, #71149, #55264, #37531, #31994, #26454, #71524, #43453, #31258, #8724, #65975, #70783, #27189, #53800, #25722, #42713, #5744, #44913, #6465, #40095, #11290, #28278, #68170, #55624, #17176, #67450, #12005, #5381, #62253, #33085, #27554, #5020, #33811, #17889, #61884, #16812, #27919, #50810, #50453, #34528, #67088, #22361, #72979, #56702, #50086, #51171, #11650, #16447, #39004, #57058, #22717, #575, #39368, #56354, #212, #29000, #51537, #45270, #61162, #17533, #28633, #937, #23445, #67803, #10557, #45991, #68528, #10917, #39736, #44557, #72617, #22000, #6102, #61519, #33443, #55988, #34165, #23080, #45637, #62609, #41894, #63690, #64053, #2374, #7911, #13080, #7545, #29362, #68888, #18974, #52617, #57424, #62965, #2023, #51895, #41534, #13433, #18616, #6828, #7189, #12361, #24534, #69613, #29717, #30079, #1293, #34895, #23803, #69968, #46354, #47078, #30449, #24167, #52255, #35983, #69254, #52978, #1658, #58502, #18245, #24892, #40818, #63334, #12722, #35258, #57779, #46719, #47437, #41181, #35619, #64421, #19339, #58139, #40449, #40683, #27792, #68761, #16683, #22947, #29234, #61753, #34401, #39239, #86, #51403, #62840, #23313, #12232, #17045, #34761, #46222, #62124, #11155, #806, #6333, #39965, #33682, #17757, #72853, #56226, #45862, #28864, #45142, #39603, #62479, #44791, #34038, #5619, #5974, #22591, #1166, #28155, #11877, #50683, #50329, #68396, #40317, #5250, #57296, #56929, #6701, #51767, #23675, #18119, #63201, #67675, #33323, #55861, #11516, #22235, #67323, #45508, #56577, #68039, #28504, #51042, #438, #17408, #15586, #4889, #48495, #31500, #32596, #65474, #21499, #66578, #26696, #55135, #59926, #14863, #60650, #65843, #21133, #49230, #54763, #15955, #43322, #61029, #72479, #21865, #38874, #44426, #49592, #32958, #60283, #4533, #37403, #44052, #38504, #71763, #27061, #9333, #31865, #10065, #15225, #43685, #66208, #4167, #10427, #37764, #55494, #66955, #16321, #8968, #54040, #72117, #27424, #9695, #3436, #49955, #25955, #71020, #20397, #42946, #54400, #3800, #26323, #48860, #71391, #38128, #20765, #32228, #39961, #33679, #22588, #5969, #45139, #51038, #10786, #46218, #50680, #50326, #62836, #67672, #18115, #802, #28500, #17041, #6697, #40312, #11512, #434, #68392, #55858, #17404, #39599, #12228, #5615, #62475, #33320, #27789, #5247, #34034, #61393, #62120, #56572, #28151, #22943, #83, #34757, #67320, #45504, #68034, #56925, #72850, #51399, #11872, #16680, #39236, #57292, #34397, #23309, #6329, #28860, #45858, #29230, #51763, #17753, #22232, #1162, #23671, #68756, #44788, #61750, #11152, #56223, #53571, #63561, #7778, #24032, #31035, #29585, #36217, #2969, #25497, #63197, #47302, #48042, #19202, #1893, #70567, #30315, #25120, #59099, #42128, #2243, #69837, #41756, #64285, #13673, #36579, #7057, #12593, #8506, #40679, #12949, #52845, #46581, #35126, #52123, #58733, #57651, #1525, #69124, #8144, #18482, #30671, #24397, #41048, #24759, #47662, #35486, #64654, #53203, #2599, #70196, #19572, #14039, #58006, #7414, #29942, #52482, #46946, #69483, #18842, #58367, #41403, #63919, #13304, #35842, #3708, #32139, #60196, #65752, #4444, #54317, #72030, #10336, #32868, #49865, #55405, #60562, #43963, #71296, #4800, #43596, #15496, #21406, #15863, #27333, #38038, #25869, #65381, #9969, #49501, #49141, #42859, #70935, #71670, #14772, #26235, #37674, #48772, #9608, #42496, #19943, #9243, #8875, #66484, #20675, #65019, #32506, #54672, #43232, #38411, #60932, #15136, #4075, #26972, #14408, #21044, #26603, #36945, #37314, #66117, #59465, #31410, #53950, #55041, #3347, #48409, #20306, #59838, #31778, #40145, #46768, #5159, #34581, #62661, #68941, #16232, #63387, #1346, #27694, #50234, #24219, #34949, #12772, #57109, #23497, #29053, #18665, #41226, #63018, #72389, #29768, #40870, #63737, #69303, #12058, #21769, #23856, #35307, #6520, #6881, #61302, #38785, #44333, #35667, #627, #18299, #13128, #46045, #51589, #46403, #68580, #58190, #989, #51947, #23133, #57830, #66861, #45689, #68223, #17586, #17940, #40503, #52303, #10697, #33229, #30131, #7239, #12417, #57476, #7593, #55767, #29414, #1704, #42311, #48588, #7961, #53763, #36033, #19386, #70745, #9061, #42676, #31594, #36403, #54132, #65568, #8324, #58551, #20122, #25687, #59280, #30497, #37122, #19022, #53025, #65199, #48221, #64468, #58915, #8688, #64099, #53389, #24941, #25309, #41947, #20486, #2419, #31220, #47485, #47126, #14588, #59651, #24579, #3527, #3158, #26048, #71114, #43041, #14957, #37496, #70016, #60016, #9428, #30854, #52663, #69657, #64838, #2070, #14225, #2785, #41582, #47856, #13484, #13861, #70385, #19761, #36762, #38221, #32321, #10881, #4265, #5346, #44521, #39332, #54494, #71487, #65939, #26789, #26415, #54856, #49323, #4625, #50050, #33412, #44878, #20864, #16053, #61127, #38601, #61846, #31956, #48957, #66306, #3895, #27516, #55950, #27884, #22325, #72578, #37858, #71854, #21963, #61485, #10522, #21227, #9787, #33050, #43779, #15683, #49688, #60750, #21595, #43415, #16775, #10159, #15319, #50418, #32693, #60379, #67054, #72217, #55230, #72944, #67413, #27154, #44149, #38969, #66678, #55589, #4984, #16413, #28599 ) ),
 .UNSPECIFIED., .F., .F., .F. ) 
 B_SPLINE_SURFACE_WITH_KNOTS ( ( 2, 2 ),
 ( 3, 2, 2, 2, 2, 2, 2, 2, 2, 2, 2, 2, 2, 2, 2, 2, 2, 2, 2, 2, 2, 2, 2, 2, 2, 2, 2, 2, 2, 2, 2, 2, 2, 2, 2, 2, 2, 2, 2, 2, 2, 2, 2, 2, 2, 2, 2, 2, 2, 2, 2, 2, 2, 2, 2, 2, 2, 2, 2, 2, 2, 2, 2, 2, 2, 2, 2, 2, 2, 2, 2, 2, 2, 2, 2, 2, 2, 2, 2, 2, 2, 2, 2, 2, 2, 2, 2, 2, 2, 2, 2, 2, 2, 2, 2, 2, 2, 2, 2, 2, 2, 2, 2, 2, 2, 2, 2, 2, 2, 2, 2, 2, 2, 2, 2, 2, 2, 2, 2, 2, 2, 2, 2, 2, 2, 2, 2, 2, 2, 2, 2, 2, 2, 2, 2, 2, 2, 2, 2, 2, 2, 2, 2, 2, 2, 2, 2, 2, 2, 2, 2, 2, 2, 2, 2, 2, 2, 2, 2, 2, 2, 2, 2, 2, 2, 2, 2, 2, 2, 2, 2, 2, 2, 2, 2, 2, 2, 2, 2, 2, 2, 2, 2, 2, 2, 2, 2, 2, 2, 2, 2, 2, 2, 2, 2, 2, 2, 2, 2, 2, 2, 2, 2, 2, 2, 2, 2, 2, 2, 2, 2, 2, 2, 2, 2, 2, 2, 2, 2, 2, 2, 2, 2, 2, 2, 2, 2, 2, 2, 2, 2, 2, 2, 2, 2, 2, 2, 2, 2, 2, 2, 2, 2, 2, 2, 2, 2, 2, 2, 2, 2, 2, 2, 2, 2, 2, 2, 2, 2, 2, 2, 2, 2, 2, 2, 2, 2, 2, 2, 2, 2, 2, 2, 2, 2, 2, 2, 2, 2, 2, 2, 2, 2, 2, 2, 2, 2, 2, 2, 2, 2, 2, 2, 2, 2, 2, 2, 2, 2, 2, 2, 2, 2, 2, 2, 2, 2, 2, 2, 2, 2, 2, 2, 2, 2, 2, 2, 2, 2, 2, 2, 2, 2, 2, 2, 2, 2, 2, 2, 2, 2, 2, 2, 2, 2, 2, 2, 2, 2, 2, 2, 2, 2, 2, 2, 2, 2, 2, 2, 2, 2, 2, 2, 2, 2, 2, 2, 2, 2, 2, 3 ),
 ( 0.000000000000000000, 1.000000000000000000 ),
 ( 0.000000000000000000, 0.002777777777777777884, 0.005555555555555555768, 0.008333333333333333218, 0.01111111111111111154, 0.01388888888888888812, 0.01666666666666666644, 0.01944444444444444475, 0.02222222222222222307, 0.02500000000000000139, 0.02777777777777777624, 0.03055555555555555455, 0.03333333333333333287, 0.03611111111111110772, 0.03888888888888888951, 0.04166666666666666435, 0.04444444444444444614, 0.04722222222222222099, 0.05000000000000000278, 0.05277777777777777762, 0.05555555555555555247, 0.05833333333333333426, 0.06111111111111110911, 0.06388888888888888395, 0.06666666666666666574, 0.06944444444444444753, 0.07222222222222221544, 0.07499999999999999722, 0.07777777777777777901, 0.08055555555555556080, 0.08333333333333332871, 0.08611111111111111049, 0.08888888888888889228, 0.09166666666666666019, 0.09444444444444444198, 0.09722222222222222376, 0.1000000000000000056, 0.1027777777777777735, 0.1055555555555555552, 0.1083333333333333370, 0.1111111111111111049, 0.1138888888888888867, 0.1166666666666666685, 0.1194444444444444503, 0.1222222222222222182, 0.1250000000000000000, 0.1277777777777777679, 0.1305555555555555636, 0.1333333333333333315, 0.1361111111111110994, 0.1388888888888888951, 0.1416666666666666630, 0.1444444444444444309, 0.1472222222222222265, 0.1499999999999999944, 0.1527777777777777901, 0.1555555555555555580, 0.1583333333333333259, 0.1611111111111111216, 0.1638888888888888895, 0.1666666666666666574, 0.1694444444444444531, 0.1722222222222222210, 0.1749999999999999889, 0.1777777777777777846, 0.1805555555555555525, 0.1833333333333333204, 0.1861111111111111160, 0.1888888888888888840, 0.1916666666666666796, 0.1944444444444444475, 0.1972222222222222154, 0.2000000000000000111, 0.2027777777777777790, 0.2055555555555555469, 0.2083333333333333426, 0.2111111111111111105, 0.2138888888888888784, 0.2166666666666666741, 0.2194444444444444420, 0.2222222222222222099, 0.2250000000000000056, 0.2277777777777777735, 0.2305555555555555691, 0.2333333333333333370, 0.2361111111111111049, 0.2388888888888889006, 0.2416666666666666685, 0.2444444444444444364, 0.2472222222222222321, 0.2500000000000000000, 0.2527777777777777679, 0.2555555555555555358, 0.2583333333333333592, 0.2611111111111111271, 0.2638888888888888951, 0.2666666666666666630, 0.2694444444444444309, 0.2722222222222221988, 0.2750000000000000222, 0.2777777777777777901, 0.2805555555555555580, 0.2833333333333333259, 0.2861111111111110938, 0.2888888888888888618, 0.2916666666666666852, 0.2944444444444444531, 0.2972222222222222210, 0.2999999999999999889, 0.3027777777777777568, 0.3055555555555555802, 0.3083333333333333481, 0.3111111111111111160, 0.3138888888888888840, 0.3166666666666666519, 0.3194444444444444198, 0.3222222222222222432, 0.3250000000000000111, 0.3277777777777777790, 0.3305555555555555469, 0.3333333333333333148, 0.3361111111111111382, 0.3388888888888889062, 0.3416666666666666741, 0.3444444444444444420, 0.3472222222222222099, 0.3499999999999999778, 0.3527777777777778012, 0.3555555555555555691, 0.3583333333333333370, 0.3611111111111111049, 0.3638888888888888729, 0.3666666666666666408, 0.3694444444444444642, 0.3722222222222222321, 0.3750000000000000000, 0.3777777777777777679, 0.3805555555555555358, 0.3833333333333333592, 0.3861111111111111271, 0.3888888888888888951, 0.3916666666666666630, 0.3944444444444444309, 0.3972222222222221988, 0.4000000000000000222, 0.4027777777777777901, 0.4055555555555555580, 0.4083333333333333259, 0.4111111111111110938, 0.4138888888888888618, 0.4166666666666666852, 0.4194444444444444531, 0.4222222222222222210, 0.4249999999999999889, 0.4277777777777777568, 0.4305555555555555802, 0.4333333333333333481, 0.4361111111111111160, 0.4388888888888888840, 0.4416666666666666519, 0.4444444444444444198, 0.4472222222222222432, 0.4500000000000000111, 0.4527777777777777790, 0.4555555555555555469, 0.4583333333333333148, 0.4611111111111111382, 0.4638888888888889062, 0.4666666666666666741, 0.4694444444444444420, 0.4722222222222222099, 0.4749999999999999778, 0.4777777777777778012, 0.4805555555555555691, 0.4833333333333333370, 0.4861111111111111049, 0.4888888888888888729, 0.4916666666666666408, 0.4944444444444444642, 0.4972222222222222321, 0.5000000000000000000, 0.5027777777777777679, 0.5055555555555555358, 0.5083333333333333037, 0.5111111111111110716, 0.5138888888888888395, 0.5166666666666667185, 0.5194444444444444864, 0.5222222222222222543, 0.5250000000000000222, 0.5277777777777777901, 0.5305555555555555580, 0.5333333333333333259, 0.5361111111111110938, 0.5388888888888888618, 0.5416666666666666297, 0.5444444444444443976, 0.5472222222222222765, 0.5500000000000000444, 0.5527777777777778123, 0.5555555555555555802, 0.5583333333333333481, 0.5611111111111111160, 0.5638888888888888840, 0.5666666666666666519, 0.5694444444444444198, 0.5722222222222221877, 0.5749999999999999556, 0.5777777777777777235, 0.5805555555555556024, 0.5833333333333333703, 0.5861111111111111382, 0.5888888888888889062, 0.5916666666666666741, 0.5944444444444444420, 0.5972222222222222099, 0.5999999999999999778, 0.6027777777777777457, 0.6055555555555555136, 0.6083333333333332815, 0.6111111111111111605, 0.6138888888888889284, 0.6166666666666666963, 0.6194444444444444642, 0.6222222222222222321, 0.6250000000000000000, 0.6277777777777777679, 0.6305555555555555358, 0.6333333333333333037, 0.6361111111111110716, 0.6388888888888888395, 0.6416666666666667185, 0.6444444444444444864, 0.6472222222222222543, 0.6500000000000000222, 0.6527777777777777901, 0.6555555555555555580, 0.6583333333333333259, 0.6611111111111110938, 0.6638888888888888618, 0.6666666666666666297, 0.6694444444444443976, 0.6722222222222222765, 0.6750000000000000444, 0.6777777777777778123, 0.6805555555555555802, 0.6833333333333333481, 0.6861111111111111160, 0.6888888888888888840, 0.6916666666666666519, 0.6944444444444444198, 0.6972222222222221877, 0.6999999999999999556, 0.7027777777777777235, 0.7055555555555556024, 0.7083333333333333703, 0.7111111111111111382, 0.7138888888888889062, 0.7166666666666666741, 0.7194444444444444420, 0.7222222222222222099, 0.7249999999999999778, 0.7277777777777777457, 0.7305555555555555136, 0.7333333333333332815, 0.7361111111111111605, 0.7388888888888889284, 0.7416666666666666963, 0.7444444444444444642, 0.7472222222222222321, 0.7500000000000000000, 0.7527777777777777679, 0.7555555555555555358, 0.7583333333333333037, 0.7611111111111110716, 0.7638888888888888395, 0.7666666666666667185, 0.7694444444444444864, 0.7722222222222222543, 0.7750000000000000222, 0.7777777777777777901, 0.7805555555555555580, 0.7833333333333333259, 0.7861111111111110938, 0.7888888888888888618, 0.7916666666666666297, 0.7944444444444443976, 0.7972222222222222765, 0.8000000000000000444, 0.8027777777777778123, 0.8055555555555555802, 0.8083333333333333481, 0.8111111111111111160, 0.8138888888888888840, 0.8166666666666666519, 0.8194444444444444198, 0.8222222222222221877, 0.8249999999999999556, 0.8277777777777777235, 0.8305555555555556024, 0.8333333333333333703, 0.8361111111111111382, 0.8388888888888889062, 0.8416666666666666741, 0.8444444444444444420, 0.8472222222222222099, 0.8499999999999999778, 0.8527777777777777457, 0.8555555555555555136, 0.8583333333333332815, 0.8611111111111111605, 0.8638888888888889284, 0.8666666666666666963, 0.8694444444444444642, 0.8722222222222222321, 0.8750000000000000000, 0.8777777777777777679, 0.8805555555555555358, 0.8833333333333333037, 0.8861111111111110716, 0.8888888888888888395, 0.8916666666666667185, 0.8944444444444444864, 0.8972222222222222543, 0.9000000000000000222, 0.9027777777777777901, 0.9055555555555555580, 0.9083333333333333259, 0.9111111111111110938, 0.9138888888888888618, 0.9166666666666666297, 0.9194444444444443976, 0.9222222222222222765, 0.9250000000000000444, 0.9277777777777778123, 0.9305555555555555802, 0.9333333333333333481, 0.9361111111111111160, 0.9388888888888888840, 0.9416666666666666519, 0.9444444444444444198, 0.9472222222222221877, 0.9499999999999999556, 0.9527777777777777235, 0.9555555555555556024, 0.9583333333333333703, 0.9611111111111111382, 0.9638888888888889062, 0.9666666666666666741, 0.9694444444444444420, 0.9722222222222222099, 0.9749999999999999778, 0.9777777777777777457, 0.9805555555555555136, 0.9833333333333332815, 0.9861111111111111605, 0.9888888888888889284, 0.9916666666666666963, 0.9944444444444444642, 0.9972222222222222321, 1.000000000000000000 ),
 .UNSPECIFIED. ) 
 GEOMETRIC_REPRESENTATION_ITEM ( )  RATIONAL_B_SPLINE_SURFACE ( (
 ( 1.000000000000000000, 0.8660254037844387076, 1.000000000000000000, 0.8660254037844387076, 1.000000000000000000, 0.8660254037844387076, 1.000000000000000000, 0.8660254037844387076, 1.000000000000000000, 0.8660254037844387076, 1.000000000000000000, 0.8660254037844387076, 1.000000000000000000, 0.8660254037844387076, 1.000000000000000000, 0.8660254037844387076, 1.000000000000000000, 0.8660254037844387076, 1.000000000000000000, 0.8660254037844387076, 1.000000000000000000, 0.8660254037844387076, 1.000000000000000000, 0.8660254037844387076, 1.000000000000000000, 0.8660254037844387076, 1.000000000000000000, 0.8660254037844387076, 1.000000000000000000, 0.8660254037844387076, 1.000000000000000000, 0.8660254037844387076, 1.000000000000000000, 0.8660254037844387076, 1.000000000000000000, 0.8660254037844387076, 1.000000000000000000, 0.8660254037844387076, 1.000000000000000000, 0.8660254037844387076, 1.000000000000000000, 0.8660254037844387076, 1.000000000000000000, 0.8660254037844387076, 1.000000000000000000, 0.8660254037844387076, 1.000000000000000000, 0.8660254037844387076, 1.000000000000000000, 0.8660254037844387076, 1.000000000000000000, 0.8660254037844387076, 1.000000000000000000, 0.8660254037844387076, 1.000000000000000000, 0.8660254037844387076, 1.000000000000000000, 0.8660254037844387076, 1.000000000000000000, 0.8660254037844387076, 1.000000000000000000, 0.8660254037844387076, 1.000000000000000000, 0.8660254037844387076, 1.000000000000000000, 0.8660254037844387076, 1.000000000000000000, 0.8660254037844387076, 1.000000000000000000, 0.8660254037844387076, 1.000000000000000000, 0.8660254037844387076, 1.000000000000000000, 0.8660254037844387076, 1.000000000000000000, 0.8660254037844387076, 1.000000000000000000, 0.8660254037844387076, 1.000000000000000000, 0.8660254037844387076, 1.000000000000000000, 0.8660254037844387076, 1.000000000000000000, 0.8660254037844387076, 1.000000000000000000, 0.8660254037844387076, 1.000000000000000000, 0.8660254037844387076, 1.000000000000000000, 0.8660254037844387076, 1.000000000000000000, 0.8660254037844387076, 1.000000000000000000, 0.8660254037844387076, 1.000000000000000000, 0.8660254037844387076, 1.000000000000000000, 0.8660254037844387076, 1.000000000000000000, 0.8660254037844387076, 1.000000000000000000, 0.8660254037844387076, 1.000000000000000000, 0.8660254037844387076, 1.000000000000000000, 0.8660254037844387076, 1.000000000000000000, 0.8660254037844387076, 1.000000000000000000, 0.8660254037844387076, 1.000000000000000000, 0.8660254037844387076, 1.000000000000000000, 0.8660254037844387076, 1.000000000000000000, 0.8660254037844387076, 1.000000000000000000, 0.8660254037844387076, 1.000000000000000000, 0.8660254037844387076, 1.000000000000000000, 0.8660254037844387076, 1.000000000000000000, 0.8660254037844387076, 1.000000000000000000, 0.8660254037844387076, 1.000000000000000000, 0.8660254037844387076, 1.000000000000000000, 0.8660254037844387076, 1.000000000000000000, 0.8660254037844387076, 1.000000000000000000, 0.8660254037844387076, 1.000000000000000000, 0.8660254037844387076, 1.000000000000000000, 0.8660254037844387076, 1.000000000000000000, 0.8660254037844387076, 1.000000000000000000, 0.8660254037844387076, 1.000000000000000000, 0.8660254037844387076, 1.000000000000000000, 0.8660254037844387076, 1.000000000000000000, 0.8660254037844387076, 1.000000000000000000, 0.8660254037844387076, 1.000000000000000000, 0.8660254037844387076, 1.000000000000000000, 0.8660254037844387076, 1.000000000000000000, 0.8660254037844387076, 1.000000000000000000, 0.8660254037844387076, 1.000000000000000000, 0.8660254037844387076, 1.000000000000000000, 0.8660254037844387076, 1.000000000000000000, 0.8660254037844387076, 1.000000000000000000, 0.8660254037844387076, 1.000000000000000000, 0.8660254037844387076, 1.000000000000000000, 0.8660254037844387076, 1.000000000000000000, 0.8660254037844387076, 1.000000000000000000, 0.8660254037844387076, 1.000000000000000000, 0.8660254037844387076, 1.000000000000000000, 0.8660254037844387076, 1.000000000000000000, 0.8660254037844387076, 1.000000000000000000, 0.8660254037844387076, 1.000000000000000000, 0.8660254037844387076, 1.000000000000000000, 0.8660254037844387076, 1.000000000000000000, 0.8660254037844387076, 1.000000000000000000, 0.8660254037844387076, 1.000000000000000000, 0.8660254037844387076, 1.000000000000000000, 0.8660254037844387076, 1.000000000000000000, 0.8660254037844387076, 1.000000000000000000, 0.8660254037844387076, 1.000000000000000000, 0.8660254037844387076, 1.000000000000000000, 0.8660254037844387076, 1.000000000000000000, 0.8660254037844387076, 1.000000000000000000, 0.8660254037844387076, 1.000000000000000000, 0.8660254037844387076, 1.000000000000000000, 0.8660254037844387076, 1.000000000000000000, 0.8660254037844387076, 1.000000000000000000, 0.8660254037844387076, 1.000000000000000000, 0.8660254037844387076, 1.000000000000000000, 0.8660254037844387076, 1.000000000000000000, 0.8660254037844387076, 1.000000000000000000, 0.8660254037844387076, 1.000000000000000000, 0.8660254037844387076, 1.000000000000000000, 0.8660254037844387076, 1.000000000000000000, 0.8660254037844387076, 1.000000000000000000, 0.8660254037844387076, 1.000000000000000000, 0.8660254037844387076, 1.000000000000000000, 0.8660254037844387076, 1.000000000000000000, 0.8660254037844387076, 1.000000000000000000, 0.8660254037844387076, 1.000000000000000000, 0.8660254037844387076, 1.000000000000000000, 0.8660254037844387076, 1.000000000000000000, 0.8660254037844387076, 1.000000000000000000, 0.8660254037844387076, 1.000000000000000000, 0.8660254037844387076, 1.000000000000000000, 0.8660254037844387076, 1.000000000000000000, 0.8660254037844387076, 1.000000000000000000, 0.8660254037844387076, 1.000000000000000000, 0.8660254037844387076, 1.000000000000000000, 0.8660254037844387076, 1.000000000000000000, 0.8660254037844387076, 1.000000000000000000, 0.8660254037844387076, 1.000000000000000000, 0.8660254037844387076, 1.000000000000000000, 0.8660254037844387076, 1.000000000000000000, 0.8660254037844387076, 1.000000000000000000, 0.8660254037844387076, 1.000000000000000000, 0.8660254037844387076, 1.000000000000000000, 0.8660254037844387076, 1.000000000000000000, 0.8660254037844387076, 1.000000000000000000, 0.8660254037844387076, 1.000000000000000000, 0.8660254037844387076, 1.000000000000000000, 0.8660254037844387076, 1.000000000000000000, 0.8660254037844387076, 1.000000000000000000, 0.8660254037844387076, 1.000000000000000000, 0.8660254037844387076, 1.000000000000000000, 0.8660254037844387076, 1.000000000000000000, 0.8660254037844387076, 1.000000000000000000, 0.8660254037844387076, 1.000000000000000000, 0.8660254037844387076, 1.000000000000000000, 0.8660254037844387076, 1.000000000000000000, 0.8660254037844387076, 1.000000000000000000, 0.8660254037844387076, 1.000000000000000000, 0.8660254037844387076, 1.000000000000000000, 0.8660254037844387076, 1.000000000000000000, 0.8660254037844387076, 1.000000000000000000, 0.8660254037844387076, 1.000000000000000000, 0.8660254037844387076, 1.000000000000000000, 0.8660254037844387076, 1.000000000000000000, 0.8660254037844387076, 1.000000000000000000, 0.8660254037844387076, 1.000000000000000000, 0.8660254037844387076, 1.000000000000000000, 0.8660254037844387076, 1.000000000000000000, 0.8660254037844387076, 1.000000000000000000, 0.8660254037844387076, 1.000000000000000000, 0.8660254037844387076, 1.000000000000000000, 0.8660254037844387076, 1.000000000000000000, 0.8660254037844387076, 1.000000000000000000, 0.8660254037844387076, 1.000000000000000000, 0.8660254037844387076, 1.000000000000000000, 0.8660254037844387076, 1.000000000000000000, 0.8660254037844387076, 1.000000000000000000, 0.8660254037844387076, 1.000000000000000000, 0.8660254037844387076, 1.000000000000000000, 0.8660254037844387076, 1.000000000000000000, 0.8660254037844387076, 1.000000000000000000, 0.8660254037844387076, 1.000000000000000000, 0.8660254037844387076, 1.000000000000000000, 0.8660254037844387076, 1.000000000000000000, 0.8660254037844387076, 1.000000000000000000, 0.8660254037844387076, 1.000000000000000000, 0.8660254037844387076, 1.000000000000000000, 0.8660254037844387076, 1.000000000000000000, 0.8660254037844387076, 1.000000000000000000, 0.8660254037844387076, 1.000000000000000000, 0.8660254037844387076, 1.000000000000000000, 0.8660254037844387076, 1.000000000000000000, 0.8660254037844387076, 1.000000000000000000, 0.8660254037844387076, 1.000000000000000000, 0.8660254037844387076, 1.000000000000000000, 0.8660254037844387076, 1.000000000000000000, 0.8660254037844387076, 1.000000000000000000, 0.8660254037844387076, 1.000000000000000000, 0.8660254037844387076, 1.000000000000000000, 0.8660254037844387076, 1.000000000000000000, 0.8660254037844387076, 1.000000000000000000, 0.8660254037844387076, 1.000000000000000000, 0.8660254037844387076, 1.000000000000000000, 0.8660254037844387076, 1.000000000000000000, 0.8660254037844387076, 1.000000000000000000, 0.8660254037844387076, 1.000000000000000000, 0.8660254037844387076, 1.000000000000000000, 0.8660254037844387076, 1.000000000000000000, 0.8660254037844387076, 1.000000000000000000, 0.8660254037844387076, 1.000000000000000000, 0.8660254037844387076, 1.000000000000000000, 0.8660254037844387076, 1.000000000000000000, 0.8660254037844387076, 1.000000000000000000, 0.8660254037844387076, 1.000000000000000000, 0.8660254037844387076, 1.000000000000000000, 0.8660254037844387076, 1.000000000000000000, 0.8660254037844387076, 1.000000000000000000, 0.8660254037844387076, 1.000000000000000000, 0.8660254037844387076, 1.000000000000000000, 0.8660254037844387076, 1.000000000000000000, 0.8660254037844387076, 1.000000000000000000, 0.8660254037844387076, 1.000000000000000000, 0.8660254037844387076, 1.000000000000000000, 0.8660254037844387076, 1.000000000000000000, 0.8660254037844387076, 1.000000000000000000, 0.8660254037844387076, 1.000000000000000000, 0.8660254037844387076, 1.000000000000000000, 0.8660254037844387076, 1.000000000000000000, 0.8660254037844387076, 1.000000000000000000, 0.8660254037844387076, 1.000000000000000000, 0.8660254037844387076, 1.000000000000000000, 0.8660254037844387076, 1.000000000000000000, 0.8660254037844387076, 1.000000000000000000, 0.8660254037844387076, 1.000000000000000000, 0.8660254037844387076, 1.000000000000000000, 0.8660254037844387076, 1.000000000000000000, 0.8660254037844387076, 1.000000000000000000, 0.8660254037844387076, 1.000000000000000000, 0.8660254037844387076, 1.000000000000000000, 0.8660254037844387076, 1.000000000000000000, 0.8660254037844387076, 1.000000000000000000, 0.8660254037844387076, 1.000000000000000000, 0.8660254037844387076, 1.000000000000000000, 0.8660254037844387076, 1.000000000000000000, 0.8660254037844387076, 1.000000000000000000, 0.8660254037844387076, 1.000000000000000000, 0.8660254037844387076, 1.000000000000000000, 0.8660254037844387076, 1.000000000000000000, 0.8660254037844387076, 1.000000000000000000, 0.8660254037844387076, 1.000000000000000000, 0.8660254037844387076, 1.000000000000000000, 0.8660254037844387076, 1.000000000000000000, 0.8660254037844387076, 1.000000000000000000, 0.8660254037844387076, 1.000000000000000000, 0.8660254037844387076, 1.000000000000000000, 0.8660254037844387076, 1.000000000000000000, 0.8660254037844387076, 1.000000000000000000, 0.8660254037844387076, 1.000000000000000000, 0.8660254037844387076, 1.000000000000000000, 0.8660254037844387076, 1.000000000000000000, 0.8660254037844387076, 1.000000000000000000, 0.8660254037844387076, 1.000000000000000000, 0.8660254037844387076, 1.000000000000000000, 0.8660254037844387076, 1.000000000000000000, 0.8660254037844387076, 1.000000000000000000, 0.8660254037844387076, 1.000000000000000000, 0.8660254037844387076, 1.000000000000000000, 0.8660254037844387076, 1.000000000000000000, 0.8660254037844387076, 1.000000000000000000, 0.8660254037844387076, 1.000000000000000000, 0.8660254037844387076, 1.000000000000000000, 0.8660254037844387076, 1.000000000000000000, 0.8660254037844387076, 1.000000000000000000, 0.8660254037844387076, 1.000000000000000000, 0.8660254037844387076, 1.000000000000000000, 0.8660254037844387076, 1.000000000000000000, 0.8660254037844387076, 1.000000000000000000, 0.8660254037844387076, 1.000000000000000000, 0.8660254037844387076, 1.000000000000000000, 0.8660254037844387076, 1.000000000000000000, 0.8660254037844387076, 1.000000000000000000, 0.8660254037844387076, 1.000000000000000000, 0.8660254037844387076, 1.000000000000000000, 0.8660254037844387076, 1.000000000000000000, 0.8660254037844387076, 1.000000000000000000, 0.8660254037844387076, 1.000000000000000000, 0.8660254037844387076, 1.000000000000000000, 0.8660254037844387076, 1.000000000000000000, 0.8660254037844387076, 1.000000000000000000, 0.8660254037844387076, 1.000000000000000000, 0.8660254037844387076, 1.000000000000000000, 0.8660254037844387076, 1.000000000000000000, 0.8660254037844387076, 1.000000000000000000, 0.8660254037844387076, 1.000000000000000000, 0.8660254037844387076, 1.000000000000000000, 0.8660254037844387076, 1.000000000000000000, 0.8660254037844387076, 1.000000000000000000, 0.8660254037844387076, 1.000000000000000000, 0.8660254037844387076, 1.000000000000000000, 0.8660254037844387076, 1.000000000000000000, 0.8660254037844387076, 1.000000000000000000, 0.8660254037844387076, 1.000000000000000000, 0.8660254037844387076, 1.000000000000000000, 0.8660254037844387076, 1.000000000000000000, 0.8660254037844387076, 1.000000000000000000, 0.8660254037844387076, 1.000000000000000000, 0.8660254037844387076, 1.000000000000000000, 0.8660254037844387076, 1.000000000000000000, 0.8660254037844387076, 1.000000000000000000, 0.8660254037844387076, 1.000000000000000000, 0.8660254037844387076, 1.000000000000000000, 0.8660254037844387076, 1.000000000000000000, 0.8660254037844387076, 1.000000000000000000, 0.8660254037844387076, 1.000000000000000000, 0.8660254037844387076, 1.000000000000000000, 0.8660254037844387076, 1.000000000000000000, 0.8660254037844387076, 1.000000000000000000, 0.8660254037844387076, 1.000000000000000000, 0.8660254037844387076, 1.000000000000000000, 0.8660254037844387076, 1.000000000000000000, 0.8660254037844387076, 1.000000000000000000, 0.8660254037844387076, 1.000000000000000000, 0.8660254037844387076, 1.000000000000000000, 0.8660254037844387076, 1.000000000000000000, 0.8660254037844387076, 1.000000000000000000, 0.8660254037844387076, 1.000000000000000000, 0.8660254037844387076, 1.000000000000000000, 0.8660254037844387076, 1.000000000000000000, 0.8660254037844387076, 1.000000000000000000, 0.8660254037844387076, 1.000000000000000000, 0.8660254037844387076, 1.000000000000000000, 0.8660254037844387076, 1.000000000000000000, 0.8660254037844387076, 1.000000000000000000, 0.8660254037844387076, 1.000000000000000000, 0.8660254037844387076, 1.000000000000000000, 0.8660254037844387076, 1.000000000000000000, 0.8660254037844387076, 1.000000000000000000, 0.8660254037844387076, 1.000000000000000000, 0.8660254037844387076, 1.000000000000000000, 0.8660254037844387076, 1.000000000000000000, 0.8660254037844387076, 1.000000000000000000, 0.8660254037844387076, 1.000000000000000000, 0.8660254037844387076, 1.000000000000000000, 0.8660254037844387076, 1.000000000000000000, 0.8660254037844387076, 1.000000000000000000, 0.8660254037844387076, 1.000000000000000000, 0.8660254037844387076, 1.000000000000000000, 0.8660254037844387076, 1.000000000000000000, 0.8660254037844387076, 1.000000000000000000, 0.8660254037844387076, 1.000000000000000000, 0.8660254037844387076, 1.000000000000000000, 0.8660254037844387076, 1.000000000000000000, 0.8660254037844387076, 1.000000000000000000, 0.8660254037844387076, 1.000000000000000000, 0.8660254037844387076, 1.000000000000000000, 0.8660254037844387076, 1.000000000000000000, 0.8660254037844387076, 1.000000000000000000, 0.8660254037844387076, 1.000000000000000000, 0.8660254037844387076, 1.000000000000000000, 0.8660254037844387076, 1.000000000000000000, 0.8660254037844387076, 1.000000000000000000, 0.8660254037844387076, 1.000000000000000000, 0.8660254037844387076, 1.000000000000000000, 0.8660254037844387076, 1.000000000000000000, 0.8660254037844387076, 1.000000000000000000, 0.8660254037844387076, 1.000000000000000000, 0.8660254037844387076, 1.000000000000000000),
 ( 1.000000000000000000, 0.8660254037844387076, 1.000000000000000000, 0.8660254037844387076, 1.000000000000000000, 0.8660254037844387076, 1.000000000000000000, 0.8660254037844387076, 1.000000000000000000, 0.8660254037844387076, 1.000000000000000000, 0.8660254037844387076, 1.000000000000000000, 0.8660254037844387076, 1.000000000000000000, 0.8660254037844387076, 1.000000000000000000, 0.8660254037844387076, 1.000000000000000000, 0.8660254037844387076, 1.000000000000000000, 0.8660254037844387076, 1.000000000000000000, 0.8660254037844387076, 1.000000000000000000, 0.8660254037844387076, 1.000000000000000000, 0.8660254037844387076, 1.000000000000000000, 0.8660254037844387076, 1.000000000000000000, 0.8660254037844387076, 1.000000000000000000, 0.8660254037844387076, 1.000000000000000000, 0.8660254037844387076, 1.000000000000000000, 0.8660254037844387076, 1.000000000000000000, 0.8660254037844387076, 1.000000000000000000, 0.8660254037844387076, 1.000000000000000000, 0.8660254037844387076, 1.000000000000000000, 0.8660254037844387076, 1.000000000000000000, 0.8660254037844387076, 1.000000000000000000, 0.8660254037844387076, 1.000000000000000000, 0.8660254037844387076, 1.000000000000000000, 0.8660254037844387076, 1.000000000000000000, 0.8660254037844387076, 1.000000000000000000, 0.8660254037844387076, 1.000000000000000000, 0.8660254037844387076, 1.000000000000000000, 0.8660254037844387076, 1.000000000000000000, 0.8660254037844387076, 1.000000000000000000, 0.8660254037844387076, 1.000000000000000000, 0.8660254037844387076, 1.000000000000000000, 0.8660254037844387076, 1.000000000000000000, 0.8660254037844387076, 1.000000000000000000, 0.8660254037844387076, 1.000000000000000000, 0.8660254037844387076, 1.000000000000000000, 0.8660254037844387076, 1.000000000000000000, 0.8660254037844387076, 1.000000000000000000, 0.8660254037844387076, 1.000000000000000000, 0.8660254037844387076, 1.000000000000000000, 0.8660254037844387076, 1.000000000000000000, 0.8660254037844387076, 1.000000000000000000, 0.8660254037844387076, 1.000000000000000000, 0.8660254037844387076, 1.000000000000000000, 0.8660254037844387076, 1.000000000000000000, 0.8660254037844387076, 1.000000000000000000, 0.8660254037844387076, 1.000000000000000000, 0.8660254037844387076, 1.000000000000000000, 0.8660254037844387076, 1.000000000000000000, 0.8660254037844387076, 1.000000000000000000, 0.8660254037844387076, 1.000000000000000000, 0.8660254037844387076, 1.000000000000000000, 0.8660254037844387076, 1.000000000000000000, 0.8660254037844387076, 1.000000000000000000, 0.8660254037844387076, 1.000000000000000000, 0.8660254037844387076, 1.000000000000000000, 0.8660254037844387076, 1.000000000000000000, 0.8660254037844387076, 1.000000000000000000, 0.8660254037844387076, 1.000000000000000000, 0.8660254037844387076, 1.000000000000000000, 0.8660254037844387076, 1.000000000000000000, 0.8660254037844387076, 1.000000000000000000, 0.8660254037844387076, 1.000000000000000000, 0.8660254037844387076, 1.000000000000000000, 0.8660254037844387076, 1.000000000000000000, 0.8660254037844387076, 1.000000000000000000, 0.8660254037844387076, 1.000000000000000000, 0.8660254037844387076, 1.000000000000000000, 0.8660254037844387076, 1.000000000000000000, 0.8660254037844387076, 1.000000000000000000, 0.8660254037844387076, 1.000000000000000000, 0.8660254037844387076, 1.000000000000000000, 0.8660254037844387076, 1.000000000000000000, 0.8660254037844387076, 1.000000000000000000, 0.8660254037844387076, 1.000000000000000000, 0.8660254037844387076, 1.000000000000000000, 0.8660254037844387076, 1.000000000000000000, 0.8660254037844387076, 1.000000000000000000, 0.8660254037844387076, 1.000000000000000000, 0.8660254037844387076, 1.000000000000000000, 0.8660254037844387076, 1.000000000000000000, 0.8660254037844387076, 1.000000000000000000, 0.8660254037844387076, 1.000000000000000000, 0.8660254037844387076, 1.000000000000000000, 0.8660254037844387076, 1.000000000000000000, 0.8660254037844387076, 1.000000000000000000, 0.8660254037844387076, 1.000000000000000000, 0.8660254037844387076, 1.000000000000000000, 0.8660254037844387076, 1.000000000000000000, 0.8660254037844387076, 1.000000000000000000, 0.8660254037844387076, 1.000000000000000000, 0.8660254037844387076, 1.000000000000000000, 0.8660254037844387076, 1.000000000000000000, 0.8660254037844387076, 1.000000000000000000, 0.8660254037844387076, 1.000000000000000000, 0.8660254037844387076, 1.000000000000000000, 0.8660254037844387076, 1.000000000000000000, 0.8660254037844387076, 1.000000000000000000, 0.8660254037844387076, 1.000000000000000000, 0.8660254037844387076, 1.000000000000000000, 0.8660254037844387076, 1.000000000000000000, 0.8660254037844387076, 1.000000000000000000, 0.8660254037844387076, 1.000000000000000000, 0.8660254037844387076, 1.000000000000000000, 0.8660254037844387076, 1.000000000000000000, 0.8660254037844387076, 1.000000000000000000, 0.8660254037844387076, 1.000000000000000000, 0.8660254037844387076, 1.000000000000000000, 0.8660254037844387076, 1.000000000000000000, 0.8660254037844387076, 1.000000000000000000, 0.8660254037844387076, 1.000000000000000000, 0.8660254037844387076, 1.000000000000000000, 0.8660254037844387076, 1.000000000000000000, 0.8660254037844387076, 1.000000000000000000, 0.8660254037844387076, 1.000000000000000000, 0.8660254037844387076, 1.000000000000000000, 0.8660254037844387076, 1.000000000000000000, 0.8660254037844387076, 1.000000000000000000, 0.8660254037844387076, 1.000000000000000000, 0.8660254037844387076, 1.000000000000000000, 0.8660254037844387076, 1.000000000000000000, 0.8660254037844387076, 1.000000000000000000, 0.8660254037844387076, 1.000000000000000000, 0.8660254037844387076, 1.000000000000000000, 0.8660254037844387076, 1.000000000000000000, 0.8660254037844387076, 1.000000000000000000, 0.8660254037844387076, 1.000000000000000000, 0.8660254037844387076, 1.000000000000000000, 0.8660254037844387076, 1.000000000000000000, 0.8660254037844387076, 1.000000000000000000, 0.8660254037844387076, 1.000000000000000000, 0.8660254037844387076, 1.000000000000000000, 0.8660254037844387076, 1.000000000000000000, 0.8660254037844387076, 1.000000000000000000, 0.8660254037844387076, 1.000000000000000000, 0.8660254037844387076, 1.000000000000000000, 0.8660254037844387076, 1.000000000000000000, 0.8660254037844387076, 1.000000000000000000, 0.8660254037844387076, 1.000000000000000000, 0.8660254037844387076, 1.000000000000000000, 0.8660254037844387076, 1.000000000000000000, 0.8660254037844387076, 1.000000000000000000, 0.8660254037844387076, 1.000000000000000000, 0.8660254037844387076, 1.000000000000000000, 0.8660254037844387076, 1.000000000000000000, 0.8660254037844387076, 1.000000000000000000, 0.8660254037844387076, 1.000000000000000000, 0.8660254037844387076, 1.000000000000000000, 0.8660254037844387076, 1.000000000000000000, 0.8660254037844387076, 1.000000000000000000, 0.8660254037844387076, 1.000000000000000000, 0.8660254037844387076, 1.000000000000000000, 0.8660254037844387076, 1.000000000000000000, 0.8660254037844387076, 1.000000000000000000, 0.8660254037844387076, 1.000000000000000000, 0.8660254037844387076, 1.000000000000000000, 0.8660254037844387076, 1.000000000000000000, 0.8660254037844387076, 1.000000000000000000, 0.8660254037844387076, 1.000000000000000000, 0.8660254037844387076, 1.000000000000000000, 0.8660254037844387076, 1.000000000000000000, 0.8660254037844387076, 1.000000000000000000, 0.8660254037844387076, 1.000000000000000000, 0.8660254037844387076, 1.000000000000000000, 0.8660254037844387076, 1.000000000000000000, 0.8660254037844387076, 1.000000000000000000, 0.8660254037844387076, 1.000000000000000000, 0.8660254037844387076, 1.000000000000000000, 0.8660254037844387076, 1.000000000000000000, 0.8660254037844387076, 1.000000000000000000, 0.8660254037844387076, 1.000000000000000000, 0.8660254037844387076, 1.000000000000000000, 0.8660254037844387076, 1.000000000000000000, 0.8660254037844387076, 1.000000000000000000, 0.8660254037844387076, 1.000000000000000000, 0.8660254037844387076, 1.000000000000000000, 0.8660254037844387076, 1.000000000000000000, 0.8660254037844387076, 1.000000000000000000, 0.8660254037844387076, 1.000000000000000000, 0.8660254037844387076, 1.000000000000000000, 0.8660254037844387076, 1.000000000000000000, 0.8660254037844387076, 1.000000000000000000, 0.8660254037844387076, 1.000000000000000000, 0.8660254037844387076, 1.000000000000000000, 0.8660254037844387076, 1.000000000000000000, 0.8660254037844387076, 1.000000000000000000, 0.8660254037844387076, 1.000000000000000000, 0.8660254037844387076, 1.000000000000000000, 0.8660254037844387076, 1.000000000000000000, 0.8660254037844387076, 1.000000000000000000, 0.8660254037844387076, 1.000000000000000000, 0.8660254037844387076, 1.000000000000000000, 0.8660254037844387076, 1.000000000000000000, 0.8660254037844387076, 1.000000000000000000, 0.8660254037844387076, 1.000000000000000000, 0.8660254037844387076, 1.000000000000000000, 0.8660254037844387076, 1.000000000000000000, 0.8660254037844387076, 1.000000000000000000, 0.8660254037844387076, 1.000000000000000000, 0.8660254037844387076, 1.000000000000000000, 0.8660254037844387076, 1.000000000000000000, 0.8660254037844387076, 1.000000000000000000, 0.8660254037844387076, 1.000000000000000000, 0.8660254037844387076, 1.000000000000000000, 0.8660254037844387076, 1.000000000000000000, 0.8660254037844387076, 1.000000000000000000, 0.8660254037844387076, 1.000000000000000000, 0.8660254037844387076, 1.000000000000000000, 0.8660254037844387076, 1.000000000000000000, 0.8660254037844387076, 1.000000000000000000, 0.8660254037844387076, 1.000000000000000000, 0.8660254037844387076, 1.000000000000000000, 0.8660254037844387076, 1.000000000000000000, 0.8660254037844387076, 1.000000000000000000, 0.8660254037844387076, 1.000000000000000000, 0.8660254037844387076, 1.000000000000000000, 0.8660254037844387076, 1.000000000000000000, 0.8660254037844387076, 1.000000000000000000, 0.8660254037844387076, 1.000000000000000000, 0.8660254037844387076, 1.000000000000000000, 0.8660254037844387076, 1.000000000000000000, 0.8660254037844387076, 1.000000000000000000, 0.8660254037844387076, 1.000000000000000000, 0.8660254037844387076, 1.000000000000000000, 0.8660254037844387076, 1.000000000000000000, 0.8660254037844387076, 1.000000000000000000, 0.8660254037844387076, 1.000000000000000000, 0.8660254037844387076, 1.000000000000000000, 0.8660254037844387076, 1.000000000000000000, 0.8660254037844387076, 1.000000000000000000, 0.8660254037844387076, 1.000000000000000000, 0.8660254037844387076, 1.000000000000000000, 0.8660254037844387076, 1.000000000000000000, 0.8660254037844387076, 1.000000000000000000, 0.8660254037844387076, 1.000000000000000000, 0.8660254037844387076, 1.000000000000000000, 0.8660254037844387076, 1.000000000000000000, 0.8660254037844387076, 1.000000000000000000, 0.8660254037844387076, 1.000000000000000000, 0.8660254037844387076, 1.000000000000000000, 0.8660254037844387076, 1.000000000000000000, 0.8660254037844387076, 1.000000000000000000, 0.8660254037844387076, 1.000000000000000000, 0.8660254037844387076, 1.000000000000000000, 0.8660254037844387076, 1.000000000000000000, 0.8660254037844387076, 1.000000000000000000, 0.8660254037844387076, 1.000000000000000000, 0.8660254037844387076, 1.000000000000000000, 0.8660254037844387076, 1.000000000000000000, 0.8660254037844387076, 1.000000000000000000, 0.8660254037844387076, 1.000000000000000000, 0.8660254037844387076, 1.000000000000000000, 0.8660254037844387076, 1.000000000000000000, 0.8660254037844387076, 1.000000000000000000, 0.8660254037844387076, 1.000000000000000000, 0.8660254037844387076, 1.000000000000000000, 0.8660254037844387076, 1.000000000000000000, 0.8660254037844387076, 1.000000000000000000, 0.8660254037844387076, 1.000000000000000000, 0.8660254037844387076, 1.000000000000000000, 0.8660254037844387076, 1.000000000000000000, 0.8660254037844387076, 1.000000000000000000, 0.8660254037844387076, 1.000000000000000000, 0.8660254037844387076, 1.000000000000000000, 0.8660254037844387076, 1.000000000000000000, 0.8660254037844387076, 1.000000000000000000, 0.8660254037844387076, 1.000000000000000000, 0.8660254037844387076, 1.000000000000000000, 0.8660254037844387076, 1.000000000000000000, 0.8660254037844387076, 1.000000000000000000, 0.8660254037844387076, 1.000000000000000000, 0.8660254037844387076, 1.000000000000000000, 0.8660254037844387076, 1.000000000000000000, 0.8660254037844387076, 1.000000000000000000, 0.8660254037844387076, 1.000000000000000000, 0.8660254037844387076, 1.000000000000000000, 0.8660254037844387076, 1.000000000000000000, 0.8660254037844387076, 1.000000000000000000, 0.8660254037844387076, 1.000000000000000000, 0.8660254037844387076, 1.000000000000000000, 0.8660254037844387076, 1.000000000000000000, 0.8660254037844387076, 1.000000000000000000, 0.8660254037844387076, 1.000000000000000000, 0.8660254037844387076, 1.000000000000000000, 0.8660254037844387076, 1.000000000000000000, 0.8660254037844387076, 1.000000000000000000, 0.8660254037844387076, 1.000000000000000000, 0.8660254037844387076, 1.000000000000000000, 0.8660254037844387076, 1.000000000000000000, 0.8660254037844387076, 1.000000000000000000, 0.8660254037844387076, 1.000000000000000000, 0.8660254037844387076, 1.000000000000000000, 0.8660254037844387076, 1.000000000000000000, 0.8660254037844387076, 1.000000000000000000, 0.8660254037844387076, 1.000000000000000000, 0.8660254037844387076, 1.000000000000000000, 0.8660254037844387076, 1.000000000000000000, 0.8660254037844387076, 1.000000000000000000, 0.8660254037844387076, 1.000000000000000000, 0.8660254037844387076, 1.000000000000000000, 0.8660254037844387076, 1.000000000000000000, 0.8660254037844387076, 1.000000000000000000, 0.8660254037844387076, 1.000000000000000000, 0.8660254037844387076, 1.000000000000000000, 0.8660254037844387076, 1.000000000000000000, 0.8660254037844387076, 1.000000000000000000, 0.8660254037844387076, 1.000000000000000000, 0.8660254037844387076, 1.000000000000000000, 0.8660254037844387076, 1.000000000000000000, 0.8660254037844387076, 1.000000000000000000, 0.8660254037844387076, 1.000000000000000000, 0.8660254037844387076, 1.000000000000000000, 0.8660254037844387076, 1.000000000000000000, 0.8660254037844387076, 1.000000000000000000, 0.8660254037844387076, 1.000000000000000000, 0.8660254037844387076, 1.000000000000000000, 0.8660254037844387076, 1.000000000000000000, 0.8660254037844387076, 1.000000000000000000, 0.8660254037844387076, 1.000000000000000000, 0.8660254037844387076, 1.000000000000000000, 0.8660254037844387076, 1.000000000000000000, 0.8660254037844387076, 1.000000000000000000, 0.8660254037844387076, 1.000000000000000000, 0.8660254037844387076, 1.000000000000000000, 0.8660254037844387076, 1.000000000000000000, 0.8660254037844387076, 1.000000000000000000, 0.8660254037844387076, 1.000000000000000000, 0.8660254037844387076, 1.000000000000000000, 0.8660254037844387076, 1.000000000000000000, 0.8660254037844387076, 1.000000000000000000, 0.8660254037844387076, 1.000000000000000000, 0.8660254037844387076, 1.000000000000000000, 0.8660254037844387076, 1.000000000000000000, 0.8660254037844387076, 1.000000000000000000, 0.8660254037844387076, 1.000000000000000000, 0.8660254037844387076, 1.000000000000000000, 0.8660254037844387076, 1.000000000000000000, 0.8660254037844387076, 1.000000000000000000, 0.8660254037844387076, 1.000000000000000000, 0.8660254037844387076, 1.000000000000000000, 0.8660254037844387076, 1.000000000000000000, 0.8660254037844387076, 1.000000000000000000, 0.8660254037844387076, 1.000000000000000000, 0.8660254037844387076, 1.000000000000000000, 0.8660254037844387076, 1.000000000000000000, 0.8660254037844387076, 1.000000000000000000, 0.8660254037844387076, 1.000000000000000000, 0.8660254037844387076, 1.000000000000000000, 0.8660254037844387076, 1.000000000000000000, 0.8660254037844387076, 1.000000000000000000, 0.8660254037844387076, 1.000000000000000000, 0.8660254037844387076, 1.000000000000000000, 0.8660254037844387076, 1.000000000000000000, 0.8660254037844387076, 1.000000000000000000, 0.8660254037844387076, 1.000000000000000000, 0.8660254037844387076, 1.000000000000000000, 0.8660254037844387076, 1.000000000000000000, 0.8660254037844387076, 1.000000000000000000) ) ) 
 REPRESENTATION_ITEM ( '' )  SURFACE ( )  );
#15854 = ORIENTED_EDGE ( 'NONE', *, *, #41629, .T. ) ;
#15855 = CARTESIAN_POINT ( 'NONE',  ( 24.10312500061451502, -4.541064518000417216, -2.621784821875001281 ) ) ;
#15856 = CARTESIAN_POINT ( 'NONE',  ( 1.626862140677534470E-15, 13.23124999877096819, 34.00000000000000000 ) ) ;
#15857 = CARTESIAN_POINT ( 'NONE',  ( 11.10937500061451644, -4.119189519843965641, -2.378215178125001383 ) ) ;
#15858 = CARTESIAN_POINT ( 'NONE',  ( -3.999999999999999112, 11.11250000122903536, 30.00000000000000000 ) ) ;
#15859 = CARTESIAN_POINT ( 'NONE',  ( -3.999999999999999556, 13.32500000122903572, -32.30940107675850470 ) ) ;
#15860 = EDGE_CURVE ( 'NONE', #14728, #69731, #25895, .T. ) ;
#15861 = CARTESIAN_POINT ( 'NONE',  ( 4.243569643749999010, 18.77187500061451786, -32.45002607614398471 ) ) ;
#15862 = CARTESIAN_POINT ( 'NONE',  ( 10.95000000000000107, 4.330127018922192761, -2.499999999999997780 ) ) ;
#15863 = CARTESIAN_POINT ( 'NONE',  ( 11.78437500061451892, 4.541064518000418104, 2.621784821874999949 ) ) ;
#15864 = CARTESIAN_POINT ( 'NONE',  ( 6.712500001229034119, 0.000000000000000000, 4.999999999999998224 ) ) ;
#15865 = CARTESIAN_POINT ( 'NONE',  ( 14.48437500061451821, 4.541064518000418104, 2.621784821874999949 ) ) ;
#15866 = CARTESIAN_POINT ( 'NONE',  ( 5.034375000614519813, 4.541064518000418104, 2.621784821874999949 ) ) ;
#15867 = DIRECTION ( 'NONE',  ( -1.000000000000000000, -0.000000000000000000, -0.000000000000000000 ) ) ;
#15868 = AXIS2_PLACEMENT_3D ( 'NONE', #16774, #6789, #16412 ) ;
#15869 = DIRECTION ( 'NONE',  ( -0.000000000000000000, -0.000000000000000000, -1.000000000000000000 ) ) ;
#15870 = CARTESIAN_POINT ( 'NONE',  ( 9.834375000614517859, 6.421520780324663323E-16, -5.243569643749999010 ) ) ;
#15871 = LINE ( 'NONE', #55413, #11150 ) ;
#15872 = CARTESIAN_POINT ( 'NONE',  ( 18.77812500061451573, 6.421520780324663323E-16, -5.243569643749999010 ) ) ;
#15873 = ADVANCED_FACE ( 'NONE', ( #26261 ), #47363, .T. ) ;
#15874 = DIRECTION ( 'NONE',  ( 0.000000000000000000, 0.000000000000000000, -1.000000000000000000 ) ) ;
#15875 = CARTESIAN_POINT ( 'NONE',  ( 10.00000000000000000, 1.224646799147353256E-15, -10.00000000000000888 ) ) ;
#15876 = CARTESIAN_POINT ( 'NONE',  ( 24.19687500061451857, -3.027376345333610441, -5.243569643749999898 ) ) ;
#15877 = CARTESIAN_POINT ( 'NONE',  ( 4.391019444462268773, 2.392760695475801835, 4.391019444462268773 ) ) ;
#15878 = EDGE_CURVE ( 'NONE', #68160, #47688, #54927, .T. ) ;
#15879 = CARTESIAN_POINT ( 'NONE',  ( 29.21250000122903145, 0.000000000000000000, 4.999999999999998224 ) ) ;
#15880 = CARTESIAN_POINT ( 'NONE',  ( 20.44687500061451502, -4.119189519843965641, -2.378215178125001383 ) ) ;
#15881 = CARTESIAN_POINT ( 'NONE',  ( 25.67812500061451431, 4.541064518000418104, 2.621784821874999949 ) ) ;
#15882 = CARTESIAN_POINT ( 'NONE',  ( 18.55312500061451431, 0.000000000000000000, 5.243569643749999010 ) ) ;
#15883 = CARTESIAN_POINT ( 'NONE',  ( 13.59375000122903288, -2.886751345948125991, -5.000000000000000000 ) ) ;
#15884 = CARTESIAN_POINT ( 'NONE',  ( 14.29687500061451821, -3.027376345333610441, -5.243569643749999898 ) ) ;
#15885 = CARTESIAN_POINT ( 'NONE',  ( 26.28750000122903430, 6.123233995736764310E-16, -4.999999999999998224 ) ) ;
#15886 = CARTESIAN_POINT ( 'NONE',  ( 26.73750000122903003, 6.123233995736764310E-16, -4.999999999999998224 ) ) ;
#15887 = CARTESIAN_POINT ( 'NONE',  ( 13.88437500061451679, 6.421520780324663323E-16, -5.243569643749999010 ) ) ;
#15888 = DIRECTION ( 'NONE',  ( 0.000000000000000000, 0.000000000000000000, -1.000000000000000000 ) ) ;
#15889 = CARTESIAN_POINT ( 'NONE',  ( 30.00000000000000000, 6.123233995736764310E-16, -4.999999999999998224 ) ) ;
#15890 = CARTESIAN_POINT ( 'NONE',  ( 4.275000001229035895, 2.886751345948129099, -4.999999999999998224 ) ) ;
#15891 = CARTESIAN_POINT ( 'NONE',  ( 25.20937500061451431, 4.541064518000418104, -2.621784821874998173 ) ) ;
#15892 = CARTESIAN_POINT ( 'NONE',  ( 16.43437500061451573, -4.541064518000419881, 2.621784821874995952 ) ) ;
#15893 = CARTESIAN_POINT ( 'NONE',  ( -1.878215178124999163, 16.95312499938548356, 26.74683588394047007 ) ) ;
#15894 = CARTESIAN_POINT ( 'NONE',  ( 27.78749999999999787, -2.886751345948129988, 4.999999999999997335 ) ) ;
#15895 = CARTESIAN_POINT ( 'NONE',  ( 5.737499999999998934, -2.886751345948129988, 4.999999999999997335 ) ) ;
#15896 = CARTESIAN_POINT ( 'NONE',  ( 28.47187500061451715, 2.746126346562643317, 4.756430356249998326 ) ) ;
#15897 = CARTESIAN_POINT ( 'NONE',  ( 20.16562500061451146, 3.027376345333613106, -5.243569643749998122 ) ) ;
#15898 = CARTESIAN_POINT ( 'NONE',  ( 9.262499999999999289, 2.886751345948126879, 4.999999999999999112 ) ) ;
#15899 = CARTESIAN_POINT ( 'NONE',  ( 4.115625000614516082, 3.027376345333611329, 5.243569643749999010 ) ) ;
#15900 = CARTESIAN_POINT ( 'NONE',  ( 19.27500000000000213, -4.330127018922194537, 2.499999999999995559 ) ) ;
#15901 = FACE_OUTER_BOUND ( 'NONE', #49932, .T. ) ;
#15902 = CARTESIAN_POINT ( 'NONE',  ( 23.92500000122903359, -5.773502691896255534, -1.060575238724906372E-15 ) ) ;
#15903 = CARTESIAN_POINT ( 'NONE',  ( 5.375648687660714131, 8.434199909737650103, 32.69359484207353717 ) ) ;
#15904 = CARTESIAN_POINT ( 'NONE',  ( 3.300000000000000711, 4.330127018922192761, -2.499999999999997780 ) ) ;
#15905 = ORIENTED_EDGE ( 'NONE', *, *, #23424, .F. ) ;
#15906 = CARTESIAN_POINT ( 'NONE',  ( 17.80312500061451786, -4.541064518000417216, -2.621784821875001281 ) ) ;
#15907 = CARTESIAN_POINT ( 'NONE',  ( 25.19062500061451715, 6.054752690667223547, 3.707466751127219781E-16 ) ) ;
#15908 = CARTESIAN_POINT ( 'NONE',  ( 22.69687500061451857, -3.027376345333614438, 5.243569643749998122 ) ) ;
#15909 = CARTESIAN_POINT ( 'NONE',  ( 7.425000000000000711, 4.330127018922191873, 2.499999999999999556 ) ) ;
#15910 = CARTESIAN_POINT ( 'NONE',  ( 8.578125000614518214, 4.541064518000418104, 2.621784821874999949 ) ) ;
#15911 = CARTESIAN_POINT ( 'NONE',  ( 25.49062500061451786, -3.027376345333610441, -5.243569643749999898 ) ) ;
#15912 = CARTESIAN_POINT ( 'NONE',  ( 15.64687500061451608, -3.027376345333610441, -5.243569643749999898 ) ) ;
#15913 = CARTESIAN_POINT ( 'NONE',  ( 19.65937500061451360, -4.541064518000417216, -2.621784821875001281 ) ) ;
#15914 = CARTESIAN_POINT ( 'NONE',  ( 1.999999999999998668, 11.86250000122903359, -33.46410161513775705 ) ) ;
#15915 = CARTESIAN_POINT ( 'NONE',  ( -4.243569643749999898, 19.31562500061451715, 27.54997392385601529 ) ) ;
#15916 = CARTESIAN_POINT ( 'NONE',  ( 21.07500000122903572, 2.886751345948126879, 4.999999999999999112 ) ) ;
#15917 = CARTESIAN_POINT ( 'NONE',  ( 17.74687500061451928, -2.746126346562646425, 4.756430356249996549 ) ) ;
#15918 = CARTESIAN_POINT ( 'NONE',  ( 10.94062500061451537, -3.027376345333614438, 5.243569643749998122 ) ) ;
#15919 = CARTESIAN_POINT ( 'NONE',  ( 8.371875000614515727, -6.054752690667223547, -1.112240025338166033E-15 ) ) ;
#15920 = CARTESIAN_POINT ( 'NONE',  ( 7.546875000614517326, -3.027376345333610441, -5.243569643749999898 ) ) ;
#15921 = ORIENTED_EDGE ( 'NONE', *, *, #32136, .T. ) ;
#15922 = CARTESIAN_POINT ( 'NONE',  ( 27.72187500061451715, -6.054752690667223547, -1.112240025338166033E-15 ) ) ;
#15923 = CARTESIAN_POINT ( 'NONE',  ( 18.59062500061451573, -3.027376345333614438, 5.243569643749998122 ) ) ;
#15924 = CARTESIAN_POINT ( 'NONE',  ( 3.065625000614517592, 3.027376345333613106, -5.243569643749998122 ) ) ;
#15925 = CARTESIAN_POINT ( 'NONE',  ( 29.12812500061451715, 6.421520780324663323E-16, -5.243569643749999010 ) ) ;
#15926 = CARTESIAN_POINT ( 'NONE',  ( 23.33437500061451786, 6.421520780324663323E-16, -5.243569643749999010 ) ) ;
#15927 = CARTESIAN_POINT ( 'NONE',  ( 19.30312500061451786, 4.541064518000418104, -2.621784821874998173 ) ) ;
#15928 = CARTESIAN_POINT ( 'NONE',  ( -3.999999999999999556, 10.96250000000000213, 27.69059892324149530 ) ) ;
#15929 = VECTOR ( 'NONE', #38365, 1000.000000000000000 ) ;
#15930 = CARTESIAN_POINT ( 'NONE',  ( 23.76562500061451644, 3.027376345333613106, -5.243569643749998122 ) ) ;
#15931 = CARTESIAN_POINT ( 'NONE',  ( 5.400000001229032343, -2.886751345948129988, 4.999999999999997335 ) ) ;
#15932 = ORIENTED_EDGE ( 'NONE', *, *, #18629, .T. ) ;
#15933 = CARTESIAN_POINT ( 'NONE',  ( 10.00000000000000000, 1.224646799147353256E-15, 50.00000000000000000 ) ) ;
#15934 = CARTESIAN_POINT ( 'NONE',  ( 2.000000000000001332, 15.20000000000000107, -26.53589838486224650 ) ) ;
#15935 = CARTESIAN_POINT ( 'NONE',  ( -1.878215178125001827, 15.30312499938548321, 33.25316411605952283 ) ) ;
#15936 = CARTESIAN_POINT ( 'NONE',  ( 4.321875000614517681, -6.054752690667223547, -1.112240025338166033E-15 ) ) ;
#15937 = CARTESIAN_POINT ( 'NONE',  ( 34.99999999999999289, -2.499999999999999556, 3.499999999999999556 ) ) ;
#15938 = CARTESIAN_POINT ( 'NONE',  ( 12.06562500061451537, 3.027376345333613106, -5.243569643749998122 ) ) ;
#15939 = CARTESIAN_POINT ( 'NONE',  ( 5.521875000614517859, 3.027376345333611329, 5.243569643749999010 ) ) ;
#15940 = CARTESIAN_POINT ( 'NONE',  ( 23.85000000122903430, -2.886751345948129988, 4.999999999999997335 ) ) ;
#15941 = AXIS2_PLACEMENT_3D ( 'NONE', #10181, #72240, #15707 ) ;
#15942 = CARTESIAN_POINT ( 'NONE',  ( 15.57187500061451857, -6.054752690667223547, -1.112240025338166033E-15 ) ) ;
#15943 = CARTESIAN_POINT ( 'NONE',  ( 3.271875000614519635, 3.027376345333611329, 5.243569643749999010 ) ) ;
#15944 = CARTESIAN_POINT ( 'NONE',  ( -2.000000000000000000, 10.92500000000000071, 26.53589838486224650 ) ) ;
#15945 = CARTESIAN_POINT ( 'NONE',  ( 26.59687500061451360, 6.054752690667223547, 3.707466751127219781E-16 ) ) ;
#15946 = CARTESIAN_POINT ( 'NONE',  ( 3.365625000614516082, -6.054752690667223547, -1.112240025338166033E-15 ) ) ;
#15947 = CARTESIAN_POINT ( 'NONE',  ( 12.70312500061451821, 0.000000000000000000, 5.243569643749999010 ) ) ;
#15948 = ORIENTED_EDGE ( 'NONE', *, *, #48843, .T. ) ;
#15949 = CARTESIAN_POINT ( 'NONE',  ( 10.97812500061451679, -4.541064518000419881, 2.621784821874995952 ) ) ;
#15950 = CARTESIAN_POINT ( 'NONE',  ( 7.565625000614518036, 3.027376345333613106, -5.243569643749998122 ) ) ;
#15951 = CARTESIAN_POINT ( 'NONE',  ( 18.38437500061451857, 5.824947211148865298E-16, -4.756430356249998326 ) ) ;
#15952 = CARTESIAN_POINT ( 'NONE',  ( 9.037499999999999645, -2.886751345948125991, -5.000000000000000000 ) ) ;
#15953 = CARTESIAN_POINT ( 'NONE',  ( 3.825000001229032609, 2.886751345948129099, -4.999999999999998224 ) ) ;
#15954 = CARTESIAN_POINT ( 'NONE',  ( 18.97499999999999787, 6.123233995736764310E-16, -4.999999999999998224 ) ) ;
#15955 = CARTESIAN_POINT ( 'NONE',  ( 19.02187500061451786, 3.027376345333611329, 5.243569643749999010 ) ) ;
#15956 = CARTESIAN_POINT ( 'NONE',  ( 13.27500000122903323, 2.886751345948129099, -4.999999999999998224 ) ) ;
#15957 = CARTESIAN_POINT ( 'NONE',  ( 20.88749999999999929, 5.773502691896255534, 3.535250795749688894E-16 ) ) ;
#15958 = CARTESIAN_POINT ( 'NONE',  ( -2.121784821874996840, 15.82812500061451644, -26.32496088578401583 ) ) ;
#15959 = CARTESIAN_POINT ( 'NONE',  ( 22.01249999999999574, -5.773502691896255534, -1.060575238724906372E-15 ) ) ;
#15960 = DIRECTION ( 'NONE',  ( -1.000000000000000000, -0.000000000000000000, -0.000000000000000000 ) ) ;
#15961 = CARTESIAN_POINT ( 'NONE',  ( 28.45312500061451289, 0.000000000000000000, 5.243569643749999010 ) ) ;
#15962 = FILL_AREA_STYLE ('',( #9341 ) ) ;
#15963 = CARTESIAN_POINT ( 'NONE',  ( 24.14999999999999858, 0.000000000000000000, 4.999999999999998224 ) ) ;
#15964 = CARTESIAN_POINT ( 'NONE',  ( 14.44687500061451679, 6.054752690667223547, 3.707466751127219781E-16 ) ) ;
#15965 = CARTESIAN_POINT ( 'NONE',  ( 27.07499999999999929, 6.123233995736764310E-16, -4.999999999999998224 ) ) ;
#15966 = ADVANCED_FACE ( 'NONE', ( #13130 ), #46047, .T. ) ;
#15967 = CARTESIAN_POINT ( 'NONE',  ( 9.365625000614519635, 3.027376345333613106, -5.243569643749998122 ) ) ;
#15968 = CARTESIAN_POINT ( 'NONE',  ( 26.44687500061451502, 4.119189519843966529, -2.378215178124998275 ) ) ;
#15969 = CARTESIAN_POINT ( 'NONE',  ( 21.64687500061451786, 6.054752690667223547, 3.707466751127219781E-16 ) ) ;
#15970 = CARTESIAN_POINT ( 'NONE',  ( 12.83437500061451786, -2.746126346562641984, -4.756430356249999214 ) ) ;
#15971 = CARTESIAN_POINT ( 'NONE',  ( 8.728125000614518569, -4.541064518000419881, 2.621784821874995952 ) ) ;
#15972 = CARTESIAN_POINT ( 'NONE',  ( 12.23437500061451821, 4.541064518000418104, 2.621784821874999949 ) ) ;
#15973 = VERTEX_POINT ( 'NONE', #629 ) ;
#15974 = CARTESIAN_POINT ( 'NONE',  ( 21.90937500061451715, -4.541064518000417216, -2.621784821875001281 ) ) ;
#15975 = CARTESIAN_POINT ( 'NONE',  ( 29.09999999999999787, 0.000000000000000000, 4.999999999999998224 ) ) ;
#15976 = DIRECTION ( 'NONE',  ( -1.000000000000000000, -0.000000000000000000, -0.000000000000000000 ) ) ;
#15977 = CARTESIAN_POINT ( 'NONE',  ( 6.112499999999999822, 2.886751345948126879, 4.999999999999999112 ) ) ;
#15978 = CARTESIAN_POINT ( 'NONE',  ( 13.95000000122903572, -2.886751345948129988, 4.999999999999997335 ) ) ;
#15979 = CARTESIAN_POINT ( 'NONE',  ( -5.810221930991193690E-16, 12.35000000122903430, 26.00000000000000355 ) ) ;
#15980 = CARTESIAN_POINT ( 'NONE',  ( -1.071796769724491005, 19.00759618943233775, -34.00000000000000000 ) ) ;
#15981 = VERTEX_POINT ( 'NONE', #7241 ) ;
#15982 = CARTESIAN_POINT ( 'NONE',  ( 13.91249999999999964, -5.773502691896255534, -1.060575238724906372E-15 ) ) ;
#15983 = CARTESIAN_POINT ( 'NONE',  ( 15.90000000000000036, 4.330127018922192761, -2.499999999999997780 ) ) ;
#15984 = CARTESIAN_POINT ( 'NONE',  ( 13.65000000122903323, -2.886751345948125991, -5.000000000000000000 ) ) ;
#15985 = CARTESIAN_POINT ( 'NONE',  ( 11.99062500061451608, -3.027376345333610441, -5.243569643749999898 ) ) ;
#15987 = ORIENTED_EDGE ( 'NONE', *, *, #66859, .F. ) ;
#15986 = AXIS2_PLACEMENT_3D ( 'NONE', #14653, #42745, #21295 ) ;
#15988 = CARTESIAN_POINT ( 'NONE',  ( 8.962500000000002132, -5.773502691896255534, -1.060575238724906372E-15 ) ) ;
#15989 = DIRECTION ( 'NONE',  ( 0.000000000000000000, 0.000000000000000000, -1.000000000000000000 ) ) ;
#15990 = CARTESIAN_POINT ( 'NONE',  ( -4.243569643749999898, 13.55937500061451750, -30.00000000000000000 ) ) ;
#15991 = CARTESIAN_POINT ( 'NONE',  ( 3.328125000614516438, -4.541064518000419881, 2.621784821874995952 ) ) ;
#15992 = CARTESIAN_POINT ( 'NONE',  ( -1.878215178125001827, 14.74062499938548321, 33.25316411605952283 ) ) ;
#15993 = CARTESIAN_POINT ( 'NONE',  ( 8.775000000000002132, 4.330127018922191873, 2.499999999999999556 ) ) ;
#15994 = CARTESIAN_POINT ( 'NONE',  ( 0.000000000000000000, 27.50000000000000000, 30.00000000000000000 ) ) ;
#15995 = ORIENTED_EDGE ( 'NONE', *, *, #10637, .T. ) ;
#15996 = CARTESIAN_POINT ( 'NONE',  ( 24.21562500061451573, 3.027376345333613106, -5.243569643749998122 ) ) ;
#15997 = CARTESIAN_POINT ( 'NONE',  ( 3.519358070056033849, 3.551693405655444113, 3.553333502389941945 ) ) ;
#15998 = VECTOR ( 'NONE', #33266, 1000.000000000000000 ) ;
#15999 = CARTESIAN_POINT ( 'NONE',  ( 3.756430356249998770, 19.80312499938548498, 32.16877607737302469 ) ) ;
#16000 = CARTESIAN_POINT ( 'NONE',  ( 21.94687500061451857, -3.027376345333610441, -5.243569643749999898 ) ) ;
#16001 = CARTESIAN_POINT ( 'NONE',  ( 17.72812500061451502, -4.541064518000419881, 2.621784821874995952 ) ) ;
#16002 = CARTESIAN_POINT ( 'NONE',  ( 9.001249775931846008E-16, 10.91562500061459140, -25.09994784771203058 ) ) ;
#16003 = CARTESIAN_POINT ( 'NONE',  ( 7.378125000614518036, -4.541064518000419881, 2.621784821874995952 ) ) ;
#16004 = CARTESIAN_POINT ( 'NONE',  ( 3.215625000614518836, 3.027376345333611329, 5.243569643749999010 ) ) ;
#16005 = CARTESIAN_POINT ( 'NONE',  ( 23.55937500061451573, 0.000000000000000000, 4.756430356249998326 ) ) ;
#16006 = CARTESIAN_POINT ( 'NONE',  ( 19.34062500061451573, 6.054752690667223547, 3.707466751127219781E-16 ) ) ;
#16007 = DIRECTION ( 'NONE',  ( 0.000000000000000000, 0.000000000000000000, -1.000000000000000000 ) ) ;
#16008 = CARTESIAN_POINT ( 'NONE',  ( 3.756430356249998770, 18.00312499938548427, 32.16877607737302469 ) ) ;
#16009 =( BOUNDED_CURVE ( )  B_SPLINE_CURVE ( 2, ( #27119, #10124, #71080, #54099, #26381, #71453, #32655, #3496, #37464 ),
 .UNSPECIFIED., .F., .F. ) 
 B_SPLINE_CURVE_WITH_KNOTS ( ( 3, 2, 2, 2, 3 ),
 ( 0.3152173913043478382, 0.3188405797101449002, 0.3260869565217391353, 0.3333333333333333148, 0.3369565217391304324 ),
 .UNSPECIFIED. ) 
 CURVE ( )  GEOMETRIC_REPRESENTATION_ITEM ( )  RATIONAL_B_SPLINE_CURVE ( ( 0.9330127018922194093, 0.9330127018922198534, 1.000000000000000000, 0.8660254037844387076, 1.000000000000000000, 0.8660254037844387076, 1.000000000000000000, 0.9330127018922194093, 0.9330127018922194093 ) ) 
 REPRESENTATION_ITEM ( '' )  );
#16010 = CARTESIAN_POINT ( 'NONE',  ( 16.09687500061452070, -3.027376345333610441, -5.243569643749999898 ) ) ;
#16011 = CARTESIAN_POINT ( 'NONE',  ( 15.15937500061451715, -4.541064518000417216, -2.621784821875001281 ) ) ;
#16012 = CARTESIAN_POINT ( 'NONE',  ( 21.83437500061451786, -4.541064518000419881, 2.621784821874995952 ) ) ;
#16013 = VERTEX_POINT ( 'NONE', #51949 ) ;
#16014 = CARTESIAN_POINT ( 'NONE',  ( 2.121784821875001281, 12.35937500061451821, 33.67503911421598417 ) ) ;
#16015 = CARTESIAN_POINT ( 'NONE',  ( 3.553125000614516082, 4.541064518000418104, -2.621784821874998173 ) ) ;
#16016 = CARTESIAN_POINT ( 'NONE',  ( 27.59062500061451573, -3.027376345333614438, 5.243569643749998122 ) ) ;
#16017 = CARTESIAN_POINT ( 'NONE',  ( 27.36562500061451786, 3.027376345333613106, -5.243569643749998122 ) ) ;
#16018 = CARTESIAN_POINT ( 'NONE',  ( 45.00000000000000000, 0.000000000000000000, 0.000000000000000000 ) ) ;
#16019 = CARTESIAN_POINT ( 'NONE',  ( 1.999999999999998668, 18.95000000000000284, 26.53589838486224650 ) ) ;
#16020 = CARTESIAN_POINT ( 'NONE',  ( 5.671875000614519102, -6.054752690667223547, -1.112240025338166033E-15 ) ) ;
#16021 = DIRECTION ( 'NONE',  ( 1.000000000000000000, 0.000000000000000000, 0.000000000000000000 ) ) ;
#16022 = CARTESIAN_POINT ( 'NONE',  ( 12.22500000122903430, -5.773502691896255534, -1.060575238724906372E-15 ) ) ;
#16023 = CARTESIAN_POINT ( 'NONE',  ( 8.550000001229031810, -2.886751345948129988, 4.999999999999997335 ) ) ;
#16024 = CARTESIAN_POINT ( 'NONE',  ( 29.62500000122903288, 2.886751345948126879, 4.999999999999999112 ) ) ;
#16025 = CARTESIAN_POINT ( 'NONE',  ( 3.999999999999998668, 15.10624999877096641, 32.30940107675850470 ) ) ;
#16026 = CARTESIAN_POINT ( 'NONE',  ( 19.74375000122903145, -2.886751345948129988, 4.999999999999997335 ) ) ;
#16027 = CARTESIAN_POINT ( 'NONE',  ( 12.27187500061451786, 3.027376345333611329, 5.243569643749999010 ) ) ;
#16028 = CARTESIAN_POINT ( 'NONE',  ( 1.071796769724476572, 14.73259618943233562, -25.99999999999999289 ) ) ;
#16029 = ORIENTED_EDGE ( 'NONE', *, *, #27236, .T. ) ;
#16030 = CARTESIAN_POINT ( 'NONE',  ( 20.16562500061451146, 3.027376345333613106, -5.243569643749998122 ) ) ;
#16031 = CARTESIAN_POINT ( 'NONE',  ( 13.84687500061451537, -3.027376345333610441, -5.243569643749999898 ) ) ;
#16032 = CARTESIAN_POINT ( 'NONE',  ( 5.690625000614516260, -3.027376345333610441, -5.243569643749999898 ) ) ;
#16033 = CARTESIAN_POINT ( 'NONE',  ( 21.98437500061451644, 6.421520780324663323E-16, -5.243569643749999010 ) ) ;
#16034 = CARTESIAN_POINT ( 'NONE',  ( 5.240625000614516971, -3.027376345333610441, -5.243569643749999898 ) ) ;
#16035 = CARTESIAN_POINT ( 'NONE',  ( 28.42499999999999716, 6.123233995736764310E-16, -4.999999999999998224 ) ) ;
#16036 = CARTESIAN_POINT ( 'NONE',  ( 6.262500001229034829, 0.000000000000000000, 4.999999999999998224 ) ) ;
#16037 = CARTESIAN_POINT ( 'NONE',  ( 22.75312500061451360, -4.541064518000417216, -2.621784821875001281 ) ) ;
#16038 = CARTESIAN_POINT ( 'NONE',  ( 8.484601909799253346E-16, 18.42500000122903714, -25.38119784648299770 ) ) ;
#16039 = CARTESIAN_POINT ( 'NONE',  ( 8.175000001229031810, -5.773502691896255534, -1.060575238724906372E-15 ) ) ;
#16040 = CARTESIAN_POINT ( 'NONE',  ( 18.06562500061451715, 3.027376345333611329, 5.243569643749999010 ) ) ;
#16041 = CARTESIAN_POINT ( 'NONE',  ( 15.29062500061451679, 6.054752690667223547, 3.707466751127219781E-16 ) ) ;
#16042 = CARTESIAN_POINT ( 'NONE',  ( 25.28437500061451715, 4.119189519843966529, 2.378215178124999607 ) ) ;
#16043 = CARTESIAN_POINT ( 'NONE',  ( 16.27499999999999858, 6.123233995736764310E-16, -4.999999999999998224 ) ) ;
#16044 = CARTESIAN_POINT ( 'NONE',  ( 11.96250000122903501, 4.330127018922192761, -2.499999999999997780 ) ) ;
#16045 = CARTESIAN_POINT ( 'NONE',  ( 7.078125000614516438, 6.421520780324663323E-16, -5.243569643749999010 ) ) ;
#16046 = CARTESIAN_POINT ( 'NONE',  ( 10.37812500061451715, 4.541064518000418104, 2.621784821874999949 ) ) ;
#16047 = CARTESIAN_POINT ( 'NONE',  ( 21.75000000122903288, -2.886751345948125991, -5.000000000000000000 ) ) ;
#16048 = CARTESIAN_POINT ( 'NONE',  ( -4.243569643749999898, 13.07187500061452035, -32.45002607614398471 ) ) ;
#16049 = FACE_OUTER_BOUND ( 'NONE', #26733, .T. ) ;
#16050 = ADVANCED_FACE ( 'NONE', ( #17943 ), #6523, .F. ) ;
#16051 = CARTESIAN_POINT ( 'NONE',  ( 5.400000001229032343, -2.886751345948129988, 4.999999999999997335 ) ) ;
#16052 =( BOUNDED_CURVE ( )  B_SPLINE_CURVE ( 2, ( #32511, #60938, #56136, #33591, #21049, #60567, #43968, #9974, #49147 ),
 .UNSPECIFIED., .F., .F. ) 
 B_SPLINE_CURVE_WITH_KNOTS ( ( 3, 2, 2, 2, 3 ),
 ( 0.8586956521739130821, 0.8623188405797101996, 0.8695652173913043237, 0.8768115942028985588, 0.8804347826086956763 ),
 .UNSPECIFIED. ) 
 CURVE ( )  GEOMETRIC_REPRESENTATION_ITEM ( )  RATIONAL_B_SPLINE_CURVE ( ( 0.9330127018922194093, 0.9330127018922194093, 1.000000000000000000, 0.8660254037844387076, 1.000000000000000000, 0.8660254037844387076, 1.000000000000000000, 0.9330127018922194093, 0.9330127018922194093 ) ) 
 REPRESENTATION_ITEM ( '' )  );
#16053 = CARTESIAN_POINT ( 'NONE',  ( 4.546875000614517326, 6.054752690667223547, 3.707466751127219781E-16 ) ) ;
#16054 = CARTESIAN_POINT ( 'NONE',  ( 21.49687500061451573, -3.027376345333610441, -5.243569643749999898 ) ) ;
#16055 = CARTESIAN_POINT ( 'NONE',  ( 27.59999999999999787, 4.330127018922192761, -2.499999999999997780 ) ) ;
#16056 = CARTESIAN_POINT ( 'NONE',  ( 15.77812500061451573, 4.541064518000418104, 2.621784821874999949 ) ) ;
#16057 = CARTESIAN_POINT ( 'NONE',  ( 12.99375000122903323, -2.886751345948129988, 4.999999999999997335 ) ) ;
#16058 = CARTESIAN_POINT ( 'NONE',  ( -3.999999999999999112, 14.67500000122903536, 27.69059892324149885 ) ) ;
#16059 = CARTESIAN_POINT ( 'NONE',  ( 4.425000000000001599, -4.330127018922194537, 2.499999999999995559 ) ) ;
#16060 = CARTESIAN_POINT ( 'NONE',  ( 28.88437500061451502, 4.541064518000418104, 2.621784821874999949 ) ) ;
#16061 = CARTESIAN_POINT ( 'NONE',  ( 19.88437500061451502, -2.746126346562646425, 4.756430356249996549 ) ) ;
#16062 = CARTESIAN_POINT ( 'NONE',  ( 15.92812500061451608, -4.541064518000419881, 2.621784821874995952 ) ) ;
#16063 = CARTESIAN_POINT ( 'NONE',  ( 12.08437500061451608, 6.421520780324663323E-16, -5.243569643749999010 ) ) ;
#16064 = EDGE_LOOP ( 'NONE', ( #22492, #6172, #52959, #40738 ) ) ;
#16065 = CARTESIAN_POINT ( 'NONE',  ( 22.31249999999999645, 2.886751345948161074, 4.999999999999941380 ) ) ;
#16066 = CARTESIAN_POINT ( 'NONE',  ( 22.52812500061451573, 4.541064518000418104, 2.621784821874999949 ) ) ;
#16067 = CARTESIAN_POINT ( 'NONE',  ( 1.071796769724505438, 11.31740381056766864, -33.99999999999999289 ) ) ;
#16068 = CARTESIAN_POINT ( 'NONE',  ( 13.16249999999999964, 2.886751345948129099, -4.999999999999998224 ) ) ;
#16069 = CARTESIAN_POINT ( 'NONE',  ( 25.31250000122903288, -4.330127018922190985, -2.500000000000001332 ) ) ;
#16070 = CARTESIAN_POINT ( 'NONE',  ( 19.19062500061452070, -3.027376345333610441, -5.243569643749999898 ) ) ;
#16071 = CARTESIAN_POINT ( 'NONE',  ( 14.07187500061451679, -4.119189519843968306, 2.378215178124996054 ) ) ;
#16072 = ORIENTED_EDGE ( 'NONE', *, *, #893, .F. ) ;
#16073 = CARTESIAN_POINT ( 'NONE',  ( 19.42499999999999716, 6.123233995736764310E-16, -4.999999999999998224 ) ) ;
#16074 = CARTESIAN_POINT ( 'NONE',  ( 22.50937500061451857, 4.541064518000418104, -2.621784821874998173 ) ) ;
#16075 = CARTESIAN_POINT ( 'NONE',  ( 27.85312500061451502, 4.541064518000418104, -2.621784821874998173 ) ) ;
#16076 =( BOUNDED_CURVE ( )  B_SPLINE_CURVE ( 2, ( #46708, #63678, #40807, #565, #28990, #63322, #68877 ),
 .UNSPECIFIED., .F., .F. ) 
 B_SPLINE_CURVE_WITH_KNOTS ( ( 3, 2, 2, 3 ),
 ( 0.05833333333333334120, 0.06111111111111110911, 0.06388888888888888395, 0.06666666666666665186 ),
 .UNSPECIFIED. ) 
 CURVE ( )  GEOMETRIC_REPRESENTATION_ITEM ( )  RATIONAL_B_SPLINE_CURVE ( ( 0.9999999999999995559, 0.8660254037844390407, 1.000000000000000000, 0.8660254037844387076, 1.000000000000000000, 0.8660254037844393737, 0.9999999999999993339 ) ) 
 REPRESENTATION_ITEM ( '' )  );
#16077 = ORIENTED_EDGE ( 'NONE', *, *, #19175, .T. ) ;
#16078 = CARTESIAN_POINT ( 'NONE',  ( 1.999999999999998668, 18.05000000000000071, -33.46410161513775705 ) ) ;
#16079 = CARTESIAN_POINT ( 'NONE',  ( 10.34062500061451750, 6.054752690667223547, 3.707466751127219781E-16 ) ) ;
#16080 = CARTESIAN_POINT ( 'NONE',  ( 17.32500000122903216, 2.886751345948162850, -4.999999999999940492 ) ) ;
#16081 = CARTESIAN_POINT ( 'NONE',  ( 15.00937500061451502, -5.492252693125287522, -1.008910452111647106E-15 ) ) ;
#16082 = AXIS2_PLACEMENT_3D ( 'NONE', #49238, #55869, #27799 ) ;
#16083 = CARTESIAN_POINT ( 'NONE',  ( 17.51249999999999929, -5.773502691896255534, -1.060575238724906372E-15 ) ) ;
#16084 = CARTESIAN_POINT ( 'NONE',  ( 24.56250000000000000, 2.886751345948126879, 4.999999999999999112 ) ) ;
#16085 = CARTESIAN_POINT ( 'NONE',  ( -4.243569643749999898, 19.80312500061451786, 30.00000000000000000 ) ) ;
#16086 = CARTESIAN_POINT ( 'NONE',  ( 4.434375000614519280, 6.421520780324663323E-16, -5.243569643749999010 ) ) ;
#16087 = CARTESIAN_POINT ( 'NONE',  ( 27.45937500061451786, 4.541064518000418104, -2.621784821874998173 ) ) ;
#16088 = VERTEX_POINT ( 'NONE', #58192 ) ;
#16089 = CARTESIAN_POINT ( 'NONE',  ( 25.15312500061451217, 4.541064518000418104, -2.621784821874998173 ) ) ;
#16090 = CARTESIAN_POINT ( 'NONE',  ( 27.34687500061451360, -3.027376345333610441, -5.243569643749999898 ) ) ;
#16091 = CARTESIAN_POINT ( 'NONE',  ( 3.196875000614516793, 6.054752690667223547, 3.707466751127219781E-16 ) ) ;
#16092 = CARTESIAN_POINT ( 'NONE',  ( 13.72500000000000142, 4.330127018922191873, 2.499999999999999556 ) ) ;
#16093 = CARTESIAN_POINT ( 'NONE',  ( 10.90312500061451928, 0.000000000000000000, 5.243569643749999010 ) ) ;
#16094 = CARTESIAN_POINT ( 'NONE',  ( 4.898587196589411843E-16, 20.00000000000000000, 33.99999999999999289 ) ) ;
#16095 = CARTESIAN_POINT ( 'NONE',  ( 27.59062500061451573, -3.027376345333614438, 5.243569643749998122 ) ) ;
#16096 = CARTESIAN_POINT ( 'NONE',  ( 16.53750000122903430, 4.330127018922191873, 2.499999999999999556 ) ) ;
#16097 = CARTESIAN_POINT ( 'NONE',  ( 15.12187500061451750, -5.492252693125287522, -1.008910452111647106E-15 ) ) ;
#16098 = CARTESIAN_POINT ( 'NONE',  ( 4.940625000614515372, 6.054752690667223547, 3.707466751127219781E-16 ) ) ;
#16099 = CARTESIAN_POINT ( 'NONE',  ( 21.27187500061451786, 3.027376345333611329, 5.243569643749999010 ) ) ;
#16100 = CARTESIAN_POINT ( 'NONE',  ( 9.001249775931846008E-16, 15.47187500061451892, 34.90005215228797653 ) ) ;
#16101 = CARTESIAN_POINT ( 'NONE',  ( 21.90937500061451715, -4.541064518000417216, -2.621784821875001281 ) ) ;
#16102 = CARTESIAN_POINT ( 'NONE',  ( 28.50937500061451502, 0.000000000000000000, 5.243569643749999010 ) ) ;
#16103 = CARTESIAN_POINT ( 'NONE',  ( 2.121784821874999061, 17.90937500061451715, 26.32496088578401583 ) ) ;
#16104 = CARTESIAN_POINT ( 'NONE',  ( 9.103125000614515017, 0.000000000000000000, 5.243569643749999010 ) ) ;
#16105 = CARTESIAN_POINT ( 'NONE',  ( 0.000000000000000000, 0.000000000000000000, 50.00000000000000000 ) ) ;
#16106 = CARTESIAN_POINT ( 'NONE',  ( 6.609375000614519102, -4.541064518000417216, -2.621784821875001281 ) ) ;
#16107 = FACE_OUTER_BOUND ( 'NONE', #21333, .T. ) ;
#16108 =( BOUNDED_CURVE ( )  B_SPLINE_CURVE ( 2, ( #32782, #60110, #20583, #55319, #4713, #26514, #27247 ),
 .UNSPECIFIED., .F., .F. ) 
 B_SPLINE_CURVE_WITH_KNOTS ( ( 3, 2, 2, 3 ),
 ( 0.7700000000000001288, 0.7733333333333334281, 0.7766666666666667274, 0.7800000000000001377 ),
 .UNSPECIFIED. ) 
 CURVE ( )  GEOMETRIC_REPRESENTATION_ITEM ( )  RATIONAL_B_SPLINE_CURVE ( ( 0.9999999999999955591, 0.8660254037844431485, 1.000000000000000000, 0.8660254037844387076, 1.000000000000000000, 0.8660254037844342667, 1.000000000000004441 ) ) 
 REPRESENTATION_ITEM ( '' )  );
#16109 = CARTESIAN_POINT ( 'NONE',  ( 8.578125000614518214, 4.541064518000418104, 2.621784821874999949 ) ) ;
#16110 = CARTESIAN_POINT ( 'NONE',  ( 11.59687500061451892, -3.027376345333610441, -5.243569643749999898 ) ) ;
#16111 = CARTESIAN_POINT ( 'NONE',  ( 20.85000000122903430, -2.886751345948125991, -5.000000000000000000 ) ) ;
#16112 = CARTESIAN_POINT ( 'NONE',  ( 7.734375000614517326, 4.541064518000418104, 2.621784821874999949 ) ) ;
#16113 = CARTESIAN_POINT ( 'NONE',  ( 11.05312500061451608, -4.541064518000417216, -2.621784821875001281 ) ) ;
#16114 = CARTESIAN_POINT ( 'NONE',  ( 6.853125000614516793, 0.000000000000000000, 5.243569643749999010 ) ) ;
#16115 = CARTESIAN_POINT ( 'NONE',  ( 24.95625000122903003, 4.330127018922192761, -2.499999999999997780 ) ) ;
#16116 = CARTESIAN_POINT ( 'NONE',  ( 19.65937500061451360, -4.541064518000417216, -2.621784821875001281 ) ) ;
#16117 = CARTESIAN_POINT ( 'NONE',  ( 1.626862140677534273E-15, 13.02500000122903323, 34.00000000000000000 ) ) ;
#16118 = CARTESIAN_POINT ( 'NONE',  ( 11.84062500061451750, -3.027376345333614438, 5.243569643749998122 ) ) ;
#16119 = CARTESIAN_POINT ( 'NONE',  ( 29.48437500061451644, -4.541064518000419881, 2.621784821874995952 ) ) ;
#16120 = CARTESIAN_POINT ( 'NONE',  ( 9.001249775931846008E-16, 11.87187500061451395, -25.09994784771203058 ) ) ;
#16121 = CARTESIAN_POINT ( 'NONE',  ( 15.75000000122902932, -2.886751345948129988, 4.999999999999997335 ) ) ;
#16122 = EDGE_CURVE ( 'NONE', #45352, #67346, #52665, .T. ) ;
#16123 = CARTESIAN_POINT ( 'NONE',  ( 2.121784821874999061, 14.70312500061451644, -33.67503911421598417 ) ) ;
#16124 = CARTESIAN_POINT ( 'NONE',  ( 16.08750000122903501, 4.330127018922191873, 2.499999999999999556 ) ) ;
#16125 = CARTESIAN_POINT ( 'NONE',  ( 10.82812500061451644, 4.541064518000418104, 2.621784821874999949 ) ) ;
#16126 = ORIENTED_EDGE ( 'NONE', *, *, #32305, .T. ) ;
#16127 = CARTESIAN_POINT ( 'NONE',  ( 13.72500000000000142, 4.330127018922191873, 2.499999999999999556 ) ) ;
#16128 = CARTESIAN_POINT ( 'NONE',  ( -2.000000000000000000, 13.62500000000000178, 26.53589838486224650 ) ) ;
#16129 = AXIS2_PLACEMENT_3D ( 'NONE', #52434, #13622, #62514 ) ;
#16130 = CARTESIAN_POINT ( 'NONE',  ( 23.16562500061451502, -6.054752690667223547, -1.112240025338166033E-15 ) ) ;
#16131 = CARTESIAN_POINT ( 'NONE',  ( 7.959375000614516971, -4.541064518000417216, -2.621784821875001281 ) ) ;
#16132 = EDGE_CURVE ( 'NONE', #71866, #37421, #57709, .T. ) ;
#16133 = CARTESIAN_POINT ( 'NONE',  ( 10.72500000122903252, 2.886751345948126879, 4.999999999999999112 ) ) ;
#16134 = CARTESIAN_POINT ( 'NONE',  ( 19.42500000122903714, -5.773502691896255534, -1.060575238724906372E-15 ) ) ;
#16135 = CARTESIAN_POINT ( 'NONE',  ( 15.55312500061451608, -4.541064518000417216, -2.621784821875001281 ) ) ;
#16136 = EDGE_CURVE ( 'NONE', #28731, #69794, #3791, .T. ) ;
#16137 = CARTESIAN_POINT ( 'NONE',  ( 18.40312500061451573, 4.541064518000418104, -2.621784821874998173 ) ) ;
#16138 = CARTESIAN_POINT ( 'NONE',  ( 26.28750000122903430, 6.123233995736764310E-16, -4.999999999999998224 ) ) ;
#16139 = CARTESIAN_POINT ( 'NONE',  ( 27.30000000122903359, 5.773502691896255534, 3.535250795749688894E-16 ) ) ;
#16140 = CARTESIAN_POINT ( 'NONE',  ( 22.64999999999999858, 4.330127018922192761, -2.499999999999997780 ) ) ;
#16141 = CARTESIAN_POINT ( 'NONE',  ( 1.878215178124997609, 14.36562499938548321, 33.25316411605952993 ) ) ;
#16142 = AXIS2_PLACEMENT_3D ( 'NONE', #6160, #24225, #57836 ) ;
#16143 = CARTESIAN_POINT ( 'NONE',  ( 26.85937500061451644, -4.541064518000417216, -2.621784821875001281 ) ) ;
#16144 = CARTESIAN_POINT ( 'NONE',  ( 13.12500000122903288, -5.773502691896255534, -1.060575238724906372E-15 ) ) ;
#16145 = CARTESIAN_POINT ( 'NONE',  ( 29.18437500061451573, 6.421520780324663323E-16, -5.243569643749999010 ) ) ;
#16146 = CARTESIAN_POINT ( 'NONE',  ( 0.000000000000000000, 20.00000000000000000, 30.00000000000000000 ) ) ;
#16147 = CARTESIAN_POINT ( 'NONE',  ( 5.296875000614518214, -3.027376345333610441, -5.243569643749999898 ) ) ;
#16148 = CARTESIAN_POINT ( 'NONE',  ( 26.05312500061451431, 4.541064518000418104, -2.621784821874998173 ) ) ;
#16149 = CARTESIAN_POINT ( 'NONE',  ( -3.756430356250000990, 13.91562499938548392, 32.16877607737301048 ) ) ;
#16150 = LINE ( 'NONE', #68228, #3165 ) ;
#16151 = CARTESIAN_POINT ( 'NONE',  ( 9.796875000614519990, -3.027376345333610441, -5.243569643749999898 ) ) ;
#16152 = CARTESIAN_POINT ( 'NONE',  ( 22.16250000122903074, -4.330127018922190985, -2.500000000000001332 ) ) ;
#16153 = CARTESIAN_POINT ( 'NONE',  ( 2.934375000614518392, -4.541064518000419881, 2.621784821874995952 ) ) ;
#16154 = CARTESIAN_POINT ( 'NONE',  ( 5.409375000614516260, 4.541064518000418104, -2.621784821874998173 ) ) ;
#16155 = CARTESIAN_POINT ( 'NONE',  ( 27.83437500061451786, 6.421520780324663323E-16, -5.243569643749999010 ) ) ;
#16156 = EDGE_CURVE ( 'NONE', #38031, #17018, #32692, .T. ) ;
#16157 = CARTESIAN_POINT ( 'NONE',  ( 9.001249775931846008E-16, 10.01562500061459637, 34.90005215228797653 ) ) ;
#16158 = CARTESIAN_POINT ( 'NONE',  ( 19.12500000000000000, 4.330127018922191873, 2.499999999999999556 ) ) ;
#16159 = ORIENTED_EDGE ( 'NONE', *, *, #14554, .F. ) ;
#16160 = CARTESIAN_POINT ( 'NONE',  ( 26.66250000000000142, 2.886751345948129099, -4.999999999999998224 ) ) ;
#16161 = CARTESIAN_POINT ( 'NONE',  ( 28.88437500061451502, 4.541064518000418104, 2.621784821874999949 ) ) ;
#16162 = ORIENTED_EDGE ( 'NONE', *, *, #28153, .T. ) ;
#16163 = CARTESIAN_POINT ( 'NONE',  ( 18.25312500061451715, -4.541064518000417216, -2.621784821875001281 ) ) ;
#16164 = CARTESIAN_POINT ( 'NONE',  ( 7.715625000614515727, 3.027376345333611329, 5.243569643749999010 ) ) ;
#16165 = CARTESIAN_POINT ( 'NONE',  ( 20.67187500061451289, 4.119189519843966529, 2.378215178124999607 ) ) ;
#16166 = CARTESIAN_POINT ( 'NONE',  ( 6.046875000614519102, -3.027376345333614438, 5.243569643749998122 ) ) ;
#16167 = CARTESIAN_POINT ( 'NONE',  ( 17.62500000122903288, -5.773502691896255534, -1.060575238724906372E-15 ) ) ;
#16168 = CARTESIAN_POINT ( 'NONE',  ( 1.071796769724491227, 19.79240381056766651, 26.00000000000000000 ) ) ;
#16169 = CARTESIAN_POINT ( 'NONE',  ( 7.846875000614518036, -3.027376345333614438, 5.243569643749998122 ) ) ;
#16170 = CARTESIAN_POINT ( 'NONE',  ( 12.90937500061451537, -4.541064518000417216, -2.621784821875001281 ) ) ;
#16171 = CARTESIAN_POINT ( 'NONE',  ( 22.99687500061451573, 6.054752690667223547, 3.707466751127219781E-16 ) ) ;
#16172 = CARTESIAN_POINT ( 'NONE',  ( -1.999999999999997113, 14.67500000000000071, -26.53589838486224295 ) ) ;
#16173 = ORIENTED_EDGE ( 'NONE', *, *, #33228, .T. ) ;
#16174 = CARTESIAN_POINT ( 'NONE',  ( 11.06250000000000000, 2.886751345948126879, 4.999999999999999112 ) ) ;
#16175 = CARTESIAN_POINT ( 'NONE',  ( 16.88437500061451502, -4.541064518000419881, 2.621784821874995952 ) ) ;
#16176 = CARTESIAN_POINT ( 'NONE',  ( 8.371875000614515727, -6.054752690667223547, -1.112240025338166033E-15 ) ) ;
#16177 = AXIS2_PLACEMENT_3D ( 'NONE', #52364, #12114, #23188 ) ;
#16178 = CARTESIAN_POINT ( 'NONE',  ( -3.756430356250000102, 14.66562499938548214, 30.00000000000000000 ) ) ;
#16179 = CARTESIAN_POINT ( 'NONE',  ( 20.99999999999999645, 0.000000000000000000, 4.999999999999998224 ) ) ;
#16180 = CARTESIAN_POINT ( 'NONE',  ( -8.484601909799255319E-16, 17.33749999999999858, 34.61880215351700940 ) ) ;
#16181 = CARTESIAN_POINT ( 'NONE',  ( 9.001249775931846008E-16, 10.07187500061451857, -25.09994784771203058 ) ) ;
#16182 = CARTESIAN_POINT ( 'NONE',  ( 21.53437500061451715, 5.824947211148865298E-16, -4.756430356249998326 ) ) ;
#16183 = CARTESIAN_POINT ( 'NONE',  ( 11.95312500061451644, -4.541064518000417216, -2.621784821875001281 ) ) ;
#16184 = CARTESIAN_POINT ( 'NONE',  ( 29.67187500061451644, 3.027376345333613106, -5.243569643749998122 ) ) ;
#16185 = DIRECTION ( 'NONE',  ( 0.000000000000000000, 0.000000000000000000, 1.000000000000000000 ) ) ;
#16186 = CARTESIAN_POINT ( 'NONE',  ( 29.85937500061451644, 0.000000000000000000, 5.243569643749999010 ) ) ;
#16187 = CARTESIAN_POINT ( 'NONE',  ( 10.49999999999999822, 4.330127018922192761, -2.499999999999997780 ) ) ;
#16188 = CARTESIAN_POINT ( 'NONE',  ( 2.000000000000001332, 16.66250000122903430, 33.46410161513774995 ) ) ;
#16189 = CARTESIAN_POINT ( 'NONE',  ( 9.187500001229034652, 6.123233995736764310E-16, -4.999999999999998224 ) ) ;
#16190 = CARTESIAN_POINT ( 'NONE',  ( 19.80937500061451573, 4.541064518000418104, -2.621784821874998173 ) ) ;
#16191 = CARTESIAN_POINT ( 'NONE',  ( 14.18437500061451750, -4.541064518000419881, 2.621784821874995952 ) ) ;
#16192 = CARTESIAN_POINT ( 'NONE',  ( 3.989788714780147405, 3.013600307987785776, -4.291086904670110336 ) ) ;
#16193 = ORIENTED_EDGE ( 'NONE', *, *, #8865, .F. ) ;
#16194 = CARTESIAN_POINT ( 'NONE',  ( 13.94062500061451892, 6.054752690667223547, 3.707466751127219781E-16 ) ) ;
#16195 = CARTESIAN_POINT ( 'NONE',  ( 28.87500000122902932, -5.773502691896255534, -1.060575238724906372E-15 ) ) ;
#16196 = CARTESIAN_POINT ( 'NONE',  ( 16.02187500061451786, -6.054752690667223547, -1.112240025338166033E-15 ) ) ;
#16197 = CARTESIAN_POINT ( 'NONE',  ( 2.953125000614516438, -4.541064518000417216, -2.621784821875001281 ) ) ;
#16198 = CARTESIAN_POINT ( 'NONE',  ( 16.82812500061451644, -4.541064518000419881, 2.621784821874995952 ) ) ;
#16199 = CARTESIAN_POINT ( 'NONE',  ( 18.11250000122903359, -4.330127018922190985, -2.500000000000001332 ) ) ;
#16200 = CARTESIAN_POINT ( 'NONE',  ( 26.03437500061451715, 6.421520780324663323E-16, -5.243569643749999010 ) ) ;
#16201 = CARTESIAN_POINT ( 'NONE',  ( 2.121784821874999061, 13.35312500061451679, 26.32496088578401583 ) ) ;
#16202 = CARTESIAN_POINT ( 'NONE',  ( 15.90937500061451892, 0.000000000000000000, 5.243569643749999010 ) ) ;
#16203 = CARTESIAN_POINT ( 'NONE',  ( 14.32500000122903394, 2.886751345948126879, 4.999999999999999112 ) ) ;
#16204 = CARTESIAN_POINT ( 'NONE',  ( 9.459375000614517859, 4.119189519843966529, -2.378215178124998275 ) ) ;
#16205 = CARTESIAN_POINT ( 'NONE',  ( -3.000416591977282496E-16, 18.39687500061451786, -34.90005215228797653 ) ) ;
#16206 = CARTESIAN_POINT ( 'NONE',  ( 19.58437500061451786, -4.541064518000419881, 2.621784821874995952 ) ) ;
#16207 = CARTESIAN_POINT ( 'NONE',  ( 22.31250000122903288, 4.330127018922192761, -2.499999999999997780 ) ) ;
#16208 = CARTESIAN_POINT ( 'NONE',  ( 16.43437500061451573, -4.541064518000419881, 2.621784821874995952 ) ) ;
#16209 = CARTESIAN_POINT ( 'NONE',  ( -2.121784821874999949, 11.68437500061451750, 26.32496088578401938 ) ) ;
#16210 = CARTESIAN_POINT ( 'NONE',  ( 17.12812500061451715, 4.541064518000418104, 2.621784821874999949 ) ) ;
#16211 = ORIENTED_EDGE ( 'NONE', *, *, #41487, .F. ) ;
#16212 = ORIENTED_EDGE ( 'NONE', *, *, #31507, .F. ) ;
#16213 = CARTESIAN_POINT ( 'NONE',  ( 19.87500000000000000, 6.123233995736764310E-16, -4.999999999999998224 ) ) ;
#16214 = CARTESIAN_POINT ( 'NONE',  ( 34.99999999999999289, -2.499999999999999556, -3.499999999999999556 ) ) ;
#16215 = CARTESIAN_POINT ( 'NONE',  ( 24.85312500061451502, 0.000000000000000000, 5.243569643749999010 ) ) ;
#16216 = CARTESIAN_POINT ( 'NONE',  ( 5.128125000614516260, -4.541064518000419881, 2.621784821874995952 ) ) ;
#16217 = CARTESIAN_POINT ( 'NONE',  ( 16.68750000122903288, -4.330127018922194537, 2.499999999999995559 ) ) ;
#16218 = CARTESIAN_POINT ( 'NONE',  ( 22.64062500061451644, -3.027376345333614438, 5.243569643749998122 ) ) ;
#16219 = CARTESIAN_POINT ( 'NONE',  ( 21.44999999999999929, 0.000000000000000000, 4.999999999999998224 ) ) ;
#16220 = EDGE_CURVE ( 'NONE', #35360, #27263, #62468, .T. ) ;
#16221 = EDGE_CURVE ( 'NONE', #9071, #47727, #32824, .T. ) ;
#16222 = CARTESIAN_POINT ( 'NONE',  ( 25.34062500061451217, -3.027376345333614438, 5.243569643749998122 ) ) ;
#16223 = CARTESIAN_POINT ( 'NONE',  ( 5.653125000614517504, -4.541064518000417216, -2.621784821875001281 ) ) ;
#16224 = EDGE_LOOP ( 'NONE', ( #17246, #9564, #52685, #16581 ) ) ;
#16225 = CARTESIAN_POINT ( 'NONE',  ( 26.92500000122903003, 2.886751345948161074, 4.999999999999941380 ) ) ;
#16226 = CARTESIAN_POINT ( 'NONE',  ( 4.040625000614517681, 6.054752690667223547, 3.707466751127219781E-16 ) ) ;
#16227 = CARTESIAN_POINT ( 'NONE',  ( 11.67187500061451821, 2.746126346562645981, -4.756430356249997438 ) ) ;
#16228 = CARTESIAN_POINT ( 'NONE',  ( 3.999999999999998668, 11.37500000122903288, -32.30940107675850470 ) ) ;
#16229 = CARTESIAN_POINT ( 'NONE',  ( 2.121784821874999061, 17.90937500061451715, -33.67503911421598417 ) ) ;
#16230 = CIRCLE ( 'NONE', #61050, 9.000000000000000000 ) ;
#16231 = CARTESIAN_POINT ( 'NONE',  ( 8.324999999999999289, 4.330127018922191873, 2.499999999999999556 ) ) ;
#16232 = CARTESIAN_POINT ( 'NONE',  ( 9.834375000614517859, 6.421520780324663323E-16, -5.243569643749999010 ) ) ;
#16233 = CARTESIAN_POINT ( 'NONE',  ( 6.112500001229034474, 4.330127018922192761, -2.499999999999997780 ) ) ;
#16234 = CARTESIAN_POINT ( 'NONE',  ( 11.52187500061451608, -6.054752690667223547, -1.112240025338166033E-15 ) ) ;
#16235 = CARTESIAN_POINT ( 'NONE',  ( 3.909375000614518481, -4.541064518000417216, -2.621784821875001281 ) ) ;
#16236 = CARTESIAN_POINT ( 'NONE',  ( 12.03749999999999964, -2.886751345948130876, 4.999999999999996447 ) ) ;
#16237 = LINE ( 'NONE', #60201, #31231 ) ;
#16238 = CARTESIAN_POINT ( 'NONE',  ( 10.20937500061451786, -4.541064518000417216, -2.621784821875001281 ) ) ;
#16239 = CARTESIAN_POINT ( 'NONE',  ( 20.20312500061451644, 4.541064518000418104, -2.621784821874998173 ) ) ;
#16240 = CARTESIAN_POINT ( 'NONE',  ( -3.137519842735245283E-14, 11.56250000000000178, 34.00000000000000000 ) ) ;
#16241 = CARTESIAN_POINT ( 'NONE',  ( 4.243569643749999898, 19.54062500061459673, 32.45002607614398471 ) ) ;
#16242 = CARTESIAN_POINT ( 'NONE',  ( 23.33437500061451786, 6.421520780324663323E-16, -5.243569643749999010 ) ) ;
#16243 = CARTESIAN_POINT ( 'NONE',  ( 28.12500000122902932, 2.886751345948129099, -4.999999999999998224 ) ) ;
#16244 = CARTESIAN_POINT ( 'NONE',  ( 20.29687500061451289, 0.000000000000000000, 4.756430356249998326 ) ) ;
#16245 = CARTESIAN_POINT ( 'NONE',  ( 25.00312500061451715, -4.541064518000417216, -2.621784821875001281 ) ) ;
#16246 = CARTESIAN_POINT ( 'NONE',  ( 15.92812500061451608, -4.541064518000419881, 2.621784821874995952 ) ) ;
#16247 = CARTESIAN_POINT ( 'NONE',  ( 14.04375000122903394, -2.886751345948125991, -5.000000000000000000 ) ) ;
#16248 = CARTESIAN_POINT ( 'NONE',  ( 13.50937500061451679, 4.541064518000418104, -2.621784821874998173 ) ) ;
#16249 = CARTESIAN_POINT ( 'NONE',  ( 7.246875000614514839, 0.000000000000000000, 4.756430356249998326 ) ) ;
#16250 = CARTESIAN_POINT ( 'NONE',  ( 25.12500000122903288, 2.886751345948126879, 4.999999999999999112 ) ) ;
#16251 = CARTESIAN_POINT ( 'NONE',  ( 2.955228467731844333, 4.033190387708875946, -2.955228467731844333 ) ) ;
#16252 = CARTESIAN_POINT ( 'NONE',  ( 15.08437500061451786, -4.541064518000419881, 2.621784821874995952 ) ) ;
#16253 = CARTESIAN_POINT ( 'NONE',  ( 21.50625000122903074, 0.000000000000000000, 4.999999999999998224 ) ) ;
#16254 = CARTESIAN_POINT ( 'NONE',  ( 24.14999999999999858, 0.000000000000000000, 4.999999999999998224 ) ) ;
#16255 = EDGE_CURVE ( 'NONE', #55334, #70765, #62765, .T. ) ;
#16256 = CARTESIAN_POINT ( 'NONE',  ( -3.999999999999999112, 12.34999999999999964, -30.00000000000000000 ) ) ;
#16257 = CARTESIAN_POINT ( 'NONE',  ( 25.73437500061451644, 4.541064518000418104, 2.621784821874999949 ) ) ;
#16258 = CARTESIAN_POINT ( 'NONE',  ( 15.90937500061451892, 0.000000000000000000, 5.243569643749999010 ) ) ;
#16259 = CARTESIAN_POINT ( 'NONE',  ( -3.756430356250001434, 17.06562499938548427, 32.16877607737301048 ) ) ;
#16260 = CARTESIAN_POINT ( 'NONE',  ( 27.33750000000000213, -2.886751345948129988, 4.999999999999997335 ) ) ;
#16261 = CARTESIAN_POINT ( 'NONE',  ( 2.925000001229034918, 2.886751345948129099, -4.999999999999998224 ) ) ;
#16262 = CARTESIAN_POINT ( 'NONE',  ( 4.537500000000000533, -2.886751345948125991, -5.000000000000000000 ) ) ;
#16263 = CARTESIAN_POINT ( 'NONE',  ( 8.146875000614516082, 0.000000000000000000, 4.756430356249998326 ) ) ;
#16264 = CARTESIAN_POINT ( 'NONE',  ( 20.35312500061451502, 0.000000000000000000, 5.243569643749999010 ) ) ;
#16265 = CARTESIAN_POINT ( 'NONE',  ( 9.525000000000002132, 6.123233995736764310E-16, -4.999999999999998224 ) ) ;
#16266 = CARTESIAN_POINT ( 'NONE',  ( 4.265625000614517326, -6.054752690667223547, -1.112240025338166033E-15 ) ) ;
#16267 = CARTESIAN_POINT ( 'NONE',  ( 17.06250000000000000, -5.773502691896255534, -1.060575238724906372E-15 ) ) ;
#16268 = CARTESIAN_POINT ( 'NONE',  ( -3.999999999999999112, 17.26249999999999929, 27.69059892324149885 ) ) ;
#16269 = CARTESIAN_POINT ( 'NONE',  ( 21.75000000122903288, -2.886751345948125991, -5.000000000000000000 ) ) ;
#16270 = LINE ( 'NONE', #26644, #26503 ) ;
#16271 = CARTESIAN_POINT ( 'NONE',  ( 28.13437500061451502, -4.541064518000419881, 2.621784821874995952 ) ) ;
#16272 = VERTEX_POINT ( 'NONE', #43419 ) ;
#16273 = CARTESIAN_POINT ( 'NONE',  ( 17.16562500061451502, 3.027376345333611329, 5.243569643749999010 ) ) ;
#16274 = CARTESIAN_POINT ( 'NONE',  ( 23.87812500061451715, 4.541064518000418104, 2.621784821874999949 ) ) ;
#16275 = CARTESIAN_POINT ( 'NONE',  ( 23.48437500061451644, 4.541064518000418104, 2.621784821874999949 ) ) ;
#16276 = CARTESIAN_POINT ( 'NONE',  ( 6.450000000000001066, 4.330127018922192761, -2.499999999999997780 ) ) ;
#16277 = CARTESIAN_POINT ( 'NONE',  ( 9.628125000614517148, -4.541064518000419881, 2.621784821874995952 ) ) ;
#16278 = CARTESIAN_POINT ( 'NONE',  ( 25.30312500061451431, 0.000000000000000000, 5.243569643749999010 ) ) ;
#16279 = CARTESIAN_POINT ( 'NONE',  ( 14.67187500061451821, -6.054752690667223547, -1.112240025338166033E-15 ) ) ;
#16280 = CARTESIAN_POINT ( 'NONE',  ( 19.95937500061451786, 0.000000000000000000, 5.243569643749999010 ) ) ;
#16281 = CARTESIAN_POINT ( 'NONE',  ( 1.071796769724491893, 11.69509619066136885, -26.00000000000000355 ) ) ;
#16282 = CARTESIAN_POINT ( 'NONE',  ( 2.121784821874999061, 10.70937500061451964, 26.32496088578401583 ) ) ;
#16283 = VECTOR ( 'NONE', #25048, 1000.000000000000000 ) ;
#16284 = CARTESIAN_POINT ( 'NONE',  ( 20.81250000122903643, -4.330127018922190985, -2.500000000000001332 ) ) ;
#16285 = CARTESIAN_POINT ( 'NONE',  ( 17.10937500061451999, 4.119189519843966529, -2.378215178124998275 ) ) ;
#16286 = CARTESIAN_POINT ( 'NONE',  ( 12.17812500061451608, 4.541064518000418104, 2.621784821874999949 ) ) ;
#16287 = CARTESIAN_POINT ( 'NONE',  ( 8.521875000614516082, 3.027376345333613106, -5.243569643749998122 ) ) ;
#16288 = CARTESIAN_POINT ( 'NONE',  ( 6.646875000614518747, -3.027376345333610441, -5.243569643749999898 ) ) ;
#16289 = ORIENTED_EDGE ( 'NONE', *, *, #67586, .F. ) ;
#16290 = CARTESIAN_POINT ( 'NONE',  ( 27.45937500061451786, 4.541064518000418104, -2.621784821874998173 ) ) ;
#16291 = CARTESIAN_POINT ( 'NONE',  ( 20.31562500061451715, 3.027376345333611329, 5.243569643749999010 ) ) ;
#16292 = CARTESIAN_POINT ( 'NONE',  ( 29.06250000122903288, 4.330127018922192761, -2.499999999999997780 ) ) ;
#16293 =( BOUNDED_CURVE ( )  B_SPLINE_CURVE ( 2, ( #21342, #50528, #9901, #27632, #66797, #38340, #5459, #16168, #10271 ),
 .UNSPECIFIED., .F., .F. ) 
 B_SPLINE_CURVE_WITH_KNOTS ( ( 3, 2, 2, 2, 3 ),
 ( 0.8750000000000000000, 0.8796296296296296502, 0.8888888888888888395, 0.8981481481481481399, 0.9027777777777777901 ),
 .UNSPECIFIED. ) 
 CURVE ( )  GEOMETRIC_REPRESENTATION_ITEM ( )  RATIONAL_B_SPLINE_CURVE ( ( 0.9330127018922194093, 0.9330127018922194093, 1.000000000000000000, 0.8660254037844387076, 1.000000000000000000, 0.8660254037844387076, 1.000000000000000000, 0.9330127018922194093, 0.9330127018922194093 ) ) 
 REPRESENTATION_ITEM ( '' )  );
#16294 = CARTESIAN_POINT ( 'NONE',  ( 26.91562500061451146, 3.027376345333613106, -5.243569643749998122 ) ) ;
#16295 = CARTESIAN_POINT ( 'NONE',  ( 24.60937500061451644, -4.541064518000417216, -2.621784821875001281 ) ) ;
#16296 = CARTESIAN_POINT ( 'NONE',  ( 19.67812500061451786, 6.421520780324663323E-16, -5.243569643749999010 ) ) ;
#16297 = CARTESIAN_POINT ( 'NONE',  ( -4.243569643749999898, 18.50937500061451857, 30.00000000000000000 ) ) ;
#16298 = CARTESIAN_POINT ( 'NONE',  ( 24.62812500061451715, 6.421520780324663323E-16, -5.243569643749999010 ) ) ;
#16299 = CARTESIAN_POINT ( 'NONE',  ( 3.562500001229033764, 0.000000000000000000, 4.999999999999998224 ) ) ;
#16300 = VERTEX_POINT ( 'NONE', #37498 ) ;
#16301 = CARTESIAN_POINT ( 'NONE',  ( 27.63749999999999929, 5.773502691896255534, 3.535250795749688894E-16 ) ) ;
#16302 = CARTESIAN_POINT ( 'NONE',  ( 3.999999999999998668, 15.31250000000000000, -32.30940107675850470 ) ) ;
#16303 = CARTESIAN_POINT ( 'NONE',  ( 1.878215178125000495, 18.67812499938548143, 26.74683588394047007 ) ) ;
#16304 = CARTESIAN_POINT ( 'NONE',  ( 4.284375000614518925, -4.541064518000419881, 2.621784821874995952 ) ) ;
#16305 = CARTESIAN_POINT ( 'NONE',  ( 13.19062500061451537, -3.027376345333614438, 5.243569643749998122 ) ) ;
#16306 = CARTESIAN_POINT ( 'NONE',  ( 6.046875000614519102, -3.027376345333614438, 5.243569643749998122 ) ) ;
#16307 = CARTESIAN_POINT ( 'NONE',  ( 24.60000000122903430, 5.773502691896255534, 3.535250795749688894E-16 ) ) ;
#16308 = CARTESIAN_POINT ( 'NONE',  ( 15.00937500061451679, 0.000000000000000000, 5.243569643749999010 ) ) ;
#16309 = CARTESIAN_POINT ( 'NONE',  ( 29.16562500061451502, 3.027376345333613106, -5.243569643749998122 ) ) ;
#16310 = CARTESIAN_POINT ( 'NONE',  ( 29.47499999999999787, 4.330127018922191873, 2.499999999999999556 ) ) ;
#16311 = CARTESIAN_POINT ( 'NONE',  ( 26.48437500061451644, 6.421520780324663323E-16, -5.243569643749999010 ) ) ;
#16312 = CARTESIAN_POINT ( 'NONE',  ( 3.403125000614518836, -4.541064518000417216, -2.621784821875001281 ) ) ;
#16313 = CARTESIAN_POINT ( 'NONE',  ( 12.44062500061451537, -3.027376345333610441, -5.243569643749999898 ) ) ;
#16314 = VERTEX_POINT ( 'NONE', #60018 ) ;
#16315 = CARTESIAN_POINT ( 'NONE',  ( 9.965625000614517504, 3.027376345333611329, 5.243569643749999010 ) ) ;
#16316 = CARTESIAN_POINT ( 'NONE',  ( 7.340625000614518392, -3.027376345333614438, 5.243569643749998122 ) ) ;
#16317 = CARTESIAN_POINT ( 'NONE',  ( 19.02187500061451786, 2.746126346562643317, 4.756430356249998326 ) ) ;
#16318 = CARTESIAN_POINT ( 'NONE',  ( 9.299999999999998934, 0.000000000000000000, 4.999999999999998224 ) ) ;
#16319 = CARTESIAN_POINT ( 'NONE',  ( 34.99999999999999289, -2.499999999999999556, 3.499999999999999556 ) ) ;
#16320 = CARTESIAN_POINT ( 'NONE',  ( 18.71249999999999858, 2.886751345948126879, 4.999999999999999112 ) ) ;
#16321 = CARTESIAN_POINT ( 'NONE',  ( 18.00937500061451502, 4.541064518000418104, -2.621784821874998173 ) ) ;
#16322 = CARTESIAN_POINT ( 'NONE',  ( 13.83750000122903323, 4.330127018922191873, 2.499999999999999556 ) ) ;
#16323 = CARTESIAN_POINT ( 'NONE',  ( 19.65000000000000213, 0.000000000000000000, 4.999999999999998224 ) ) ;
#16324 = CARTESIAN_POINT ( 'NONE',  ( -4.243569643749997233, 16.24062500061451431, -27.54997392385601174 ) ) ;
#16325 = CARTESIAN_POINT ( 'NONE',  ( -4.000000000000000888, 13.60624999877096641, 32.30940107675850470 ) ) ;
#16326 = CARTESIAN_POINT ( 'NONE',  ( 26.74687500061451573, -4.119189519843965641, -2.378215178125001383 ) ) ;
#16327 = CARTESIAN_POINT ( 'NONE',  ( 18.80625000122903501, 0.000000000000000000, 4.999999999999998224 ) ) ;
#16328 = CARTESIAN_POINT ( 'NONE',  ( 27.55312500061451786, 0.000000000000000000, 5.243569643749999010 ) ) ;
#16329 = CARTESIAN_POINT ( 'NONE',  ( 3.999999999999998668, 16.21250000000000213, -32.30940107675850470 ) ) ;
#16330 = CARTESIAN_POINT ( 'NONE',  ( 27.48749999999999716, -2.886751345948125991, -5.000000000000000000 ) ) ;
#16331 = CARTESIAN_POINT ( 'NONE',  ( 8.578125000614518214, 4.541064518000418104, 2.621784821874999949 ) ) ;
#16332 = CARTESIAN_POINT ( 'NONE',  ( 26.33437500061451431, -2.746126346562642428, -4.756430356249999214 ) ) ;
#16333 = CARTESIAN_POINT ( 'NONE',  ( 21.72187500061451715, 3.027376345333611329, 5.243569643749999010 ) ) ;
#16334 = CARTESIAN_POINT ( 'NONE',  ( 13.62187500061451750, -4.119189519843968306, 2.378215178124996054 ) ) ;
#16335 = CARTESIAN_POINT ( 'NONE',  ( 5.990625000614517859, -3.027376345333614438, 5.243569643749998122 ) ) ;
#16336 = CARTESIAN_POINT ( 'NONE',  ( 11.33437500061451608, 4.541064518000418104, 2.621784821874999949 ) ) ;
#16337 = ORIENTED_EDGE ( 'NONE', *, *, #24471, .F. ) ;
#16338 = CARTESIAN_POINT ( 'NONE',  ( 21.08437500061451786, 6.421520780324663323E-16, -5.243569643749999010 ) ) ;
#16339 = CARTESIAN_POINT ( 'NONE',  ( 2.679675080847534030, 4.226630133448150417, -27.01986178876142830 ) ) ;
#16340 = CARTESIAN_POINT ( 'NONE',  ( 29.21249999999999858, -5.773502691896255534, -1.060575238724906372E-15 ) ) ;
#16341 = CARTESIAN_POINT ( 'NONE',  ( 6.037500000000001421, 5.773502691896255534, 3.535250795749688894E-16 ) ) ;
#16342 = CARTESIAN_POINT ( 'NONE',  ( 14.85000000122903252, -2.886751345948129988, 4.999999999999997335 ) ) ;
#16343 = CARTESIAN_POINT ( 'NONE',  ( 2.000000000000001332, 15.20000000000000107, -26.53589838486224650 ) ) ;
#16344 = CARTESIAN_POINT ( 'NONE',  ( 3.786627597484739649, -3.265197691826910553, 4.102873032019218158 ) ) ;
#16345 = ORIENTED_EDGE ( 'NONE', *, *, #3608, .F. ) ;
#16346 = CARTESIAN_POINT ( 'NONE',  ( 11.70000000000000284, -4.330127018922190985, -2.500000000000001332 ) ) ;
#16347 = CARTESIAN_POINT ( 'NONE',  ( 17.06250000000000000, -5.773502691896255534, -1.060575238724906372E-15 ) ) ;
#16348 = CARTESIAN_POINT ( 'NONE',  ( 12.52500000122903145, 2.886751345948126879, 4.999999999999999112 ) ) ;
#16349 = CARTESIAN_POINT ( 'NONE',  ( 10.49062500061451431, -3.027376345333614438, 5.243569643749998122 ) ) ;
#16350 = CARTESIAN_POINT ( 'NONE',  ( 8.400000000000000355, 0.000000000000000000, 4.999999999999998224 ) ) ;
#16351 = FACE_OUTER_BOUND ( 'NONE', #7971, .T. ) ;
#16352 = CARTESIAN_POINT ( 'NONE',  ( 4.243569643749999010, 15.62187500061451928, -32.45002607614398471 ) ) ;
#16353 = CARTESIAN_POINT ( 'NONE',  ( 28.01250000122903216, -4.330127018922190985, -2.500000000000001332 ) ) ;
#16354 = CARTESIAN_POINT ( 'NONE',  ( -3.756430356250000102, 14.21562499938548285, 30.00000000000000000 ) ) ;
#16355 = CARTESIAN_POINT ( 'NONE',  ( 10.46249999999999858, 2.886751345948129099, -4.999999999999998224 ) ) ;
#16356 = DIRECTION ( 'NONE',  ( 1.000000000000000000, 0.000000000000000000, 0.000000000000000000 ) ) ;
#16357 = ORIENTED_EDGE ( 'NONE', *, *, #35944, .F. ) ;
#16358 = CARTESIAN_POINT ( 'NONE',  ( 24.92812500061451431, -4.541064518000419881, 2.621784821874995952 ) ) ;
#16359 = CARTESIAN_POINT ( 'NONE',  ( 3.578077538329305973, 3.492538166020475732, 3.745691089025586784 ) ) ;
#16360 = DIRECTION ( 'NONE',  ( 0.000000000000000000, 0.000000000000000000, 1.000000000000000000 ) ) ;
#16361 = CARTESIAN_POINT ( 'NONE',  ( 21.30937500061451573, 0.000000000000000000, 5.243569643749999010 ) ) ;
#16362 = CARTESIAN_POINT ( 'NONE',  ( 16.60312500061451857, 4.541064518000418104, -2.621784821874998173 ) ) ;
#16363 = CARTESIAN_POINT ( 'NONE',  ( 2.121784821875001281, 10.95312500061459460, -26.32496088578401938 ) ) ;
#16364 = CARTESIAN_POINT ( 'NONE',  ( 7.640625000614517326, 6.054752690667223547, 3.707466751127219781E-16 ) ) ;
#16365 = CARTESIAN_POINT ( 'NONE',  ( 29.40000000122903145, -2.886751345948125991, -5.000000000000000000 ) ) ;
#16366 = CARTESIAN_POINT ( 'NONE',  ( 24.08437500061451786, -4.119189519843968306, 2.378215178124996054 ) ) ;
#16367 = CARTESIAN_POINT ( 'NONE',  ( 18.62812500061451715, -4.541064518000419881, 2.621784821874995952 ) ) ;
#16368 = CARTESIAN_POINT ( 'NONE',  ( 9.084375000614517859, 4.119189519843966529, 2.378215178124999607 ) ) ;
#16369 = CARTESIAN_POINT ( 'NONE',  ( -7.967954043666661671E-16, 18.82812499938548356, 34.33755215474603517 ) ) ;
#16370 = CARTESIAN_POINT ( 'NONE',  ( 15.15937500061451715, -4.541064518000417216, -2.621784821875001281 ) ) ;
#16371 = CARTESIAN_POINT ( 'NONE',  ( 14.93437500061451750, 4.541064518000418104, 2.621784821874999949 ) ) ;
#16372 = CARTESIAN_POINT ( 'NONE',  ( 21.45937500061451786, -4.541064518000417216, -2.621784821875001281 ) ) ;
#16373 = ORIENTED_EDGE ( 'NONE', *, *, #59244, .F. ) ;
#16374 = CARTESIAN_POINT ( 'NONE',  ( -4.243569643749999898, 11.75937500061451857, 30.00000000000000000 ) ) ;
#16375 = CARTESIAN_POINT ( 'NONE',  ( 3.253125000614518036, 0.000000000000000000, 5.243569643749999010 ) ) ;
#16376 = CARTESIAN_POINT ( 'NONE',  ( 26.69062500061451715, -3.027376345333614438, 5.243569643749998122 ) ) ;
#16377 = EDGE_CURVE ( 'NONE', #14158, #53411, #26418, .T. ) ;
#16378 = CARTESIAN_POINT ( 'NONE',  ( 27.40312500061451573, 4.541064518000418104, -2.621784821874998173 ) ) ;
#16379 = CARTESIAN_POINT ( 'NONE',  ( 2.000000000000001332, 19.36250000122903359, -26.53589838486224650 ) ) ;
#16380 = CARTESIAN_POINT ( 'NONE',  ( -1.999999999999997113, 17.37500000000000000, 33.46410161513775705 ) ) ;
#16381 = CARTESIAN_POINT ( 'NONE',  ( 5.746875000614517504, -3.027376345333610441, -5.243569643749999898 ) ) ;
#16382 = CARTESIAN_POINT ( 'NONE',  ( 12.03750000122903430, 4.330127018922191873, 2.499999999999999556 ) ) ;
#16383 = CARTESIAN_POINT ( 'NONE',  ( 6.450000001229034829, -2.886751345948125991, -5.000000000000000000 ) ) ;
#16384 = CARTESIAN_POINT ( 'NONE',  ( 29.17500000122903714, 2.886751345948126879, 4.999999999999999112 ) ) ;
#16385 = CARTESIAN_POINT ( 'NONE',  ( 4.000000000000000000, 19.23124999877096641, 27.69059892324149530 ) ) ;
#16386 = CARTESIAN_POINT ( 'NONE',  ( 18.84375000122903288, -2.886751345948129988, 4.999999999999997335 ) ) ;
#16387 = CARTESIAN_POINT ( 'NONE',  ( 11.33437500061451608, 4.541064518000418104, 2.621784821874999949 ) ) ;
#16388 = ORIENTED_EDGE ( 'NONE', *, *, #50186, .T. ) ;
#16389 = CARTESIAN_POINT ( 'NONE',  ( 20.09062500061451573, -3.027376345333610441, -5.243569643749999898 ) ) ;
#16390 = CARTESIAN_POINT ( 'NONE',  ( 13.62187500061451750, 3.027376345333611329, 5.243569643749999010 ) ) ;
#16391 = CARTESIAN_POINT ( 'NONE',  ( 4.940625000614515372, 6.054752690667223547, 3.707466751127219781E-16 ) ) ;
#16392 = EDGE_CURVE ( 'NONE', #72350, #55885, #65268, .T. ) ;
#16393 = CARTESIAN_POINT ( 'NONE',  ( 21.08437500061451786, 6.421520780324663323E-16, -5.243569643749999010 ) ) ;
#16394 = CARTESIAN_POINT ( 'NONE',  ( 10.43437500061451750, 4.541064518000418104, 2.621784821874999949 ) ) ;
#16395 = CARTESIAN_POINT ( 'NONE',  ( 4.453125000614517326, 4.541064518000418104, -2.621784821874998173 ) ) ;
#16396 = CARTESIAN_POINT ( 'NONE',  ( 10.91250000122903252, -4.330127018922190985, -2.500000000000001332 ) ) ;
#16397 = CARTESIAN_POINT ( 'NONE',  ( 5.137500001229033941, 6.123233995736764310E-16, -4.999999999999998224 ) ) ;
#16398 = CARTESIAN_POINT ( 'NONE',  ( 19.19062500061452070, -3.027376345333610441, -5.243569643749999898 ) ) ;
#16399 = EDGE_CURVE ( 'NONE', #860, #48144, #21899, .T. ) ;
#16400 = CARTESIAN_POINT ( 'NONE',  ( 7.500000001229034652, 5.773502691896255534, 3.535250795749688894E-16 ) ) ;
#16401 = CARTESIAN_POINT ( 'NONE',  ( 16.15312500061451573, 4.541064518000418104, -2.621784821874998173 ) ) ;
#16402 = CARTESIAN_POINT ( 'NONE',  ( 15.77812500061451573, 4.541064518000418104, 2.621784821874999949 ) ) ;
#16403 = CARTESIAN_POINT ( 'NONE',  ( 25.47187500061451715, -5.492252693125287522, -1.008910452111647106E-15 ) ) ;
#16404 = CARTESIAN_POINT ( 'NONE',  ( 16.64999999999999858, -4.330127018922190985, -2.500000000000001332 ) ) ;
#16405 = CARTESIAN_POINT ( 'NONE',  ( 9.600000001229034297, -2.886751345948125991, -5.000000000000000000 ) ) ;
#16406 = CARTESIAN_POINT ( 'NONE',  ( 9.028125000614517504, 4.541064518000418104, 2.621784821874999949 ) ) ;
#16407 = EDGE_CURVE ( 'NONE', #403, #31197, #7963, .T. ) ;
#16408 = CARTESIAN_POINT ( 'NONE',  ( 21.37500000122902932, 2.886751345948129099, -4.999999999999998224 ) ) ;
#16409 = CARTESIAN_POINT ( 'NONE',  ( 26.81250000000000000, 2.886751345948126879, 4.999999999999999112 ) ) ;
#16410 = CARTESIAN_POINT ( 'NONE',  ( 4.243569643749999010, 12.47187500061451715, -32.45002607614398471 ) ) ;
#16411 = CARTESIAN_POINT ( 'NONE',  ( 4.615679581435968792, -1.922694556504207286, 4.852467576076502809 ) ) ;
#16412 = DIRECTION ( 'NONE',  ( 0.000000000000000000, 0.000000000000000000, -1.000000000000000000 ) ) ;
#16413 = CARTESIAN_POINT ( 'NONE',  ( 2.896875000614518747, -3.027376345333614438, 5.243569643749998122 ) ) ;
#16414 = CARTESIAN_POINT ( 'NONE',  ( 20.37187500061451573, 3.027376345333611329, 5.243569643749999010 ) ) ;
#16415 = CARTESIAN_POINT ( 'NONE',  ( 1.626862140677534273E-15, 16.51249999999999929, -26.00000000000000355 ) ) ;
#16416 = CARTESIAN_POINT ( 'NONE',  ( 16.79062500061451857, -3.027376345333614438, 5.243569643749998122 ) ) ;
#16417 = CARTESIAN_POINT ( 'NONE',  ( 11.98125000122903394, 4.330127018922191873, 2.499999999999999556 ) ) ;
#16418 = CARTESIAN_POINT ( 'NONE',  ( 29.33437500061451431, 4.541064518000418104, 2.621784821874999949 ) ) ;
#16419 = CARTESIAN_POINT ( 'NONE',  ( 19.92187500061451289, -4.119189519843968306, 2.378215178124996054 ) ) ;
#16420 = CARTESIAN_POINT ( 'NONE',  ( 14.95312500061451644, 0.000000000000000000, 5.243569643749999010 ) ) ;
#16421 = CARTESIAN_POINT ( 'NONE',  ( 11.07187500061451679, -6.054752690667223547, -1.112240025338166033E-15 ) ) ;
#16422 = ORIENTED_EDGE ( 'NONE', *, *, #74, .F. ) ;
#16423 = CARTESIAN_POINT ( 'NONE',  ( -3.999999999999999112, 14.15000000000000036, -30.00000000000000000 ) ) ;
#16424 = CARTESIAN_POINT ( 'NONE',  ( 23.72812500061451502, 6.421520780324663323E-16, -5.243569643749999010 ) ) ;
#16425 = PLANE ( 'NONE',  #32178 ) ;
#16426 = DIRECTION ( 'NONE',  ( -1.000000000000000000, -0.000000000000000000, -0.000000000000000000 ) ) ;
#16427 = CARTESIAN_POINT ( 'NONE',  ( 12.82499999999999929, 4.330127018922191873, 2.499999999999999556 ) ) ;
#16428 = CARTESIAN_POINT ( 'NONE',  ( 22.05000000122903714, -2.886751345948129988, 4.999999999999997335 ) ) ;
#16429 = CARTESIAN_POINT ( 'NONE',  ( 16.30312500061451786, 0.000000000000000000, 5.243569643749999010 ) ) ;
#16430 = CARTESIAN_POINT ( 'NONE',  ( 11.74687500061451573, 0.000000000000000000, 4.756430356249998326 ) ) ;
#16431 = VERTEX_POINT ( 'NONE', #55232 ) ;
#16432 = CARTESIAN_POINT ( 'NONE',  ( 19.61249999999999716, 2.886751345948126879, 4.999999999999999112 ) ) ;
#16433 =( BOUNDED_CURVE ( )  B_SPLINE_CURVE ( 2, ( #12305, #34840, #40761, #67750, #57367, #56302, #29307 ),
 .UNSPECIFIED., .F., .F. ) 
 B_SPLINE_CURVE_WITH_KNOTS ( ( 3, 2, 2, 3 ),
 ( 0.8500000000000001998, 0.8533333333333336101, 0.8566666666666669094, 0.8600000000000002087 ),
 .UNSPECIFIED. ) 
 CURVE ( )  GEOMETRIC_REPRESENTATION_ITEM ( )  RATIONAL_B_SPLINE_CURVE ( ( 0.9999999999999911182, 0.8660254037844475894, 1.000000000000000000, 0.8660254037844387076, 1.000000000000000000, 0.8660254037844298258, 1.000000000000008882 ) ) 
 REPRESENTATION_ITEM ( '' )  );
#16434 = CARTESIAN_POINT ( 'NONE',  ( 20.70937500061451786, 4.541064518000418104, -2.621784821874998173 ) ) ;
#16435 = CARTESIAN_POINT ( 'NONE',  ( 26.76562500061451644, -6.054752690667223547, -1.112240025338166033E-15 ) ) ;
#16436 = ORIENTED_EDGE ( 'NONE', *, *, #1440, .F. ) ;
#16437 = CARTESIAN_POINT ( 'NONE',  ( 21.09375000122903288, -2.886751345948130876, 4.999999999999996447 ) ) ;
#16438 = CARTESIAN_POINT ( 'NONE',  ( 10.00312500061451715, 0.000000000000000000, 5.243569643749999010 ) ) ;
#16439 = CARTESIAN_POINT ( 'NONE',  ( 6.187500000000001776, -2.886751345948130876, 4.999999999999996447 ) ) ;
#16440 = CARTESIAN_POINT ( 'NONE',  ( 16.46249999999999503, 2.886751345948126879, 4.999999999999999112 ) ) ;
#16441 = CARTESIAN_POINT ( 'NONE',  ( 23.36250000000000071, -5.773502691896255534, -1.060575238724906372E-15 ) ) ;
#16442 = CARTESIAN_POINT ( 'NONE',  ( 2.121784821875001281, 19.50312500061451360, 33.67503911421598417 ) ) ;
#16443 = CARTESIAN_POINT ( 'NONE',  ( 4.471875000614518925, 3.027376345333613106, -5.243569643749998122 ) ) ;
#16444 = CARTESIAN_POINT ( 'NONE',  ( 29.74687500061451217, 6.054752690667223547, 3.707466751127219781E-16 ) ) ;
#16445 = ORIENTED_EDGE ( 'NONE', *, *, #36482, .T. ) ;
#16446 = CARTESIAN_POINT ( 'NONE',  ( 23.54062500061451146, -3.027376345333614438, 5.243569643749998122 ) ) ;
#16447 = CARTESIAN_POINT ( 'NONE',  ( 25.32187500061451857, 3.027376345333611329, 5.243569643749999010 ) ) ;
#16448 = CARTESIAN_POINT ( 'NONE',  ( 9.001249775931846008E-16, 19.46562500061459033, -25.09994784771203058 ) ) ;
#16449 = CARTESIAN_POINT ( 'NONE',  ( 13.87500000000000178, -4.330127018922194537, 2.499999999999995559 ) ) ;
#16450 = CARTESIAN_POINT ( 'NONE',  ( 9.215625000614515727, -6.054752690667223547, -1.112240025338166033E-15 ) ) ;
#16451 = CARTESIAN_POINT ( 'NONE',  ( 0.6522972858965978560, 20.64114861271052348, 33.69936173848522998 ) ) ;
#16452 = CARTESIAN_POINT ( 'NONE',  ( 25.41562500061451146, -6.054752690667223547, -1.112240025338166033E-15 ) ) ;
#16453 = CARTESIAN_POINT ( 'NONE',  ( 12.63750000122903394, -4.330127018922194537, 2.499999999999995559 ) ) ;
#16454 = CARTESIAN_POINT ( 'NONE',  ( 15.19687500061451857, -2.746126346562642428, -4.756430356249999214 ) ) ;
#16455 = CARTESIAN_POINT ( 'NONE',  ( 3.740625000614516527, -3.027376345333614438, 5.243569643749998122 ) ) ;
#16456 = CARTESIAN_POINT ( 'NONE',  ( 19.84687500061451360, 6.054752690667223547, 3.707466751127219781E-16 ) ) ;
#16457 = CARTESIAN_POINT ( 'NONE',  ( 4.243569643749999898, 13.78437500061451715, 30.00000000000000000 ) ) ;
#16458 = CARTESIAN_POINT ( 'NONE',  ( 22.65937500061451715, 0.000000000000000000, 5.243569643749999010 ) ) ;
#16459 = CARTESIAN_POINT ( 'NONE',  ( 28.43437500061451573, 4.541064518000418104, 2.621784821874999949 ) ) ;
#16460 = CARTESIAN_POINT ( 'NONE',  ( 4.243569643749999898, 19.18437500061451928, 30.00000000000000000 ) ) ;
#16461 = CARTESIAN_POINT ( 'NONE',  ( 10.75312500061451715, 4.541064518000418104, -2.621784821874998173 ) ) ;
#16462 = CARTESIAN_POINT ( 'NONE',  ( -3.999999999999999112, 15.12500000122903465, 27.69059892324149885 ) ) ;
#16463 = CARTESIAN_POINT ( 'NONE',  ( 7.171875000614517326, 3.027376345333613106, -5.243569643749998122 ) ) ;
#16464 = CARTESIAN_POINT ( 'NONE',  ( 13.03125000122903110, -4.330127018922194537, 2.499999999999995559 ) ) ;
#16465 = CARTESIAN_POINT ( 'NONE',  ( 8.090625000614515727, 6.054752690667223547, 3.707466751127219781E-16 ) ) ;
#16466 = CARTESIAN_POINT ( 'NONE',  ( 12.04687500061451821, -3.027376345333610441, -5.243569643749999898 ) ) ;
#16467 = CARTESIAN_POINT ( 'NONE',  ( 19.12500000122903288, 2.886751345948129099, -4.999999999999998224 ) ) ;
#16468 = CARTESIAN_POINT ( 'NONE',  ( 8.071875000614518569, 3.027376345333613106, -5.243569643749998122 ) ) ;
#16469 = EDGE_CURVE ( 'NONE', #41395, #4055, #72843, .T. ) ;
#16470 = CARTESIAN_POINT ( 'NONE',  ( 9.590625000614517504, -3.027376345333614438, 5.243569643749998122 ) ) ;
#16471 = CARTESIAN_POINT ( 'NONE',  ( 4.875318576323432573, 3.418657702705165669, -4.565850452727954867 ) ) ;
#16472 = CARTESIAN_POINT ( 'NONE',  ( 25.78125000122903288, 6.123233995736764310E-16, -4.999999999999998224 ) ) ;
#16473 = CARTESIAN_POINT ( 'NONE',  ( 19.13437500061451857, -4.541064518000419881, 2.621784821874995952 ) ) ;
#16474 = CARTESIAN_POINT ( 'NONE',  ( 18.11250000000000071, 2.886751345948129099, -4.999999999999997335 ) ) ;
#16475 = CARTESIAN_POINT ( 'NONE',  ( 27.70312500061451289, -4.541064518000417216, -2.621784821875001281 ) ) ;
#16476 = CARTESIAN_POINT ( 'NONE',  ( 11.27812500061451573, 4.541064518000418104, 2.621784821874999949 ) ) ;
#16477 = CARTESIAN_POINT ( 'NONE',  ( -5.000000000000004441, 0.000000000000000000, 4.999999999999998224 ) ) ;
#16478 = CARTESIAN_POINT ( 'NONE',  ( -4.243569643749998122, 13.14687500061451786, -27.54997392385601174 ) ) ;
#16479 = CARTESIAN_POINT ( 'NONE',  ( 12.90000000122903145, 5.773502691896255534, 3.535250795749688894E-16 ) ) ;
#16480 = CARTESIAN_POINT ( 'NONE',  ( 27.10312500061451502, 0.000000000000000000, 5.243569643749999010 ) ) ;
#16481 = EDGE_CURVE ( 'NONE', #61496, #70526, #19498, .T. ) ;
#16482 = CARTESIAN_POINT ( 'NONE',  ( -3.000416591977282496E-16, 16.54062500061451857, -34.90005215228797653 ) ) ;
#16483 = CARTESIAN_POINT ( 'NONE',  ( 14.47500000122903430, -5.773502691896255534, -1.060575238724906372E-15 ) ) ;
#16484 = CARTESIAN_POINT ( 'NONE',  ( 13.38750000000000107, -2.886751345948129988, 4.999999999999997335 ) ) ;
#16485 = CARTESIAN_POINT ( 'NONE',  ( 23.98125000122903216, 6.123233995736764310E-16, -4.999999999999998224 ) ) ;
#16486 = CARTESIAN_POINT ( 'NONE',  ( 22.22812500061451502, -4.541064518000419881, 2.621784821874995952 ) ) ;
#16487 = CARTESIAN_POINT ( 'NONE',  ( 8.559375000614515727, 4.541064518000418104, -2.621784821874998173 ) ) ;
#16488 = CARTESIAN_POINT ( 'NONE',  ( 9.712500001229033231, 4.330127018922192761, -2.499999999999997780 ) ) ;
#16489 = CARTESIAN_POINT ( 'NONE',  ( 18.63750000122903216, 6.123233995736764310E-16, -4.999999999999998224 ) ) ;
#16490 =( BOUNDED_CURVE ( )  B_SPLINE_CURVE ( 2, ( #66691, #16065, #38614, #61137, #9072, #31607, #3538 ),
 .UNSPECIFIED., .F., .F. ) 
 B_SPLINE_CURVE_WITH_KNOTS ( ( 3, 2, 2, 3 ),
 ( 0.2833333333333333814, 0.2861111111111111494, 0.2888888888888889173, 0.2916666666666667407 ),
 .UNSPECIFIED. ) 
 CURVE ( )  GEOMETRIC_REPRESENTATION_ITEM ( )  RATIONAL_B_SPLINE_CURVE ( ( 0.9999999999999973355, 0.8660254037844413721, 1.000000000000000000, 0.8660254037844387076, 1.000000000000000000, 0.8660254037844360431, 1.000000000000002665 ) ) 
 REPRESENTATION_ITEM ( '' )  );
#16491 = CARTESIAN_POINT ( 'NONE',  ( 14.46562500061451750, 3.027376345333611329, 5.243569643749999010 ) ) ;
#16492 = CARTESIAN_POINT ( 'NONE',  ( 17.69062500061451715, -3.027376345333614438, 5.243569643749998122 ) ) ;
#16493 = CARTESIAN_POINT ( 'NONE',  ( 24.97500000122903430, 2.886751345948129099, -4.999999999999998224 ) ) ;
#16494 =( BOUNDED_CURVE ( )  B_SPLINE_CURVE ( 2, ( #46075, #40174, #18695, #6184, #41259, #68251, #35339, #62333, #28713 ),
 .UNSPECIFIED., .F., .F. ) 
 B_SPLINE_CURVE_WITH_KNOTS ( ( 3, 2, 2, 2, 3 ),
 ( 0.4239130434782608647, 0.4275362318840579823, 0.4347826086956521618, 0.4420289855072463969, 0.4456521739130435145 ),
 .UNSPECIFIED. ) 
 CURVE ( )  GEOMETRIC_REPRESENTATION_ITEM ( )  RATIONAL_B_SPLINE_CURVE ( ( 0.9330127018922194093, 0.9330127018922194093, 1.000000000000000000, 0.8660254037844387076, 1.000000000000000000, 0.8660254037844387076, 1.000000000000000000, 0.9330127018922188542, 0.9330127018922194093 ) ) 
 REPRESENTATION_ITEM ( '' )  );
#16495 = CARTESIAN_POINT ( 'NONE',  ( 28.46250000122903145, -4.330127018922190985, -2.500000000000001332 ) ) ;
#16496 = CARTESIAN_POINT ( 'NONE',  ( 22.42500000000000071, -4.330127018922194537, 2.499999999999995559 ) ) ;
#16497 = CARTESIAN_POINT ( 'NONE',  ( 2.655984681222220721E-16, 13.65312499938548463, 25.66244784525396483 ) ) ;
#16498 = CARTESIAN_POINT ( 'NONE',  ( 25.13437500061451502, 6.421520780324663323E-16, -5.243569643749999010 ) ) ;
#16499 = DIRECTION ( 'NONE',  ( -1.000000000000000000, -0.000000000000000000, -0.000000000000000000 ) ) ;
#16500 = PRODUCT_RELATED_PRODUCT_CATEGORY ( 'part', '', ( #45592 ) ) ;
#16501 = CARTESIAN_POINT ( 'NONE',  ( 11.36250000122903536, -4.330127018922190985, -2.500000000000001332 ) ) ;
#16502 = CARTESIAN_POINT ( 'NONE',  ( 28.13437500061451502, -4.541064518000419881, 2.621784821874995952 ) ) ;
#16503 = DIRECTION ( 'NONE',  ( 0.000000000000000000, 0.000000000000000000, 1.000000000000000000 ) ) ;
#16504 =( BOUNDED_SURFACE ( )  B_SPLINE_SURFACE ( 1, 2, ( 
 ( #32700, #32327, #55596, #49330, #50425, #55237, #10529, #21602, #61132, #60386, #10889, #10166, #67061, #56325, #16418, #38976, #61492, #33417, #72586, #11260, #27891, #38609, #44156, #50781, #27162, #66685, #16060, #33057, #4991, #72951, #27523, #50056, #15325, #21234, #39340, #55957, #4272, #54864, #67420, #21969, #22333, #71862, #60758, #5353, #15690, #37867, #44528, #28250, #44885, #16782, #26796, #61852, #33782, #5714, #20871, #43424, #65946, #9794, #43786, #66313, #38228, #4632, #49696, #72223, #28606, #18214, #40066, #57028, #63658, #57391, #23052, #45962, #51507, #184, #56675, #11977, #6434, #28969, #40418, #6073, #68495, #62580, #51142, #907, #24135, #34500, #62935, #541, #12692, #67773, #68858, #46323, #17148, #12328, #35588, #45607, #1264, #69224, #34864, #18585, #17859, #23415, #39706, #29687, #6798, #29332, #63300, #51862, #23771, #40787, #30045, #46686, #41150, #13049, #35229, #57750, #7158, #11620, #58107, #52224, #62224, #7514, #22689, #1628, #45240, #34136, #68141, #17505, #25602, #14878, #25968, #42959, #47046, #36321, #36680, #70664, #59940, #37417, #71036, #9347, #65121, #24859, #53307, #14511, #20040, #52585, #48140, #69580, #47406, #65488, #13779, #47768, #30776, #24502, #35947, #59201, #41859, #8609, #58836, #19306, #13400, #1991, #52945, #53679, #8246, #42595, #31514, #54055, #18942, #37044, #70304, #41501, #19677, #58468, #20411, #2342, #64021, #59568, #8982, #31138, #69936, #2706, #25222, #30417, #7881, #42230, #14145, #64389, #3450, #64755, #3074, #48509, #60665, #72132, #22247, #4545, #10800, #60297, #21146, #49605, #43700, #54775, #20780, #61406, #66221, #21512, #43336, #4903, #10078, #4180, #15599, #44065, #33335, #27074, #38141, #39252, #66593, #16333, #44801, #15969, #71778, #44439, #49243, #16694, #27439, #72493, #38519, #49969, #38888, #61042, #26336, #21878, #71405, #9708, #32609, #65858, #10440, #32242, #55873, #55147, #32970, #55510, #66968, #15240, #5260, #27804, #50340, #67334, #72864, #61764, #31880, #54414, #3815, #48875, #37777, #26709, #18498, #22959, #52137, #1540, #39616, #50694, #6345, #5985, #62850, #17769, #5630, #51415, #40329, #68050, #12244, #34775, #51777, #34413, #57307, #56941, #450, #62135, #39978, #35143, #51055, #817, #17057, #23685, #28167, #6712, #29245, #96, #23325, #46597, #34049, #1177, #7072, #45875, #29601, #28876, #45519, #22602, #40696, #46233, #68773, #18129, #17419, #68407, #62490, #41063, #57666, #24050, #69139, #63213, #12609, #11168, #45154, #33692, #56238, #67686, #11528, #56589, #28515, #11888, #41773, #25137, #2616, #36595, #25885, #36960, #53966, #58021, #47319, #47678, #8523, #70951, #48425, #8894, #20322, #2984, #35859, #64302, #25512, #31052, #63577, #59116, #3364, #70582, #8159, #13691, #12964, #69852, #36235, #58749, #30688, #70214, #19958, #53219, #19588, #7431, #63935, #31426, #48057, #46962, #1908, #59482, #42144, #65034, #41419, #30333, #53589, #58382, #29957, #64671, #35502, #14056, #42510, #24413, #14425, #52498, #69498, #18858, #13320, #7794, #52861, #2261, #24775, #19219, #66136, #20691, #4818, #71315, #60952, #9625, #26623, #33249, #26992, #65770, #15514, #21063, #42876, #26251, #54691, #49160, #71691, #9989, #48788, #38056, #21789, #43250, #32158, #60581, #4094, #15152, #31794, #72407, #43614, #32524, #54333, #15884, #55061, #37689, #4462, #49521, #44355, #72046, #21424, #50254, #43981, #27351, #55787, #66502, #38429, #55425, #60212, #27714, #10355, #32885, #49882, #66880, #16248, #38804, #37331, #61320, #9259, #10717, #5178, #3726, #72777, #65399, #14790, #59855, #11807, #22871, #62408, #61678, #12161, #11446, #68328, #57586, #17688, #40249, #62770, #34689, #733, #29162, #67963, #57220, #29520, #33966, #63130, #12526, #50609, #11077, #17336, #16969, #23242, #28790, #16607, #34324, #51331, #5898, #45793, #6633, #51694, #45429, #1098, #39163, #67604, #35059, #56505, #39895, #364, #67249, #5543, #6262, #28431, #23606, #50968, #62051, #56149, #44713, #22520, #46151, #56856, #68691, #18051, #40609, #33605, #6989, #52055, #28081, #22161, #13, #45067, #39525, #1459, #8432, #64584, #30607, #1822, #35777, #58300, #52414, #42427, #7709, #36148, #69052, #53503, #7348, #30243, #19504, #52776, #41690, #64948, #8075, #53135, #13972, #2178, #47235, #24691, #31338, #25426, #19874, #14340, #13602, #2534, #47597, #12883, #36874, #25054, #18414, #59392, #47969, #69768, #8802, #19136, #58667, #70126, #42061, #23965, #70497, #46513, #40980, #64213, #36510, #59030, #63495, #35416, #57941, #29878, #30968, #46878, #2895, #24329, #69417, #18772, #41338, #63848, #13239, #71599, #54603, #10632, #60128, #26531, #4008, #20974, #37971, #10269, #43527, #66049, #48337, #54241, #72325, #15797, #37243, #65309, #27267, #60492, #55338, #31706, #20602, #49432, #48701, #70862, #9898, #61238, #15427, #32434, #14699, #49071, #4733, #54971, #32802, #4377, #26906, #71966, #3271, #20236, #49800, #21340, #3638, #38337, #9171, #43895, #43161, #37606, #44262, #66419, #26162, #60866, #32071, #53879, #59764, #65681, #9537, #21705, #66795, #71224, #16166, #15069, #38718, #25799, #42788, #73053, #283, #39076, #45710, #27630, #28706, #6176, #50163, #22791, #68603, #56063, #34238, #29076, #45344, #51611, #28346, #22435, #72693, #62686, #12082, #39810, #62326, #23156, #39439, #5815, #16885, #63041, #57132, #1011, #23518, #67878, #11722, #51245, #44634, #46068, #56772, #22075, #17964, #6542, #50883, #40525, #11363, #17250, #648, #68244, #33162, #55700, #5094, #67163, #61959, #17607, #40167, #16524, #61593, #10994, #33514, #34603, #5456, #33881, #27996, #50525, #44983, #67520, #56426, #19415, #30155, #13152, #42340, #18688, #58214, #35694, #52689, #69685, #41975, #2095, #24605, #6904, #12796, #30879, #47513, #68966 ),
 ( #47153, #34973, #29435, #13888, #7619, #63410, #70042, #40896, #30524, #52329, #69329, #2811, #19050, #35332, #41608, #63763, #12440, #18323, #24244, #41252, #64127, #13513, #57855, #36060, #1731, #7264, #58580, #36428, #46793, #7988, #29793, #24968, #51972, #53051, #2445, #1371, #64496, #47884, #58942, #8350, #53420, #25339, #70413, #19789, #57502, #23881, #46428, #42703, #33706, #26076, #26445, #59305, #44814, #70773, #71140, #9815, #20513, #31985, #56253, #37523, #67348, #20149, #54158, #9455, #3554, #14615, #53789, #22261, #48615, #54519, #3185, #37886, #43070, #37154, #65596, #3922, #16710, #60044, #14985, #111, #48985, #49351, #5644, #71514, #31624, #4291, #9087, #50708, #60406, #32347, #20890, #54885, #72879, #43444, #8716, #26817, #31248, #65225, #65966, #25712, #15346, #59679, #39266, #61778, #11182, #28180, #22617, #48249, #64863, #14251, #36790, #7445, #18143, #40710, #12622, #57681, #23699, #52151, #17783, #7086, #52512, #56955, #12979, #35516, #466, #11545, #40342, #39991, #46247, #51790, #39631, #12258, #1191, #28891, #68787, #63228, #35157, #68421, #29615, #62149, #17433, #58035, #6359, #62863, #23340, #17071, #28530, #29260, #34427, #1554, #51430, #11902, #5999, #67699, #45536, #24064, #832, #46610, #69153, #18512, #34062, #41077, #34789, #56603, #57322, #51068, #29971, #68065, #45168, #63591, #1922, #22974, #62504, #45889, #6726, #59868, #36972, #69865, #25151, #59495, #65048, #24427, #70594, #14802, #31439, #42157, #47691, #54345, #30700, #70227, #19601, #64684, #8536, #53979, #14069, #36608, #18871, #24788, #42889, #8908, #7809, #35872, #70963, #31065, #25898, #2272, #64315, #19969, #19231, #41433, #53603, #31807, #59129, #2997, #58396, #25525, #48438, #48068, #3377, #42522, #14438, #20336, #46976, #63949, #65412, #37345, #47332, #9272, #52874, #69511, #13705, #8172, #13334, #30346, #41785, #36248, #2629, #58762, #53232, #15528, #60594, #32538, #43995, #9638, #49535, #66150, #32172, #55075, #27730, #43628, #66517, #54705, #16264, #71330, #72422, #49897, #20705, #15897, #39177, #26638, #4832, #72793, #38444, #22176, #72059, #38070, #43263, #33264, #10370, #32900, #66896, #10003, #21438, #4475, #33620, #50268, #44729, #67264, #60970, #55440, #21805, #15166, #16622, #27366, #65784, #61693, #11092, #44369, #3739, #27005, #38819, #61334, #10732, #26264, #48801, #37703, #60224, #55802, #5192, #4110, #49174, #71705, #21077, #62065, #68705, #50623, #51709, #29175, #28, #45806, #18429, #5912, #57233, #52069, #68342, #1474, #51345, #45444, #22534, #12540, #62784, #12176, #46165, #62422, #28804, #39909, #12898, #7003, #23980, #46528, #17702, #34704, #1112, #67617, #69070, #6648, #45081, #40995, #29534, #747, #63511, #34338, #40263, #23619, #18065, #56164, #5558, #28095, #16983, #11821, #40626, #63145, #39540, #11459, #33980, #56519, #35074, #28446, #56872, #57600, #50981, #378, #22886, #67977, #17350, #23256, #6276, #65327, #41705, #8091, #58681, #2550, #19520, #64966, #25069, #47612, #29892, #35791, #53897, #70515, #18788, #46893, #8819, #42078, #36892, #13253, #2193, #30986, #30259, #52431, #64600, #42805, #70142, #13987, #69431, #30621, #59411, #36526, #14357, #59046, #53151, #8450, #57955, #1837, #31356, #53519, #58314, #19891, #63863, #2913, #24707, #19151, #25816, #25444, #7725, #47987, #13618, #35431, #41353, #47251, #64229, #36163, #42444, #52792, #3288, #69784, #48354, #70879, #20253, #7363, #24345, #4394, #15443, #54988, #54259, #4749, #4024, #60882, #50181, #10287, #32817, #55355, #27283, #66435, #21721, #60509, #49816, #22092, #26549, #55716, #5111, #43179, #3655, #9915, #9553, #15813, #21355, #9188, #26923, #43911, #71618, #38355, #72340, #44280, #37987, #66811, #31723, #60144, #27645, #49090, #32453, #66065, #59782, #71241, #71982, #20991, #16183, #43544, #54618, #48719, #37260, #15085, #38734, #49448, #61254, #10648, #33178, #26178, #72709, #44650, #20621, #14718, #65698, #37622, #32087, #67180, #1029, #57149, #23172, #67537, #28363, #50899, #45000, #34991, #299, #28721, #61611, #46085, #73070, #22808, #12098, #45360, #34255, #57520, #39828, #68621, #22451, #56441, #11738, #5831, #16900, #56083, #23535, #67894, #56788, #5475, #40183, #17266, #39455, #62343, #6193, #17983, #51262, #664, #1389, #45726, #51629, #6921, #68261, #33897, #6561, #11378, #51988, #62704, #34619, #17624, #29093, #40542, #63058, #11012, #12460, #33533, #61976, #29451, #28014, #23898, #16541, #39094, #50542, #40915, #36080, #8734, #69349, #47533, #42361, #58601, #64883, #41626, #35712, #12815, #2831, #53070, #2465, #36448, #52708, #19070, #30177, #3204, #70433, #14271, #36809, #8008, #24988, #19435, #57873, #59324, #70061, #63428, #31268, #19808, #64146, #53810, #24625, #30543, #41996, #64516, #46446, #68984, #18341, #35349, #2114, #13909, #58962, #7283, #29812, #52347, #1750, #8370, #18707, #47172, #30898, #53440, #24263, #25359, #46812, #47904, #13533, #69704, #41271, #63783, #13172, #58234, #7639, #9836, #55274, #65985, #37907, #20169, #26096, #44196, #60796, #9106, #37173, #72261, #32365, #27199, #3573, #65615, #21273, #20531, #42723, #54903, #33095, #15365, #60425, #59699, #49003, #49734, #4311, #4669, #49370, #71534, #43461, #48270, #65244, #21638, #20909, #48634, #10201, #54176, #43827, #15004, #9474, #16098, #26836, #71159, #71900, #3941, #25732, #31644, #37541, #32004, #54539, #66351, #43088, #15729, #60063, #26464, #38268, #66727, #32737, #38648, #61172, #10567, #14633, #55634, #70794, #22370, #67812, #50461, #50818, #67097, #10926, #44922, #33453, #16455, #72627, #221, #55997, #67458, #22011, #11299, #27928, #39013, #5390, #16821, #22726, #72988, #39375, #39746, #61894, #28287, #17186, #33819, #56363, #5753, #61528, #62262, #45279, #5027, #27565 ) ),
 .UNSPECIFIED., .F., .F., .T. ) 
 B_SPLINE_SURFACE_WITH_KNOTS ( ( 2, 2 ),
 ( 3, 2, 2, 2, 2, 2, 2, 2, 2, 2, 2, 2, 2, 2, 2, 2, 2, 2, 2, 2, 2, 2, 2, 2, 2, 2, 2, 2, 2, 2, 2, 2, 2, 2, 2, 2, 2, 2, 2, 2, 2, 2, 2, 2, 2, 2, 2, 2, 2, 2, 2, 2, 2, 2, 2, 2, 2, 2, 2, 2, 2, 2, 2, 2, 2, 2, 2, 2, 2, 2, 2, 2, 2, 2, 2, 2, 2, 2, 2, 2, 2, 2, 2, 2, 2, 2, 2, 2, 2, 2, 2, 2, 2, 2, 2, 2, 2, 2, 2, 2, 2, 2, 2, 2, 2, 2, 2, 2, 2, 2, 2, 2, 2, 2, 2, 2, 2, 2, 2, 2, 2, 2, 2, 2, 2, 2, 2, 2, 2, 2, 2, 2, 2, 2, 2, 2, 2, 2, 2, 2, 2, 2, 2, 2, 2, 2, 2, 2, 2, 2, 2, 2, 2, 2, 2, 2, 2, 2, 2, 2, 2, 2, 2, 2, 2, 2, 2, 2, 2, 2, 2, 2, 2, 2, 2, 2, 2, 2, 2, 2, 2, 2, 2, 2, 2, 2, 2, 2, 2, 2, 2, 2, 2, 2, 2, 2, 2, 2, 2, 2, 2, 2, 2, 2, 2, 2, 2, 2, 2, 2, 2, 2, 2, 2, 2, 2, 2, 2, 2, 2, 2, 2, 2, 2, 2, 2, 2, 2, 2, 2, 2, 2, 2, 2, 2, 2, 2, 2, 2, 2, 2, 2, 2, 2, 2, 2, 2, 2, 2, 2, 2, 2, 2, 2, 2, 2, 2, 2, 2, 2, 2, 2, 2, 2, 2, 2, 2, 2, 2, 2, 2, 2, 2, 2, 2, 2, 2, 2, 2, 2, 2, 2, 2, 2, 2, 2, 2, 2, 2, 2, 2, 2, 2, 2, 2, 2, 2, 2, 2, 2, 2, 2, 2, 2, 2, 2, 2, 2, 2, 2, 2, 2, 2, 2, 2, 2, 2, 2, 2, 2, 2, 2, 2, 2, 2, 2, 2, 2, 2, 2, 2, 2, 2, 2, 2, 2, 2, 2, 2, 2, 2, 2, 2, 2, 2, 2, 2, 2, 2, 2, 2, 2, 2, 2, 2, 2, 2, 2, 2, 2, 3 ),
 ( 0.000000000000000000, 1.000000000000000000 ),
 ( 0.000000000000000000, 0.002777777777777777884, 0.005555555555555555768, 0.008333333333333333218, 0.01111111111111111154, 0.01388888888888888812, 0.01666666666666666644, 0.01944444444444444475, 0.02222222222222222307, 0.02500000000000000139, 0.02777777777777777624, 0.03055555555555555455, 0.03333333333333333287, 0.03611111111111110772, 0.03888888888888888951, 0.04166666666666666435, 0.04444444444444444614, 0.04722222222222222099, 0.05000000000000000278, 0.05277777777777777762, 0.05555555555555555247, 0.05833333333333333426, 0.06111111111111110911, 0.06388888888888888395, 0.06666666666666666574, 0.06944444444444444753, 0.07222222222222221544, 0.07499999999999999722, 0.07777777777777777901, 0.08055555555555556080, 0.08333333333333332871, 0.08611111111111111049, 0.08888888888888889228, 0.09166666666666666019, 0.09444444444444444198, 0.09722222222222222376, 0.1000000000000000056, 0.1027777777777777735, 0.1055555555555555552, 0.1083333333333333370, 0.1111111111111111049, 0.1138888888888888867, 0.1166666666666666685, 0.1194444444444444503, 0.1222222222222222182, 0.1250000000000000000, 0.1277777777777777679, 0.1305555555555555636, 0.1333333333333333315, 0.1361111111111110994, 0.1388888888888888951, 0.1416666666666666630, 0.1444444444444444309, 0.1472222222222222265, 0.1499999999999999944, 0.1527777777777777901, 0.1555555555555555580, 0.1583333333333333259, 0.1611111111111111216, 0.1638888888888888895, 0.1666666666666666574, 0.1694444444444444531, 0.1722222222222222210, 0.1749999999999999889, 0.1777777777777777846, 0.1805555555555555525, 0.1833333333333333204, 0.1861111111111111160, 0.1888888888888888840, 0.1916666666666666796, 0.1944444444444444475, 0.1972222222222222154, 0.2000000000000000111, 0.2027777777777777790, 0.2055555555555555469, 0.2083333333333333426, 0.2111111111111111105, 0.2138888888888888784, 0.2166666666666666741, 0.2194444444444444420, 0.2222222222222222099, 0.2250000000000000056, 0.2277777777777777735, 0.2305555555555555691, 0.2333333333333333370, 0.2361111111111111049, 0.2388888888888889006, 0.2416666666666666685, 0.2444444444444444364, 0.2472222222222222321, 0.2500000000000000000, 0.2527777777777777679, 0.2555555555555555358, 0.2583333333333333592, 0.2611111111111111271, 0.2638888888888888951, 0.2666666666666666630, 0.2694444444444444309, 0.2722222222222221988, 0.2750000000000000222, 0.2777777777777777901, 0.2805555555555555580, 0.2833333333333333259, 0.2861111111111110938, 0.2888888888888888618, 0.2916666666666666852, 0.2944444444444444531, 0.2972222222222222210, 0.2999999999999999889, 0.3027777777777777568, 0.3055555555555555802, 0.3083333333333333481, 0.3111111111111111160, 0.3138888888888888840, 0.3166666666666666519, 0.3194444444444444198, 0.3222222222222222432, 0.3250000000000000111, 0.3277777777777777790, 0.3305555555555555469, 0.3333333333333333148, 0.3361111111111111382, 0.3388888888888889062, 0.3416666666666666741, 0.3444444444444444420, 0.3472222222222222099, 0.3499999999999999778, 0.3527777777777778012, 0.3555555555555555691, 0.3583333333333333370, 0.3611111111111111049, 0.3638888888888888729, 0.3666666666666666408, 0.3694444444444444642, 0.3722222222222222321, 0.3750000000000000000, 0.3777777777777777679, 0.3805555555555555358, 0.3833333333333333592, 0.3861111111111111271, 0.3888888888888888951, 0.3916666666666666630, 0.3944444444444444309, 0.3972222222222221988, 0.4000000000000000222, 0.4027777777777777901, 0.4055555555555555580, 0.4083333333333333259, 0.4111111111111110938, 0.4138888888888888618, 0.4166666666666666852, 0.4194444444444444531, 0.4222222222222222210, 0.4249999999999999889, 0.4277777777777777568, 0.4305555555555555802, 0.4333333333333333481, 0.4361111111111111160, 0.4388888888888888840, 0.4416666666666666519, 0.4444444444444444198, 0.4472222222222222432, 0.4500000000000000111, 0.4527777777777777790, 0.4555555555555555469, 0.4583333333333333148, 0.4611111111111111382, 0.4638888888888889062, 0.4666666666666666741, 0.4694444444444444420, 0.4722222222222222099, 0.4749999999999999778, 0.4777777777777778012, 0.4805555555555555691, 0.4833333333333333370, 0.4861111111111111049, 0.4888888888888888729, 0.4916666666666666408, 0.4944444444444444642, 0.4972222222222222321, 0.5000000000000000000, 0.5027777777777777679, 0.5055555555555555358, 0.5083333333333333037, 0.5111111111111110716, 0.5138888888888888395, 0.5166666666666667185, 0.5194444444444444864, 0.5222222222222222543, 0.5250000000000000222, 0.5277777777777777901, 0.5305555555555555580, 0.5333333333333333259, 0.5361111111111110938, 0.5388888888888888618, 0.5416666666666666297, 0.5444444444444443976, 0.5472222222222222765, 0.5500000000000000444, 0.5527777777777778123, 0.5555555555555555802, 0.5583333333333333481, 0.5611111111111111160, 0.5638888888888888840, 0.5666666666666666519, 0.5694444444444444198, 0.5722222222222221877, 0.5749999999999999556, 0.5777777777777777235, 0.5805555555555556024, 0.5833333333333333703, 0.5861111111111111382, 0.5888888888888889062, 0.5916666666666666741, 0.5944444444444444420, 0.5972222222222222099, 0.5999999999999999778, 0.6027777777777777457, 0.6055555555555555136, 0.6083333333333332815, 0.6111111111111111605, 0.6138888888888889284, 0.6166666666666666963, 0.6194444444444444642, 0.6222222222222222321, 0.6250000000000000000, 0.6277777777777777679, 0.6305555555555555358, 0.6333333333333333037, 0.6361111111111110716, 0.6388888888888888395, 0.6416666666666667185, 0.6444444444444444864, 0.6472222222222222543, 0.6500000000000000222, 0.6527777777777777901, 0.6555555555555555580, 0.6583333333333333259, 0.6611111111111110938, 0.6638888888888888618, 0.6666666666666666297, 0.6694444444444443976, 0.6722222222222222765, 0.6750000000000000444, 0.6777777777777778123, 0.6805555555555555802, 0.6833333333333333481, 0.6861111111111111160, 0.6888888888888888840, 0.6916666666666666519, 0.6944444444444444198, 0.6972222222222221877, 0.6999999999999999556, 0.7027777777777777235, 0.7055555555555556024, 0.7083333333333333703, 0.7111111111111111382, 0.7138888888888889062, 0.7166666666666666741, 0.7194444444444444420, 0.7222222222222222099, 0.7249999999999999778, 0.7277777777777777457, 0.7305555555555555136, 0.7333333333333332815, 0.7361111111111111605, 0.7388888888888889284, 0.7416666666666666963, 0.7444444444444444642, 0.7472222222222222321, 0.7500000000000000000, 0.7527777777777777679, 0.7555555555555555358, 0.7583333333333333037, 0.7611111111111110716, 0.7638888888888888395, 0.7666666666666667185, 0.7694444444444444864, 0.7722222222222222543, 0.7750000000000000222, 0.7777777777777777901, 0.7805555555555555580, 0.7833333333333333259, 0.7861111111111110938, 0.7888888888888888618, 0.7916666666666666297, 0.7944444444444443976, 0.7972222222222222765, 0.8000000000000000444, 0.8027777777777778123, 0.8055555555555555802, 0.8083333333333333481, 0.8111111111111111160, 0.8138888888888888840, 0.8166666666666666519, 0.8194444444444444198, 0.8222222222222221877, 0.8249999999999999556, 0.8277777777777777235, 0.8305555555555556024, 0.8333333333333333703, 0.8361111111111111382, 0.8388888888888889062, 0.8416666666666666741, 0.8444444444444444420, 0.8472222222222222099, 0.8499999999999999778, 0.8527777777777777457, 0.8555555555555555136, 0.8583333333333332815, 0.8611111111111111605, 0.8638888888888889284, 0.8666666666666666963, 0.8694444444444444642, 0.8722222222222222321, 0.8750000000000000000, 0.8777777777777777679, 0.8805555555555555358, 0.8833333333333333037, 0.8861111111111110716, 0.8888888888888888395, 0.8916666666666667185, 0.8944444444444444864, 0.8972222222222222543, 0.9000000000000000222, 0.9027777777777777901, 0.9055555555555555580, 0.9083333333333333259, 0.9111111111111110938, 0.9138888888888888618, 0.9166666666666666297, 0.9194444444444443976, 0.9222222222222222765, 0.9250000000000000444, 0.9277777777777778123, 0.9305555555555555802, 0.9333333333333333481, 0.9361111111111111160, 0.9388888888888888840, 0.9416666666666666519, 0.9444444444444444198, 0.9472222222222221877, 0.9499999999999999556, 0.9527777777777777235, 0.9555555555555556024, 0.9583333333333333703, 0.9611111111111111382, 0.9638888888888889062, 0.9666666666666666741, 0.9694444444444444420, 0.9722222222222222099, 0.9749999999999999778, 0.9777777777777777457, 0.9805555555555555136, 0.9833333333333332815, 0.9861111111111111605, 0.9888888888888889284, 0.9916666666666666963, 0.9944444444444444642, 0.9972222222222222321, 1.000000000000000000 ),
 .UNSPECIFIED. ) 
 GEOMETRIC_REPRESENTATION_ITEM ( )  RATIONAL_B_SPLINE_SURFACE ( (
 ( 1.000000000000000000, 0.8660254037844387076, 1.000000000000000000, 0.8660254037844387076, 1.000000000000000000, 0.8660254037844387076, 1.000000000000000000, 0.8660254037844387076, 1.000000000000000000, 0.8660254037844387076, 1.000000000000000000, 0.8660254037844387076, 1.000000000000000000, 0.8660254037844387076, 1.000000000000000000, 0.8660254037844387076, 1.000000000000000000, 0.8660254037844387076, 1.000000000000000000, 0.8660254037844387076, 1.000000000000000000, 0.8660254037844387076, 1.000000000000000000, 0.8660254037844387076, 1.000000000000000000, 0.8660254037844387076, 1.000000000000000000, 0.8660254037844387076, 1.000000000000000000, 0.8660254037844387076, 1.000000000000000000, 0.8660254037844387076, 1.000000000000000000, 0.8660254037844387076, 1.000000000000000000, 0.8660254037844387076, 1.000000000000000000, 0.8660254037844387076, 1.000000000000000000, 0.8660254037844387076, 1.000000000000000000, 0.8660254037844387076, 1.000000000000000000, 0.8660254037844387076, 1.000000000000000000, 0.8660254037844387076, 1.000000000000000000, 0.8660254037844387076, 1.000000000000000000, 0.8660254037844387076, 1.000000000000000000, 0.8660254037844387076, 1.000000000000000000, 0.8660254037844387076, 1.000000000000000000, 0.8660254037844387076, 1.000000000000000000, 0.8660254037844387076, 1.000000000000000000, 0.8660254037844387076, 1.000000000000000000, 0.8660254037844387076, 1.000000000000000000, 0.8660254037844387076, 1.000000000000000000, 0.8660254037844387076, 1.000000000000000000, 0.8660254037844387076, 1.000000000000000000, 0.8660254037844387076, 1.000000000000000000, 0.8660254037844387076, 1.000000000000000000, 0.8660254037844387076, 1.000000000000000000, 0.8660254037844387076, 1.000000000000000000, 0.8660254037844387076, 1.000000000000000000, 0.8660254037844387076, 1.000000000000000000, 0.8660254037844387076, 1.000000000000000000, 0.8660254037844387076, 1.000000000000000000, 0.8660254037844387076, 1.000000000000000000, 0.8660254037844387076, 1.000000000000000000, 0.8660254037844387076, 1.000000000000000000, 0.8660254037844387076, 1.000000000000000000, 0.8660254037844387076, 1.000000000000000000, 0.8660254037844387076, 1.000000000000000000, 0.8660254037844387076, 1.000000000000000000, 0.8660254037844387076, 1.000000000000000000, 0.8660254037844387076, 1.000000000000000000, 0.8660254037844387076, 1.000000000000000000, 0.8660254037844387076, 1.000000000000000000, 0.8660254037844387076, 1.000000000000000000, 0.8660254037844387076, 1.000000000000000000, 0.8660254037844387076, 1.000000000000000000, 0.8660254037844387076, 1.000000000000000000, 0.8660254037844387076, 1.000000000000000000, 0.8660254037844387076, 1.000000000000000000, 0.8660254037844387076, 1.000000000000000000, 0.8660254037844387076, 1.000000000000000000, 0.8660254037844387076, 1.000000000000000000, 0.8660254037844387076, 1.000000000000000000, 0.8660254037844387076, 1.000000000000000000, 0.8660254037844387076, 1.000000000000000000, 0.8660254037844387076, 1.000000000000000000, 0.8660254037844387076, 1.000000000000000000, 0.8660254037844387076, 1.000000000000000000, 0.8660254037844387076, 1.000000000000000000, 0.8660254037844387076, 1.000000000000000000, 0.8660254037844387076, 1.000000000000000000, 0.8660254037844387076, 1.000000000000000000, 0.8660254037844387076, 1.000000000000000000, 0.8660254037844387076, 1.000000000000000000, 0.8660254037844387076, 1.000000000000000000, 0.8660254037844387076, 1.000000000000000000, 0.8660254037844387076, 1.000000000000000000, 0.8660254037844387076, 1.000000000000000000, 0.8660254037844387076, 1.000000000000000000, 0.8660254037844387076, 1.000000000000000000, 0.8660254037844387076, 1.000000000000000000, 0.8660254037844387076, 1.000000000000000000, 0.8660254037844387076, 1.000000000000000000, 0.8660254037844387076, 1.000000000000000000, 0.8660254037844387076, 1.000000000000000000, 0.8660254037844387076, 1.000000000000000000, 0.8660254037844387076, 1.000000000000000000, 0.8660254037844387076, 1.000000000000000000, 0.8660254037844387076, 1.000000000000000000, 0.8660254037844387076, 1.000000000000000000, 0.8660254037844387076, 1.000000000000000000, 0.8660254037844387076, 1.000000000000000000, 0.8660254037844387076, 1.000000000000000000, 0.8660254037844387076, 1.000000000000000000, 0.8660254037844387076, 1.000000000000000000, 0.8660254037844387076, 1.000000000000000000, 0.8660254037844387076, 1.000000000000000000, 0.8660254037844387076, 1.000000000000000000, 0.8660254037844387076, 1.000000000000000000, 0.8660254037844387076, 1.000000000000000000, 0.8660254037844387076, 1.000000000000000000, 0.8660254037844387076, 1.000000000000000000, 0.8660254037844387076, 1.000000000000000000, 0.8660254037844387076, 1.000000000000000000, 0.8660254037844387076, 1.000000000000000000, 0.8660254037844387076, 1.000000000000000000, 0.8660254037844387076, 1.000000000000000000, 0.8660254037844387076, 1.000000000000000000, 0.8660254037844387076, 1.000000000000000000, 0.8660254037844387076, 1.000000000000000000, 0.8660254037844387076, 1.000000000000000000, 0.8660254037844387076, 1.000000000000000000, 0.8660254037844387076, 1.000000000000000000, 0.8660254037844387076, 1.000000000000000000, 0.8660254037844387076, 1.000000000000000000, 0.8660254037844387076, 1.000000000000000000, 0.8660254037844387076, 1.000000000000000000, 0.8660254037844387076, 1.000000000000000000, 0.8660254037844387076, 1.000000000000000000, 0.8660254037844387076, 1.000000000000000000, 0.8660254037844387076, 1.000000000000000000, 0.8660254037844387076, 1.000000000000000000, 0.8660254037844387076, 1.000000000000000000, 0.8660254037844387076, 1.000000000000000000, 0.8660254037844387076, 1.000000000000000000, 0.8660254037844387076, 1.000000000000000000, 0.8660254037844387076, 1.000000000000000000, 0.8660254037844387076, 1.000000000000000000, 0.8660254037844387076, 1.000000000000000000, 0.8660254037844387076, 1.000000000000000000, 0.8660254037844387076, 1.000000000000000000, 0.8660254037844387076, 1.000000000000000000, 0.8660254037844387076, 1.000000000000000000, 0.8660254037844387076, 1.000000000000000000, 0.8660254037844387076, 1.000000000000000000, 0.8660254037844387076, 1.000000000000000000, 0.8660254037844387076, 1.000000000000000000, 0.8660254037844387076, 1.000000000000000000, 0.8660254037844387076, 1.000000000000000000, 0.8660254037844387076, 1.000000000000000000, 0.8660254037844387076, 1.000000000000000000, 0.8660254037844387076, 1.000000000000000000, 0.8660254037844387076, 1.000000000000000000, 0.8660254037844387076, 1.000000000000000000, 0.8660254037844387076, 1.000000000000000000, 0.8660254037844387076, 1.000000000000000000, 0.8660254037844387076, 1.000000000000000000, 0.8660254037844387076, 1.000000000000000000, 0.8660254037844387076, 1.000000000000000000, 0.8660254037844387076, 1.000000000000000000, 0.8660254037844387076, 1.000000000000000000, 0.8660254037844387076, 1.000000000000000000, 0.8660254037844387076, 1.000000000000000000, 0.8660254037844387076, 1.000000000000000000, 0.8660254037844387076, 1.000000000000000000, 0.8660254037844387076, 1.000000000000000000, 0.8660254037844387076, 1.000000000000000000, 0.8660254037844387076, 1.000000000000000000, 0.8660254037844387076, 1.000000000000000000, 0.8660254037844387076, 1.000000000000000000, 0.8660254037844387076, 1.000000000000000000, 0.8660254037844387076, 1.000000000000000000, 0.8660254037844387076, 1.000000000000000000, 0.8660254037844387076, 1.000000000000000000, 0.8660254037844387076, 1.000000000000000000, 0.8660254037844387076, 1.000000000000000000, 0.8660254037844387076, 1.000000000000000000, 0.8660254037844387076, 1.000000000000000000, 0.8660254037844387076, 1.000000000000000000, 0.8660254037844387076, 1.000000000000000000, 0.8660254037844387076, 1.000000000000000000, 0.8660254037844387076, 1.000000000000000000, 0.8660254037844387076, 1.000000000000000000, 0.8660254037844387076, 1.000000000000000000, 0.8660254037844387076, 1.000000000000000000, 0.8660254037844387076, 1.000000000000000000, 0.8660254037844387076, 1.000000000000000000, 0.8660254037844387076, 1.000000000000000000, 0.8660254037844387076, 1.000000000000000000, 0.8660254037844387076, 1.000000000000000000, 0.8660254037844387076, 1.000000000000000000, 0.8660254037844387076, 1.000000000000000000, 0.8660254037844387076, 1.000000000000000000, 0.8660254037844387076, 1.000000000000000000, 0.8660254037844387076, 1.000000000000000000, 0.8660254037844387076, 1.000000000000000000, 0.8660254037844387076, 1.000000000000000000, 0.8660254037844387076, 1.000000000000000000, 0.8660254037844387076, 1.000000000000000000, 0.8660254037844387076, 1.000000000000000000, 0.8660254037844387076, 1.000000000000000000, 0.8660254037844387076, 1.000000000000000000, 0.8660254037844387076, 1.000000000000000000, 0.8660254037844387076, 1.000000000000000000, 0.8660254037844387076, 1.000000000000000000, 0.8660254037844387076, 1.000000000000000000, 0.8660254037844387076, 1.000000000000000000, 0.8660254037844387076, 1.000000000000000000, 0.8660254037844387076, 1.000000000000000000, 0.8660254037844387076, 1.000000000000000000, 0.8660254037844387076, 1.000000000000000000, 0.8660254037844387076, 1.000000000000000000, 0.8660254037844387076, 1.000000000000000000, 0.8660254037844387076, 1.000000000000000000, 0.8660254037844387076, 1.000000000000000000, 0.8660254037844387076, 1.000000000000000000, 0.8660254037844387076, 1.000000000000000000, 0.8660254037844387076, 1.000000000000000000, 0.8660254037844387076, 1.000000000000000000, 0.8660254037844387076, 1.000000000000000000, 0.8660254037844387076, 1.000000000000000000, 0.8660254037844387076, 1.000000000000000000, 0.8660254037844387076, 1.000000000000000000, 0.8660254037844387076, 1.000000000000000000, 0.8660254037844387076, 1.000000000000000000, 0.8660254037844387076, 1.000000000000000000, 0.8660254037844387076, 1.000000000000000000, 0.8660254037844387076, 1.000000000000000000, 0.8660254037844387076, 1.000000000000000000, 0.8660254037844387076, 1.000000000000000000, 0.8660254037844387076, 1.000000000000000000, 0.8660254037844387076, 1.000000000000000000, 0.8660254037844387076, 1.000000000000000000, 0.8660254037844387076, 1.000000000000000000, 0.8660254037844387076, 1.000000000000000000, 0.8660254037844387076, 1.000000000000000000, 0.8660254037844387076, 1.000000000000000000, 0.8660254037844387076, 1.000000000000000000, 0.8660254037844387076, 1.000000000000000000, 0.8660254037844387076, 1.000000000000000000, 0.8660254037844387076, 1.000000000000000000, 0.8660254037844387076, 1.000000000000000000, 0.8660254037844387076, 1.000000000000000000, 0.8660254037844387076, 1.000000000000000000, 0.8660254037844387076, 1.000000000000000000, 0.8660254037844387076, 1.000000000000000000, 0.8660254037844387076, 1.000000000000000000, 0.8660254037844387076, 1.000000000000000000, 0.8660254037844387076, 1.000000000000000000, 0.8660254037844387076, 1.000000000000000000, 0.8660254037844387076, 1.000000000000000000, 0.8660254037844387076, 1.000000000000000000, 0.8660254037844387076, 1.000000000000000000, 0.8660254037844387076, 1.000000000000000000, 0.8660254037844387076, 1.000000000000000000, 0.8660254037844387076, 1.000000000000000000, 0.8660254037844387076, 1.000000000000000000, 0.8660254037844387076, 1.000000000000000000, 0.8660254037844387076, 1.000000000000000000, 0.8660254037844387076, 1.000000000000000000, 0.8660254037844387076, 1.000000000000000000, 0.8660254037844387076, 1.000000000000000000, 0.8660254037844387076, 1.000000000000000000, 0.8660254037844387076, 1.000000000000000000, 0.8660254037844387076, 1.000000000000000000, 0.8660254037844387076, 1.000000000000000000, 0.8660254037844387076, 1.000000000000000000, 0.8660254037844387076, 1.000000000000000000, 0.8660254037844387076, 1.000000000000000000, 0.8660254037844387076, 1.000000000000000000, 0.8660254037844387076, 1.000000000000000000, 0.8660254037844387076, 1.000000000000000000, 0.8660254037844387076, 1.000000000000000000, 0.8660254037844387076, 1.000000000000000000, 0.8660254037844387076, 1.000000000000000000, 0.8660254037844387076, 1.000000000000000000, 0.8660254037844387076, 1.000000000000000000, 0.8660254037844387076, 1.000000000000000000, 0.8660254037844387076, 1.000000000000000000, 0.8660254037844387076, 1.000000000000000000, 0.8660254037844387076, 1.000000000000000000, 0.8660254037844387076, 1.000000000000000000, 0.8660254037844387076, 1.000000000000000000, 0.8660254037844387076, 1.000000000000000000, 0.8660254037844387076, 1.000000000000000000, 0.8660254037844387076, 1.000000000000000000, 0.8660254037844387076, 1.000000000000000000, 0.8660254037844387076, 1.000000000000000000, 0.8660254037844387076, 1.000000000000000000, 0.8660254037844387076, 1.000000000000000000, 0.8660254037844387076, 1.000000000000000000, 0.8660254037844387076, 1.000000000000000000, 0.8660254037844387076, 1.000000000000000000, 0.8660254037844387076, 1.000000000000000000, 0.8660254037844387076, 1.000000000000000000, 0.8660254037844387076, 1.000000000000000000, 0.8660254037844387076, 1.000000000000000000, 0.8660254037844387076, 1.000000000000000000, 0.8660254037844387076, 1.000000000000000000, 0.8660254037844387076, 1.000000000000000000, 0.8660254037844387076, 1.000000000000000000, 0.8660254037844387076, 1.000000000000000000, 0.8660254037844387076, 1.000000000000000000, 0.8660254037844387076, 1.000000000000000000, 0.8660254037844387076, 1.000000000000000000, 0.8660254037844387076, 1.000000000000000000, 0.8660254037844387076, 1.000000000000000000, 0.8660254037844387076, 1.000000000000000000, 0.8660254037844387076, 1.000000000000000000, 0.8660254037844387076, 1.000000000000000000, 0.8660254037844387076, 1.000000000000000000, 0.8660254037844387076, 1.000000000000000000, 0.8660254037844387076, 1.000000000000000000, 0.8660254037844387076, 1.000000000000000000, 0.8660254037844387076, 1.000000000000000000, 0.8660254037844387076, 1.000000000000000000, 0.8660254037844387076, 1.000000000000000000, 0.8660254037844387076, 1.000000000000000000, 0.8660254037844387076, 1.000000000000000000, 0.8660254037844387076, 1.000000000000000000, 0.8660254037844387076, 1.000000000000000000, 0.8660254037844387076, 1.000000000000000000, 0.8660254037844387076, 1.000000000000000000, 0.8660254037844387076, 1.000000000000000000, 0.8660254037844387076, 1.000000000000000000, 0.8660254037844387076, 1.000000000000000000, 0.8660254037844387076, 1.000000000000000000, 0.8660254037844387076, 1.000000000000000000, 0.8660254037844387076, 1.000000000000000000, 0.8660254037844387076, 1.000000000000000000, 0.8660254037844387076, 1.000000000000000000, 0.8660254037844387076, 1.000000000000000000, 0.8660254037844387076, 1.000000000000000000, 0.8660254037844387076, 1.000000000000000000, 0.8660254037844387076, 1.000000000000000000, 0.8660254037844387076, 1.000000000000000000, 0.8660254037844387076, 1.000000000000000000, 0.8660254037844387076, 1.000000000000000000, 0.8660254037844387076, 1.000000000000000000, 0.8660254037844387076, 1.000000000000000000, 0.8660254037844387076, 1.000000000000000000, 0.8660254037844387076, 1.000000000000000000, 0.8660254037844387076, 1.000000000000000000, 0.8660254037844387076, 1.000000000000000000, 0.8660254037844387076, 1.000000000000000000, 0.8660254037844387076, 1.000000000000000000, 0.8660254037844387076, 1.000000000000000000, 0.8660254037844387076, 1.000000000000000000, 0.8660254037844387076, 1.000000000000000000, 0.8660254037844387076, 1.000000000000000000, 0.8660254037844387076, 1.000000000000000000, 0.8660254037844387076, 1.000000000000000000, 0.8660254037844387076, 1.000000000000000000, 0.8660254037844387076, 1.000000000000000000, 0.8660254037844387076, 1.000000000000000000, 0.8660254037844387076, 1.000000000000000000, 0.8660254037844387076, 1.000000000000000000, 0.8660254037844387076, 1.000000000000000000, 0.8660254037844387076, 1.000000000000000000, 0.8660254037844387076, 1.000000000000000000, 0.8660254037844387076, 1.000000000000000000, 0.8660254037844387076, 1.000000000000000000, 0.8660254037844387076, 1.000000000000000000, 0.8660254037844387076, 1.000000000000000000, 0.8660254037844387076, 1.000000000000000000, 0.8660254037844387076, 1.000000000000000000, 0.8660254037844387076, 1.000000000000000000, 0.8660254037844387076, 1.000000000000000000, 0.8660254037844387076, 1.000000000000000000, 0.8660254037844387076, 1.000000000000000000),
 ( 1.000000000000000000, 0.8660254037844387076, 1.000000000000000000, 0.8660254037844387076, 1.000000000000000000, 0.8660254037844387076, 1.000000000000000000, 0.8660254037844387076, 1.000000000000000000, 0.8660254037844387076, 1.000000000000000000, 0.8660254037844387076, 1.000000000000000000, 0.8660254037844387076, 1.000000000000000000, 0.8660254037844387076, 1.000000000000000000, 0.8660254037844387076, 1.000000000000000000, 0.8660254037844387076, 1.000000000000000000, 0.8660254037844387076, 1.000000000000000000, 0.8660254037844387076, 1.000000000000000000, 0.8660254037844387076, 1.000000000000000000, 0.8660254037844387076, 1.000000000000000000, 0.8660254037844387076, 1.000000000000000000, 0.8660254037844387076, 1.000000000000000000, 0.8660254037844387076, 1.000000000000000000, 0.8660254037844387076, 1.000000000000000000, 0.8660254037844387076, 1.000000000000000000, 0.8660254037844387076, 1.000000000000000000, 0.8660254037844387076, 1.000000000000000000, 0.8660254037844387076, 1.000000000000000000, 0.8660254037844387076, 1.000000000000000000, 0.8660254037844387076, 1.000000000000000000, 0.8660254037844387076, 1.000000000000000000, 0.8660254037844387076, 1.000000000000000000, 0.8660254037844387076, 1.000000000000000000, 0.8660254037844387076, 1.000000000000000000, 0.8660254037844387076, 1.000000000000000000, 0.8660254037844387076, 1.000000000000000000, 0.8660254037844387076, 1.000000000000000000, 0.8660254037844387076, 1.000000000000000000, 0.8660254037844387076, 1.000000000000000000, 0.8660254037844387076, 1.000000000000000000, 0.8660254037844387076, 1.000000000000000000, 0.8660254037844387076, 1.000000000000000000, 0.8660254037844387076, 1.000000000000000000, 0.8660254037844387076, 1.000000000000000000, 0.8660254037844387076, 1.000000000000000000, 0.8660254037844387076, 1.000000000000000000, 0.8660254037844387076, 1.000000000000000000, 0.8660254037844387076, 1.000000000000000000, 0.8660254037844387076, 1.000000000000000000, 0.8660254037844387076, 1.000000000000000000, 0.8660254037844387076, 1.000000000000000000, 0.8660254037844387076, 1.000000000000000000, 0.8660254037844387076, 1.000000000000000000, 0.8660254037844387076, 1.000000000000000000, 0.8660254037844387076, 1.000000000000000000, 0.8660254037844387076, 1.000000000000000000, 0.8660254037844387076, 1.000000000000000000, 0.8660254037844387076, 1.000000000000000000, 0.8660254037844387076, 1.000000000000000000, 0.8660254037844387076, 1.000000000000000000, 0.8660254037844387076, 1.000000000000000000, 0.8660254037844387076, 1.000000000000000000, 0.8660254037844387076, 1.000000000000000000, 0.8660254037844387076, 1.000000000000000000, 0.8660254037844387076, 1.000000000000000000, 0.8660254037844387076, 1.000000000000000000, 0.8660254037844387076, 1.000000000000000000, 0.8660254037844387076, 1.000000000000000000, 0.8660254037844387076, 1.000000000000000000, 0.8660254037844387076, 1.000000000000000000, 0.8660254037844387076, 1.000000000000000000, 0.8660254037844387076, 1.000000000000000000, 0.8660254037844387076, 1.000000000000000000, 0.8660254037844387076, 1.000000000000000000, 0.8660254037844387076, 1.000000000000000000, 0.8660254037844387076, 1.000000000000000000, 0.8660254037844387076, 1.000000000000000000, 0.8660254037844387076, 1.000000000000000000, 0.8660254037844387076, 1.000000000000000000, 0.8660254037844387076, 1.000000000000000000, 0.8660254037844387076, 1.000000000000000000, 0.8660254037844387076, 1.000000000000000000, 0.8660254037844387076, 1.000000000000000000, 0.8660254037844387076, 1.000000000000000000, 0.8660254037844387076, 1.000000000000000000, 0.8660254037844387076, 1.000000000000000000, 0.8660254037844387076, 1.000000000000000000, 0.8660254037844387076, 1.000000000000000000, 0.8660254037844387076, 1.000000000000000000, 0.8660254037844387076, 1.000000000000000000, 0.8660254037844387076, 1.000000000000000000, 0.8660254037844387076, 1.000000000000000000, 0.8660254037844387076, 1.000000000000000000, 0.8660254037844387076, 1.000000000000000000, 0.8660254037844387076, 1.000000000000000000, 0.8660254037844387076, 1.000000000000000000, 0.8660254037844387076, 1.000000000000000000, 0.8660254037844387076, 1.000000000000000000, 0.8660254037844387076, 1.000000000000000000, 0.8660254037844387076, 1.000000000000000000, 0.8660254037844387076, 1.000000000000000000, 0.8660254037844387076, 1.000000000000000000, 0.8660254037844387076, 1.000000000000000000, 0.8660254037844387076, 1.000000000000000000, 0.8660254037844387076, 1.000000000000000000, 0.8660254037844387076, 1.000000000000000000, 0.8660254037844387076, 1.000000000000000000, 0.8660254037844387076, 1.000000000000000000, 0.8660254037844387076, 1.000000000000000000, 0.8660254037844387076, 1.000000000000000000, 0.8660254037844387076, 1.000000000000000000, 0.8660254037844387076, 1.000000000000000000, 0.8660254037844387076, 1.000000000000000000, 0.8660254037844387076, 1.000000000000000000, 0.8660254037844387076, 1.000000000000000000, 0.8660254037844387076, 1.000000000000000000, 0.8660254037844387076, 1.000000000000000000, 0.8660254037844387076, 1.000000000000000000, 0.8660254037844387076, 1.000000000000000000, 0.8660254037844387076, 1.000000000000000000, 0.8660254037844387076, 1.000000000000000000, 0.8660254037844387076, 1.000000000000000000, 0.8660254037844387076, 1.000000000000000000, 0.8660254037844387076, 1.000000000000000000, 0.8660254037844387076, 1.000000000000000000, 0.8660254037844387076, 1.000000000000000000, 0.8660254037844387076, 1.000000000000000000, 0.8660254037844387076, 1.000000000000000000, 0.8660254037844387076, 1.000000000000000000, 0.8660254037844387076, 1.000000000000000000, 0.8660254037844387076, 1.000000000000000000, 0.8660254037844387076, 1.000000000000000000, 0.8660254037844387076, 1.000000000000000000, 0.8660254037844387076, 1.000000000000000000, 0.8660254037844387076, 1.000000000000000000, 0.8660254037844387076, 1.000000000000000000, 0.8660254037844387076, 1.000000000000000000, 0.8660254037844387076, 1.000000000000000000, 0.8660254037844387076, 1.000000000000000000, 0.8660254037844387076, 1.000000000000000000, 0.8660254037844387076, 1.000000000000000000, 0.8660254037844387076, 1.000000000000000000, 0.8660254037844387076, 1.000000000000000000, 0.8660254037844387076, 1.000000000000000000, 0.8660254037844387076, 1.000000000000000000, 0.8660254037844387076, 1.000000000000000000, 0.8660254037844387076, 1.000000000000000000, 0.8660254037844387076, 1.000000000000000000, 0.8660254037844387076, 1.000000000000000000, 0.8660254037844387076, 1.000000000000000000, 0.8660254037844387076, 1.000000000000000000, 0.8660254037844387076, 1.000000000000000000, 0.8660254037844387076, 1.000000000000000000, 0.8660254037844387076, 1.000000000000000000, 0.8660254037844387076, 1.000000000000000000, 0.8660254037844387076, 1.000000000000000000, 0.8660254037844387076, 1.000000000000000000, 0.8660254037844387076, 1.000000000000000000, 0.8660254037844387076, 1.000000000000000000, 0.8660254037844387076, 1.000000000000000000, 0.8660254037844387076, 1.000000000000000000, 0.8660254037844387076, 1.000000000000000000, 0.8660254037844387076, 1.000000000000000000, 0.8660254037844387076, 1.000000000000000000, 0.8660254037844387076, 1.000000000000000000, 0.8660254037844387076, 1.000000000000000000, 0.8660254037844387076, 1.000000000000000000, 0.8660254037844387076, 1.000000000000000000, 0.8660254037844387076, 1.000000000000000000, 0.8660254037844387076, 1.000000000000000000, 0.8660254037844387076, 1.000000000000000000, 0.8660254037844387076, 1.000000000000000000, 0.8660254037844387076, 1.000000000000000000, 0.8660254037844387076, 1.000000000000000000, 0.8660254037844387076, 1.000000000000000000, 0.8660254037844387076, 1.000000000000000000, 0.8660254037844387076, 1.000000000000000000, 0.8660254037844387076, 1.000000000000000000, 0.8660254037844387076, 1.000000000000000000, 0.8660254037844387076, 1.000000000000000000, 0.8660254037844387076, 1.000000000000000000, 0.8660254037844387076, 1.000000000000000000, 0.8660254037844387076, 1.000000000000000000, 0.8660254037844387076, 1.000000000000000000, 0.8660254037844387076, 1.000000000000000000, 0.8660254037844387076, 1.000000000000000000, 0.8660254037844387076, 1.000000000000000000, 0.8660254037844387076, 1.000000000000000000, 0.8660254037844387076, 1.000000000000000000, 0.8660254037844387076, 1.000000000000000000, 0.8660254037844387076, 1.000000000000000000, 0.8660254037844387076, 1.000000000000000000, 0.8660254037844387076, 1.000000000000000000, 0.8660254037844387076, 1.000000000000000000, 0.8660254037844387076, 1.000000000000000000, 0.8660254037844387076, 1.000000000000000000, 0.8660254037844387076, 1.000000000000000000, 0.8660254037844387076, 1.000000000000000000, 0.8660254037844387076, 1.000000000000000000, 0.8660254037844387076, 1.000000000000000000, 0.8660254037844387076, 1.000000000000000000, 0.8660254037844387076, 1.000000000000000000, 0.8660254037844387076, 1.000000000000000000, 0.8660254037844387076, 1.000000000000000000, 0.8660254037844387076, 1.000000000000000000, 0.8660254037844387076, 1.000000000000000000, 0.8660254037844387076, 1.000000000000000000, 0.8660254037844387076, 1.000000000000000000, 0.8660254037844387076, 1.000000000000000000, 0.8660254037844387076, 1.000000000000000000, 0.8660254037844387076, 1.000000000000000000, 0.8660254037844387076, 1.000000000000000000, 0.8660254037844387076, 1.000000000000000000, 0.8660254037844387076, 1.000000000000000000, 0.8660254037844387076, 1.000000000000000000, 0.8660254037844387076, 1.000000000000000000, 0.8660254037844387076, 1.000000000000000000, 0.8660254037844387076, 1.000000000000000000, 0.8660254037844387076, 1.000000000000000000, 0.8660254037844387076, 1.000000000000000000, 0.8660254037844387076, 1.000000000000000000, 0.8660254037844387076, 1.000000000000000000, 0.8660254037844387076, 1.000000000000000000, 0.8660254037844387076, 1.000000000000000000, 0.8660254037844387076, 1.000000000000000000, 0.8660254037844387076, 1.000000000000000000, 0.8660254037844387076, 1.000000000000000000, 0.8660254037844387076, 1.000000000000000000, 0.8660254037844387076, 1.000000000000000000, 0.8660254037844387076, 1.000000000000000000, 0.8660254037844387076, 1.000000000000000000, 0.8660254037844387076, 1.000000000000000000, 0.8660254037844387076, 1.000000000000000000, 0.8660254037844387076, 1.000000000000000000, 0.8660254037844387076, 1.000000000000000000, 0.8660254037844387076, 1.000000000000000000, 0.8660254037844387076, 1.000000000000000000, 0.8660254037844387076, 1.000000000000000000, 0.8660254037844387076, 1.000000000000000000, 0.8660254037844387076, 1.000000000000000000, 0.8660254037844387076, 1.000000000000000000, 0.8660254037844387076, 1.000000000000000000, 0.8660254037844387076, 1.000000000000000000, 0.8660254037844387076, 1.000000000000000000, 0.8660254037844387076, 1.000000000000000000, 0.8660254037844387076, 1.000000000000000000, 0.8660254037844387076, 1.000000000000000000, 0.8660254037844387076, 1.000000000000000000, 0.8660254037844387076, 1.000000000000000000, 0.8660254037844387076, 1.000000000000000000, 0.8660254037844387076, 1.000000000000000000, 0.8660254037844387076, 1.000000000000000000, 0.8660254037844387076, 1.000000000000000000, 0.8660254037844387076, 1.000000000000000000, 0.8660254037844387076, 1.000000000000000000, 0.8660254037844387076, 1.000000000000000000, 0.8660254037844387076, 1.000000000000000000, 0.8660254037844387076, 1.000000000000000000, 0.8660254037844387076, 1.000000000000000000, 0.8660254037844387076, 1.000000000000000000, 0.8660254037844387076, 1.000000000000000000, 0.8660254037844387076, 1.000000000000000000, 0.8660254037844387076, 1.000000000000000000, 0.8660254037844387076, 1.000000000000000000, 0.8660254037844387076, 1.000000000000000000, 0.8660254037844387076, 1.000000000000000000, 0.8660254037844387076, 1.000000000000000000, 0.8660254037844387076, 1.000000000000000000, 0.8660254037844387076, 1.000000000000000000, 0.8660254037844387076, 1.000000000000000000, 0.8660254037844387076, 1.000000000000000000, 0.8660254037844387076, 1.000000000000000000, 0.8660254037844387076, 1.000000000000000000, 0.8660254037844387076, 1.000000000000000000, 0.8660254037844387076, 1.000000000000000000, 0.8660254037844387076, 1.000000000000000000, 0.8660254037844387076, 1.000000000000000000, 0.8660254037844387076, 1.000000000000000000, 0.8660254037844387076, 1.000000000000000000, 0.8660254037844387076, 1.000000000000000000, 0.8660254037844387076, 1.000000000000000000, 0.8660254037844387076, 1.000000000000000000, 0.8660254037844387076, 1.000000000000000000, 0.8660254037844387076, 1.000000000000000000, 0.8660254037844387076, 1.000000000000000000, 0.8660254037844387076, 1.000000000000000000, 0.8660254037844387076, 1.000000000000000000, 0.8660254037844387076, 1.000000000000000000, 0.8660254037844387076, 1.000000000000000000, 0.8660254037844387076, 1.000000000000000000, 0.8660254037844387076, 1.000000000000000000, 0.8660254037844387076, 1.000000000000000000, 0.8660254037844387076, 1.000000000000000000, 0.8660254037844387076, 1.000000000000000000, 0.8660254037844387076, 1.000000000000000000, 0.8660254037844387076, 1.000000000000000000, 0.8660254037844387076, 1.000000000000000000, 0.8660254037844387076, 1.000000000000000000, 0.8660254037844387076, 1.000000000000000000, 0.8660254037844387076, 1.000000000000000000, 0.8660254037844387076, 1.000000000000000000, 0.8660254037844387076, 1.000000000000000000, 0.8660254037844387076, 1.000000000000000000, 0.8660254037844387076, 1.000000000000000000, 0.8660254037844387076, 1.000000000000000000, 0.8660254037844387076, 1.000000000000000000, 0.8660254037844387076, 1.000000000000000000, 0.8660254037844387076, 1.000000000000000000, 0.8660254037844387076, 1.000000000000000000, 0.8660254037844387076, 1.000000000000000000, 0.8660254037844387076, 1.000000000000000000, 0.8660254037844387076, 1.000000000000000000, 0.8660254037844387076, 1.000000000000000000, 0.8660254037844387076, 1.000000000000000000, 0.8660254037844387076, 1.000000000000000000, 0.8660254037844387076, 1.000000000000000000, 0.8660254037844387076, 1.000000000000000000, 0.8660254037844387076, 1.000000000000000000, 0.8660254037844387076, 1.000000000000000000, 0.8660254037844387076, 1.000000000000000000, 0.8660254037844387076, 1.000000000000000000, 0.8660254037844387076, 1.000000000000000000, 0.8660254037844387076, 1.000000000000000000, 0.8660254037844387076, 1.000000000000000000, 0.8660254037844387076, 1.000000000000000000, 0.8660254037844387076, 1.000000000000000000, 0.8660254037844387076, 1.000000000000000000, 0.8660254037844387076, 1.000000000000000000, 0.8660254037844387076, 1.000000000000000000, 0.8660254037844387076, 1.000000000000000000, 0.8660254037844387076, 1.000000000000000000, 0.8660254037844387076, 1.000000000000000000, 0.8660254037844387076, 1.000000000000000000, 0.8660254037844387076, 1.000000000000000000, 0.8660254037844387076, 1.000000000000000000, 0.8660254037844387076, 1.000000000000000000, 0.8660254037844387076, 1.000000000000000000, 0.8660254037844387076, 1.000000000000000000, 0.8660254037844387076, 1.000000000000000000, 0.8660254037844387076, 1.000000000000000000, 0.8660254037844387076, 1.000000000000000000, 0.8660254037844387076, 1.000000000000000000, 0.8660254037844387076, 1.000000000000000000, 0.8660254037844387076, 1.000000000000000000, 0.8660254037844387076, 1.000000000000000000, 0.8660254037844387076, 1.000000000000000000, 0.8660254037844387076, 1.000000000000000000, 0.8660254037844387076, 1.000000000000000000, 0.8660254037844387076, 1.000000000000000000, 0.8660254037844387076, 1.000000000000000000, 0.8660254037844387076, 1.000000000000000000, 0.8660254037844387076, 1.000000000000000000, 0.8660254037844387076, 1.000000000000000000, 0.8660254037844387076, 1.000000000000000000, 0.8660254037844387076, 1.000000000000000000, 0.8660254037844387076, 1.000000000000000000, 0.8660254037844387076, 1.000000000000000000, 0.8660254037844387076, 1.000000000000000000, 0.8660254037844387076, 1.000000000000000000, 0.8660254037844387076, 1.000000000000000000, 0.8660254037844387076, 1.000000000000000000, 0.8660254037844387076, 1.000000000000000000, 0.8660254037844387076, 1.000000000000000000, 0.8660254037844387076, 1.000000000000000000, 0.8660254037844387076, 1.000000000000000000, 0.8660254037844387076, 1.000000000000000000) ) ) 
 REPRESENTATION_ITEM ( '' )  SURFACE ( )  );
#16505 = CARTESIAN_POINT ( 'NONE',  ( 6.196875000614515905, -3.027376345333610441, -5.243569643749999898 ) ) ;
#16506 = CARTESIAN_POINT ( 'NONE',  ( 23.84062500061451928, 6.054752690667223547, 3.707466751127219781E-16 ) ) ;
#16507 = CARTESIAN_POINT ( 'NONE',  ( -1.878215178124999163, 15.15312499938548285, 26.74683588394047007 ) ) ;
#16508 = CARTESIAN_POINT ( 'NONE',  ( 4.648177544792955741E-15, 14.13124999877096322, 33.99999999999999289 ) ) ;
#16509 = CARTESIAN_POINT ( 'NONE',  ( 10.09687500061451715, -3.027376345333614438, 5.243569643749998122 ) ) ;
#16510 = CARTESIAN_POINT ( 'NONE',  ( 34.99999999999999289, -2.499999999999999556, -3.499999999999999556 ) ) ;
#16511 = CARTESIAN_POINT ( 'NONE',  ( 4.096875000614518925, 6.054752690667223547, 3.707466751127219781E-16 ) ) ;
#16512 = CARTESIAN_POINT ( 'NONE',  ( 6.084375000614518747, -4.541064518000419881, 2.621784821874995952 ) ) ;
#16513 = CARTESIAN_POINT ( 'NONE',  ( 29.18437500061451573, 6.421520780324663323E-16, -5.243569643749999010 ) ) ;
#16514 = CARTESIAN_POINT ( 'NONE',  ( 29.11875000122902790, 2.886751345948106007, 5.000000000000033751 ) ) ;
#16515 = CARTESIAN_POINT ( 'NONE',  ( 20.54999999999999716, 0.000000000000000000, 4.999999999999998224 ) ) ;
#16516 = ORIENTED_EDGE ( 'NONE', *, *, #21398, .F. ) ;
#16517 = CARTESIAN_POINT ( 'NONE',  ( 27.44999999999999929, -4.330127018922190985, -2.500000000000001332 ) ) ;
#16518 = CARTESIAN_POINT ( 'NONE',  ( 28.73437500061451644, 6.421520780324663323E-16, -5.243569643749999010 ) ) ;
#16519 = EDGE_CURVE ( 'NONE', #34969, #23351, #37001, .T. ) ;
#16520 = ORIENTED_EDGE ( 'NONE', *, *, #36401, .T. ) ;
#16521 = CARTESIAN_POINT ( 'NONE',  ( 17.24062500061451786, -3.027376345333614438, 5.243569643749998122 ) ) ;
#16522 = CARTESIAN_POINT ( 'NONE',  ( 9.215625000614515727, -6.054752690667223547, -1.112240025338166033E-15 ) ) ;
#16523 = CARTESIAN_POINT ( 'NONE',  ( 20.89687500061451786, -4.119189519843965641, -2.378215178125001383 ) ) ;
#16524 = CARTESIAN_POINT ( 'NONE',  ( 3.909375000614518481, -4.541064518000417216, -2.621784821875001281 ) ) ;
#16525 = CARTESIAN_POINT ( 'NONE',  ( 16.65000000122903501, -2.886751345948129988, 4.999999999999997335 ) ) ;
#16526 = LINE ( 'NONE', #10997, #47301 ) ;
#16527 = CARTESIAN_POINT ( 'NONE',  ( 7.696875000614516793, 6.054752690667223547, 3.707466751127219781E-16 ) ) ;
#16528 = CARTESIAN_POINT ( 'NONE',  ( 11.44687500061451857, -3.027376345333614438, 5.243569643749998122 ) ) ;
#16529 = CARTESIAN_POINT ( 'NONE',  ( 22.02187500061452141, 3.027376345333613106, -5.243569643749998122 ) ) ;
#16530 = CARTESIAN_POINT ( 'NONE',  ( 4.385796401931335353, -2.400997692794667682, 4.385796401931427724 ) ) ;
#16531 = ORIENTED_EDGE ( 'NONE', *, *, #49494, .F. ) ;
#16532 = CARTESIAN_POINT ( 'NONE',  ( 4.359375000614517326, -4.541064518000417216, -2.621784821875001281 ) ) ;
#16533 = CARTESIAN_POINT ( 'NONE',  ( 11.51250000000000107, 2.886751345948126879, 4.999999999999999112 ) ) ;
#16534 = CARTESIAN_POINT ( 'NONE',  ( 7.359375000614516438, 0.000000000000000000, 5.243569643749999010 ) ) ;
#16535 = CARTESIAN_POINT ( 'NONE',  ( 1.878215178125000495, 14.51562499938548356, 26.74683588394047007 ) ) ;
#16536 = CARTESIAN_POINT ( 'NONE',  ( 21.22500000000000142, 6.123233995736764310E-16, -4.999999999999998224 ) ) ;
#16537 = CARTESIAN_POINT ( 'NONE',  ( 18.92812500061451431, 4.541064518000418104, 2.621784821874999949 ) ) ;
#16538 = CARTESIAN_POINT ( 'NONE',  ( -4.000000000000000888, 18.16249999999999787, 32.30940107675850470 ) ) ;
#16539 = CARTESIAN_POINT ( 'NONE',  ( 4.266506403143407233, 2.607457314201153231, 4.357040118942011375 ) ) ;
#16540 = CARTESIAN_POINT ( 'NONE',  ( 23.44687500061451502, 5.492252693125287522, 3.363034840372157021E-16 ) ) ;
#16541 = CARTESIAN_POINT ( 'NONE',  ( 8.953125000614518214, 4.541064518000418104, -2.621784821874998173 ) ) ;
#16542 = CARTESIAN_POINT ( 'NONE',  ( 29.44687500061451857, -3.027376345333614438, 5.243569643749998122 ) ) ;
#16543 = CARTESIAN_POINT ( 'NONE',  ( 28.29375000122902506, -2.886751345948110004, 5.000000000000031974 ) ) ;
#16544 = CARTESIAN_POINT ( 'NONE',  ( 29.37187500061451928, 3.027376345333611329, 5.243569643749999010 ) ) ;
#16545 = CARTESIAN_POINT ( 'NONE',  ( 10.08749999999999858, 5.773502691896255534, 3.535250795749688894E-16 ) ) ;
#16546 = CARTESIAN_POINT ( 'NONE',  ( -2.828200636599751609E-16, 16.40000000122903501, 25.38119784648299770 ) ) ;
#16547 = CARTESIAN_POINT ( 'NONE',  ( 9.600000001229034297, -2.886751345948125991, -5.000000000000000000 ) ) ;
#16548 = CARTESIAN_POINT ( 'NONE',  ( 19.17187500061451999, -6.054752690667223547, -1.112240025338166033E-15 ) ) ;
#16549 = CARTESIAN_POINT ( 'NONE',  ( 13.09687500061451892, 6.054752690667223547, 3.707466751127219781E-16 ) ) ;
#16550 = CARTESIAN_POINT ( 'NONE',  ( 12.00000000000000000, 0.000000000000000000, 4.999999999999998224 ) ) ;
#16551 = ORIENTED_EDGE ( 'NONE', *, *, #41902, .T. ) ;
#16552 = CARTESIAN_POINT ( 'NONE',  ( 15.36562500061451608, 3.027376345333611329, 5.243569643749999010 ) ) ;
#16553 = CARTESIAN_POINT ( 'NONE',  ( 25.72500000122903074, -5.773502691896255534, -1.060575238724906372E-15 ) ) ;
#16554 = CARTESIAN_POINT ( 'NONE',  ( 15.60937500061451644, -4.541064518000417216, -2.621784821875001281 ) ) ;
#16555 = CARTESIAN_POINT ( 'NONE',  ( 5.789369777004289119, 8.154036291478783838, -28.41181880268660009 ) ) ;
#16556 = CARTESIAN_POINT ( 'NONE',  ( 18.25312500061451715, -4.541064518000417216, -2.621784821875001281 ) ) ;
#16557 = EDGE_CURVE ( 'NONE', #63279, #60995, #7233, .T. ) ;
#16558 = CARTESIAN_POINT ( 'NONE',  ( 1.071796769724488785, 20.00134618820329635, 34.00000000000000000 ) ) ;
#16559 = CARTESIAN_POINT ( 'NONE',  ( 25.99687500061451928, -3.027376345333610441, -5.243569643749999898 ) ) ;
#16560 = CARTESIAN_POINT ( 'NONE',  ( 4.243569643749999898, 10.54062500061451679, 32.45002607614398471 ) ) ;
#16561 = CARTESIAN_POINT ( 'NONE',  ( 15.38437500061451679, 4.541064518000418104, 2.621784821874999949 ) ) ;
#16562 = CARTESIAN_POINT ( 'NONE',  ( 15.00000000122903465, -2.886751345948125991, -5.000000000000000000 ) ) ;
#16563 = CARTESIAN_POINT ( 'NONE',  ( 8.559375000614515727, 4.119189519843966529, -2.378215178124998275 ) ) ;
#16564 = CARTESIAN_POINT ( 'NONE',  ( 2.121784821875001281, 18.65937500061451715, -26.32496088578401938 ) ) ;
#16565 = CARTESIAN_POINT ( 'NONE',  ( 20.48437500061451289, -4.541064518000419881, 2.621784821874995952 ) ) ;
#16566 = CARTESIAN_POINT ( 'NONE',  ( 20.73750000122903359, -4.330127018922194537, 2.499999999999995559 ) ) ;
#16567 = CARTESIAN_POINT ( 'NONE',  ( 17.07187500061451502, 3.027376345333613106, -5.243569643749998122 ) ) ;
#16568 = CARTESIAN_POINT ( 'NONE',  ( 9.001249775931846008E-16, 12.32187500061451857, 34.90005215228797653 ) ) ;
#16569 = CARTESIAN_POINT ( 'NONE',  ( 16.64062500061451289, 6.054752690667223547, 3.707466751127219781E-16 ) ) ;
#16570 = ORIENTED_EDGE ( 'NONE', *, *, #8132, .F. ) ;
#16571 = ORIENTED_EDGE ( 'NONE', *, *, #13710, .F. ) ;
#16572 = CARTESIAN_POINT ( 'NONE',  ( 20.51249999999999929, 2.886751345948126879, 4.999999999999999112 ) ) ;
#16573 = CARTESIAN_POINT ( 'NONE',  ( 45.00000000000000000, 0.000000000000000000, 0.000000000000000000 ) ) ;
#16574 = CARTESIAN_POINT ( 'NONE',  ( 23.39062500061451289, 6.054752690667223547, 3.707466751127219781E-16 ) ) ;
#16575 = CARTESIAN_POINT ( 'NONE',  ( 3.928125000614516527, 6.421520780324663323E-16, -5.243569643749999010 ) ) ;
#16576 = CARTESIAN_POINT ( 'NONE',  ( 17.51250000122903216, 0.000000000000000000, 4.999999999999998224 ) ) ;
#16577 = CARTESIAN_POINT ( 'NONE',  ( 22.90312500061451573, 4.541064518000418104, -2.621784821874998173 ) ) ;
#16578 = CARTESIAN_POINT ( 'NONE',  ( 21.52499999999999858, -4.330127018922194537, 2.499999999999995559 ) ) ;
#16579 = CARTESIAN_POINT ( 'NONE',  ( 25.67812500061451431, 4.541064518000418104, 2.621784821874999949 ) ) ;
#16580 = CARTESIAN_POINT ( 'NONE',  ( 5.278125000614516615, 6.421520780324663323E-16, -5.243569643749999010 ) ) ;
#16581 = ORIENTED_EDGE ( 'NONE', *, *, #58905, .F. ) ;
#16582 = CARTESIAN_POINT ( 'NONE',  ( 29.92500000000000071, 4.330127018922191873, 2.499999999999999556 ) ) ;
#16583 = CARTESIAN_POINT ( 'NONE',  ( 2.840625000614518392, -3.027376345333614438, 5.243569643749998122 ) ) ;
#16584 = CARTESIAN_POINT ( 'NONE',  ( 11.70937500061451608, 4.119189519843966529, -2.378215178124998275 ) ) ;
#16585 = CARTESIAN_POINT ( 'NONE',  ( -2.000000000000000000, 11.03750000122903430, 26.53589838486224650 ) ) ;
#16586 = CARTESIAN_POINT ( 'NONE',  ( -2.828200636599751609E-16, 11.90000000122903501, -34.61880215351700230 ) ) ;
#16587 = CARTESIAN_POINT ( 'NONE',  ( -4.243569643749999898, 19.37187500061451928, -32.45002607614398471 ) ) ;
#16588 = CARTESIAN_POINT ( 'NONE',  ( 8.175000000000002487, 6.123233995736764310E-16, -4.999999999999998224 ) ) ;
#16589 = CARTESIAN_POINT ( 'NONE',  ( 5.700000001229033941, 5.773502691896255534, 3.535250795749688894E-16 ) ) ;
#16590 = CARTESIAN_POINT ( 'NONE',  ( 12.04687500061451821, -3.027376345333610441, -5.243569643749999898 ) ) ;
#16591 = CARTESIAN_POINT ( 'NONE',  ( 29.69062500061451715, 6.054752690667223547, 3.707466751127219781E-16 ) ) ;
#16592 = CARTESIAN_POINT ( 'NONE',  ( 4.284375000614518925, -4.541064518000419881, 2.621784821874995952 ) ) ;
#16593 = CARTESIAN_POINT ( 'NONE',  ( 2.000000000000001332, 18.91250000122903430, 33.46410161513774995 ) ) ;
#16594 = DIRECTION ( 'NONE',  ( -1.000000000000000000, -0.000000000000000000, -0.000000000000000000 ) ) ;
#16595 = CARTESIAN_POINT ( 'NONE',  ( 9.346875000614517148, -3.027376345333610441, -5.243569643749999898 ) ) ;
#16596 = CARTESIAN_POINT ( 'NONE',  ( 1.071796769724489895, 14.12990381179669797, -34.00000000000000000 ) ) ;
#16597 = CARTESIAN_POINT ( 'NONE',  ( 19.64062500061451644, -3.027376345333610441, -5.243569643749999898 ) ) ;
#16598 = CARTESIAN_POINT ( 'NONE',  ( 30.00000000000000000, 6.123233995736764310E-16, -4.999999999999998224 ) ) ;
#16599 = CARTESIAN_POINT ( 'NONE',  ( 2.121784821874999061, 18.30312500061459602, 26.32496088578401583 ) ) ;
#16600 = CARTESIAN_POINT ( 'NONE',  ( 22.84687500061451715, -3.027376345333610441, -5.243569643749999898 ) ) ;
#16601 = DIRECTION ( 'NONE',  ( 0.000000000000000000, 0.000000000000000000, -1.000000000000000000 ) ) ;
#16602 = CARTESIAN_POINT ( 'NONE',  ( 3.215625000614518836, 3.027376345333611329, 5.243569643749999010 ) ) ;
#16603 = CARTESIAN_POINT ( 'NONE',  ( 19.13437500061451502, -2.746126346562642428, -4.756430356249999214 ) ) ;
#16604 = CARTESIAN_POINT ( 'NONE',  ( 24.06562500061451715, -6.054752690667223547, -1.112240025338166033E-15 ) ) ;
#16605 = CARTESIAN_POINT ( 'NONE',  ( 14.69062500061451537, -3.027376345333610441, -5.243569643749999898 ) ) ;
#16606 = CARTESIAN_POINT ( 'NONE',  ( 14.38125000122903252, -4.330127018922194537, 2.499999999999995559 ) ) ;
#16607 = CARTESIAN_POINT ( 'NONE',  ( 12.08437500061451608, 6.421520780324663323E-16, -5.243569643749999010 ) ) ;
#16608 = CARTESIAN_POINT ( 'NONE',  ( 1.626862140677534470E-15, 12.83750000000000213, 34.00000000000000000 ) ) ;
#16609 = CARTESIAN_POINT ( 'NONE',  ( 25.08750000122903145, 4.330127018922191873, 2.499999999999999556 ) ) ;
#16610 = CARTESIAN_POINT ( 'NONE',  ( 3.984375000614517326, 6.421520780324663323E-16, -5.243569643749999010 ) ) ;
#16611 = CARTESIAN_POINT ( 'NONE',  ( 14.55937500061451573, 0.000000000000000000, 5.243569643749999010 ) ) ;
#16612 = CARTESIAN_POINT ( 'NONE',  ( 29.82187500061451502, 3.027376345333611329, 5.243569643749999010 ) ) ;
#16613 = CARTESIAN_POINT ( 'NONE',  ( 21.75000000000000000, 4.330127018922192761, -2.499999999999997780 ) ) ;
#16614 = DIRECTION ( 'NONE',  ( 0.000000000000000000, 0.000000000000000000, 1.000000000000000000 ) ) ;
#16615 = CARTESIAN_POINT ( 'NONE',  ( 24.42187500061451999, 3.027376345333611329, 5.243569643749999010 ) ) ;
#16616 = CARTESIAN_POINT ( 'NONE',  ( 14.37187500061451928, 3.027376345333613106, -5.243569643749998122 ) ) ;
#16617 = CARTESIAN_POINT ( 'NONE',  ( 3.756430356250000102, 15.45312499938548356, 30.00000000000000000 ) ) ;
#16618 = CARTESIAN_POINT ( 'NONE',  ( 29.36250000000000071, 2.886751345948129099, -4.999999999999998224 ) ) ;
#16619 = CARTESIAN_POINT ( 'NONE',  ( 4.012500001229033053, 0.000000000000000000, 4.999999999999998224 ) ) ;
#16620 = CARTESIAN_POINT ( 'NONE',  ( 5.325000000000000178, -4.330127018922194537, 2.499999999999995559 ) ) ;
#16621 = CARTESIAN_POINT ( 'NONE',  ( 29.55937500061451573, -4.119189519843965641, -2.378215178125001383 ) ) ;
#16622 = CARTESIAN_POINT ( 'NONE',  ( 19.22812500061451502, 6.421520780324663323E-16, -5.243569643749999010 ) ) ;
#16623 = CARTESIAN_POINT ( 'NONE',  ( 10.31250000000000355, -5.773502691896255534, -1.060575238724906372E-15 ) ) ;
#16624 = EDGE_CURVE ( 'NONE', #6077, #19923, #72580, .T. ) ;
#16625 = CARTESIAN_POINT ( 'NONE',  ( 15.52500000000000036, 4.330127018922191873, 2.499999999999999556 ) ) ;
#16626 = CARTESIAN_POINT ( 'NONE',  ( 17.21249999999999858, 2.886751345948129099, -4.999999999999998224 ) ) ;
#16627 = CARTESIAN_POINT ( 'NONE',  ( -2.121784821874999949, 11.62812500061451715, 26.32496088578401938 ) ) ;
#16628 = DIRECTION ( 'NONE',  ( -1.000000000000000000, -0.000000000000000000, -0.000000000000000000 ) ) ;
#16629 = CARTESIAN_POINT ( 'NONE',  ( 19.65000000122902790, 5.773502691896255534, 3.535250795749688894E-16 ) ) ;
#16630 = CARTESIAN_POINT ( 'NONE',  ( 30.00000000000000000, 6.123233995736764310E-16, -4.999999999999998224 ) ) ;
#16631 = CARTESIAN_POINT ( 'NONE',  ( 27.53437500061451360, 4.541064518000418104, 2.621784821874999949 ) ) ;
#16632 = ORIENTED_EDGE ( 'NONE', *, *, #3173, .F. ) ;
#16633 = CARTESIAN_POINT ( 'NONE',  ( 15.96562500061451573, -6.054752690667223547, -1.112240025338166033E-15 ) ) ;
#16634 = CARTESIAN_POINT ( 'NONE',  ( 22.94062500061451715, 6.054752690667223547, 3.707466751127219781E-16 ) ) ;
#16635 = CARTESIAN_POINT ( 'NONE',  ( 22.05937500061451573, 4.541064518000418104, -2.621784821874998173 ) ) ;
#16636 = CARTESIAN_POINT ( 'NONE',  ( 7.387500000000001066, 5.773502691896255534, 3.535250795749688894E-16 ) ) ;
#16637 = CARTESIAN_POINT ( 'NONE',  ( 10.45312500061451644, 0.000000000000000000, 5.243569643749999010 ) ) ;
#16638 = CARTESIAN_POINT ( 'NONE',  ( 25.07812500061451644, 6.421520780324663323E-16, -5.243569643749999010 ) ) ;
#16639 = CARTESIAN_POINT ( 'NONE',  ( 13.65937500061451715, 0.000000000000000000, 5.243569643749999010 ) ) ;
#16640 = CARTESIAN_POINT ( 'NONE',  ( 18.27187500061451431, -6.054752690667223547, -1.112240025338166033E-15 ) ) ;
#16641 = DIRECTION ( 'NONE',  ( -1.000000000000000000, -0.000000000000000000, -0.000000000000000000 ) ) ;
#16642 = CARTESIAN_POINT ( 'NONE',  ( 4.243569643749999010, 18.71562500061451217, 27.54997392385601174 ) ) ;
#16643 = CARTESIAN_POINT ( 'NONE',  ( 20.51250000122903216, 4.330127018922192761, -2.499999999999997780 ) ) ;
#16644 = CARTESIAN_POINT ( 'NONE',  ( 16.73437500061451644, 4.119189519843966529, 2.378215178124999607 ) ) ;
#16645 = CARTESIAN_POINT ( 'NONE',  ( 11.61562500061451608, 3.027376345333612662, -5.243569643749998122 ) ) ;
#16646 = CARTESIAN_POINT ( 'NONE',  ( 5.596875000614516260, -3.027376345333614438, 5.243569643749998122 ) ) ;
#16647 = CARTESIAN_POINT ( 'NONE',  ( 6.009375000614519458, 0.000000000000000000, 5.243569643749999010 ) ) ;
#16648 = VERTEX_POINT ( 'NONE', #50776 ) ;
#16649 = CARTESIAN_POINT ( 'NONE',  ( 26.85937500061451644, -4.541064518000417216, -2.621784821875001281 ) ) ;
#16650 = CARTESIAN_POINT ( 'NONE',  ( 18.47812500061451857, 4.541064518000418104, 2.621784821874999949 ) ) ;
#16651 = CARTESIAN_POINT ( 'NONE',  ( 3.928125000614516527, 6.421520780324663323E-16, -5.243569643749999010 ) ) ;
#16652 = CARTESIAN_POINT ( 'NONE',  ( 27.32812500061451644, 6.421520780324663323E-16, -5.243569643749999010 ) ) ;
#16653 = CARTESIAN_POINT ( 'NONE',  ( 23.10937500061451644, 0.000000000000000000, 5.243569643749999010 ) ) ;
#16654 = CARTESIAN_POINT ( 'NONE',  ( 20.24062500061451431, 6.054752690667223547, 3.707466751127219781E-16 ) ) ;
#16655 = CARTESIAN_POINT ( 'NONE',  ( -4.243569643749999898, 18.92187500061451644, 27.54997392385601529 ) ) ;
#16656 = CARTESIAN_POINT ( 'NONE',  ( 24.74062500061451786, 6.054752690667223547, 3.707466751127219781E-16 ) ) ;
#16657 = CARTESIAN_POINT ( 'NONE',  ( 5.025000001229035895, -5.773502691896255534, -1.060575238724906372E-15 ) ) ;
#16658 = VERTEX_POINT ( 'NONE', #16415 ) ;
#16659 = CARTESIAN_POINT ( 'NONE',  ( 27.11249999999999716, 2.886751345948129099, -4.999999999999998224 ) ) ;
#16660 = CARTESIAN_POINT ( 'NONE',  ( 2.000000000000001332, 14.75000000000000178, -26.53589838486224650 ) ) ;
#16661 = CARTESIAN_POINT ( 'NONE',  ( 3.756430356250000102, 17.25312499938548072, 30.00000000000000000 ) ) ;
#16662 = CARTESIAN_POINT ( 'NONE',  ( 5.521875000614517859, 3.027376345333611329, 5.243569643749999010 ) ) ;
#16663 = CARTESIAN_POINT ( 'NONE',  ( 12.92812500061451786, 6.421520780324663323E-16, -5.243569643749999010 ) ) ;
#16664 = CARTESIAN_POINT ( 'NONE',  ( 6.759375000614516793, 4.541064518000418104, -2.621784821874998173 ) ) ;
#16665 = CARTESIAN_POINT ( 'NONE',  ( 23.51250000122903216, -4.330127018922190985, -2.500000000000001332 ) ) ;
#16666 = CARTESIAN_POINT ( 'NONE',  ( 15.75937500061451857, 4.541064518000418104, -2.621784821874998173 ) ) ;
#16667 = CARTESIAN_POINT ( 'NONE',  ( 29.35312500061451502, 0.000000000000000000, 5.243569643749999010 ) ) ;
#16668 = CARTESIAN_POINT ( 'NONE',  ( 27.44999999999999929, -4.330127018922190985, -2.500000000000001332 ) ) ;
#16669 = CARTESIAN_POINT ( 'NONE',  ( 26.93437500061451573, 6.421520780324663323E-16, -5.243569643749999010 ) ) ;
#16670 = CARTESIAN_POINT ( 'NONE',  ( 3.853125000614517681, -4.541064518000417216, -2.621784821875001281 ) ) ;
#16671 = CARTESIAN_POINT ( 'NONE',  ( 12.25312500061451537, 0.000000000000000000, 5.243569643749999010 ) ) ;
#16672 = VERTEX_POINT ( 'NONE', #16777 ) ;
#16673 = CARTESIAN_POINT ( 'NONE',  ( 9.365625000614519635, 3.027376345333613106, -5.243569643749998122 ) ) ;
#16674 = CARTESIAN_POINT ( 'NONE',  ( 6.140625000614516438, -3.027376345333610441, -5.243569643749999898 ) ) ;
#16675 = CARTESIAN_POINT ( 'NONE',  ( 18.45937500061451431, 4.119189519843966529, -2.378215178124998275 ) ) ;
#16676 = EDGE_CURVE ( 'NONE', #26352, #47876, #49691, .T. ) ;
#16677 = DIRECTION ( 'NONE',  ( 0.000000000000000000, 0.000000000000000000, -1.000000000000000000 ) ) ;
#16678 = EDGE_CURVE ( 'NONE', #26340, #39358, #24271, .T. ) ;
#16679 = CARTESIAN_POINT ( 'NONE',  ( 15.22500000000000142, -4.330127018922194537, 2.499999999999995559 ) ) ;
#16680 = CARTESIAN_POINT ( 'NONE',  ( 15.57187500061451679, -6.054752690667223547, -1.112240025338166033E-15 ) ) ;
#16681 = CARTESIAN_POINT ( 'NONE',  ( 12.67500000122903536, -5.773502691896255534, -1.060575238724906372E-15 ) ) ;
#16682 = CARTESIAN_POINT ( 'NONE',  ( 19.12500000000000000, 4.330127018922191873, 2.499999999999999556 ) ) ;
#16683 = CARTESIAN_POINT ( 'NONE',  ( 21.94687500061451857, -3.027376345333610441, -5.243569643749999898 ) ) ;
#16684 = CARTESIAN_POINT ( 'NONE',  ( 2.121784821874999061, 13.80312500061451786, -33.67503911421598417 ) ) ;
#16685 = DIRECTION ( 'NONE',  ( -0.000000000000000000, -1.000000000000000000, 8.673617379884035472E-17 ) ) ;
#16686 = CARTESIAN_POINT ( 'NONE',  ( 25.50937500061451502, 2.746126346562645981, -4.756430356249997438 ) ) ;
#16687 = CARTESIAN_POINT ( 'NONE',  ( 20.58749999999999858, -2.886751345948096681, 5.000000000000054179 ) ) ;
#16688 = CARTESIAN_POINT ( 'NONE',  ( 25.79062500061451502, -3.027376345333614438, 5.243569643749998122 ) ) ;
#16689 = CARTESIAN_POINT ( 'NONE',  ( -3.999999999999999112, 19.51250000000000284, -32.30940107675850470 ) ) ;
#16690 = DIRECTION ( 'NONE',  ( 0.000000000000000000, 1.000000000000000000, 0.000000000000000000 ) ) ;
#16691 = CARTESIAN_POINT ( 'NONE',  ( 25.57499999999999929, -4.330127018922194537, 2.499999999999995559 ) ) ;
#16692 = CARTESIAN_POINT ( 'NONE',  ( 9.140625000614518214, -3.027376345333614438, 5.243569643749998122 ) ) ;
#16693 = CARTESIAN_POINT ( 'NONE',  ( 28.02187500061451431, -4.119189519843968306, 2.378215178124996054 ) ) ;
#16694 = CARTESIAN_POINT ( 'NONE',  ( 21.49687500061451573, -3.027376345333610441, -5.243569643749999898 ) ) ;
#16695 = CARTESIAN_POINT ( 'NONE',  ( 13.50937500061451679, 2.746126346562643317, 4.756430356249998326 ) ) ;
#16696 = CARTESIAN_POINT ( 'NONE',  ( 5.765625000614519102, 3.027376345333613106, -5.243569643749998122 ) ) ;
#16697 = CARTESIAN_POINT ( 'NONE',  ( 11.25937500061451679, 4.541064518000418104, -2.621784821874998173 ) ) ;
#16698 = ORIENTED_EDGE ( 'NONE', *, *, #25145, .F. ) ;
#16699 = CARTESIAN_POINT ( 'NONE',  ( 20.85937500061451644, 0.000000000000000000, 5.243569643749999010 ) ) ;
#16700 = FACE_OUTER_BOUND ( 'NONE', #45989, .T. ) ;
#16701 = CARTESIAN_POINT ( 'NONE',  ( 29.69999999999999574, -4.330127018922190985, -2.500000000000001332 ) ) ;
#16702 = EDGE_CURVE ( 'NONE', #71801, #46607, #27091, .T. ) ;
#16703 = CARTESIAN_POINT ( 'NONE',  ( 3.937500000000000444, -2.886751345948129988, 4.999999999999997335 ) ) ;
#16704 = CARTESIAN_POINT ( 'NONE',  ( 15.71250000122903501, 0.000000000000000000, 4.999999999999998224 ) ) ;
#16705 = CARTESIAN_POINT ( 'NONE',  ( 20.71875000122903288, -5.773502691896255534, -1.060575238724906372E-15 ) ) ;
#16706 = CARTESIAN_POINT ( 'NONE',  ( -3.999999999999999112, 19.06250000000000000, -32.30940107675850470 ) ) ;
#16707 = PRODUCT_DEFINITION_FORMATION_WITH_SPECIFIED_SOURCE ( 'ANY', '', #14280, .NOT_KNOWN. ) ;
#16708 = ORIENTED_EDGE ( 'NONE', *, *, #12168, .F. ) ;
#16709 = CARTESIAN_POINT ( 'NONE',  ( 12.78749999999999964, 5.773502691896255534, 3.535250795749688894E-16 ) ) ;
#16710 = CARTESIAN_POINT ( 'NONE',  ( 26.95312500061451644, 4.541064518000418104, -2.621784821874998173 ) ) ;
#16711 = CARTESIAN_POINT ( 'NONE',  ( 16.31250000000000000, 2.886751345948129099, -4.999999999999998224 ) ) ;
#16712 = CARTESIAN_POINT ( 'NONE',  ( 9.525000001229033231, -5.773502691896255534, -1.060575238724906372E-15 ) ) ;
#16713 = CARTESIAN_POINT ( 'NONE',  ( 8.428125000614517859, 6.421520780324663323E-16, -5.243569643749999010 ) ) ;
#16714 =( BOUNDED_CURVE ( )  B_SPLINE_CURVE ( 2, ( #58392, #45532, #59125, #32169, #14435, #9269, #53599 ),
 .UNSPECIFIED., .F., .F. ) 
 B_SPLINE_CURVE_WITH_KNOTS ( ( 3, 2, 2, 3 ),
 ( 0.8800000000000000044, 0.8833333333333333037, 0.8866666666666667140, 0.8900000000000000133 ),
 .UNSPECIFIED. ) 
 CURVE ( )  GEOMETRIC_REPRESENTATION_ITEM ( )  RATIONAL_B_SPLINE_CURVE ( ( 1.000000000000000000, 0.8660254037844387076, 1.000000000000000000, 0.8660254037844387076, 1.000000000000000000, 0.8660254037844387076, 1.000000000000000000 ) ) 
 REPRESENTATION_ITEM ( '' )  );
#16715 = CARTESIAN_POINT ( 'NONE',  ( 8.474999999999999645, -4.330127018922194537, 2.499999999999995559 ) ) ;
#16716 = CARTESIAN_POINT ( 'NONE',  ( -1.071796769724488563, 11.09240381056766545, -26.00000000000000000 ) ) ;
#16717 = CARTESIAN_POINT ( 'NONE',  ( 2.121784821874999061, 14.30937500061451750, -33.67503911421598417 ) ) ;
#16718 = CARTESIAN_POINT ( 'NONE',  ( 28.08750000122903145, 6.123233995736764310E-16, -4.999999999999998224 ) ) ;
#16719 = CARTESIAN_POINT ( 'NONE',  ( 2.655984681222220721E-16, 15.90312499938548108, 25.66244784525396483 ) ) ;
#16720 = CARTESIAN_POINT ( 'NONE',  ( 8.324999999999999289, 4.330127018922191873, 2.499999999999999556 ) ) ;
#16721 = CARTESIAN_POINT ( 'NONE',  ( 0.000000000000000000, 20.00000000000000000, 26.00000000000000000 ) ) ;
#16722 = ORIENTED_EDGE ( 'NONE', *, *, #19527, .F. ) ;
#16723 = CARTESIAN_POINT ( 'NONE',  ( 23.95312500061451289, 0.000000000000000000, 5.243569643749999010 ) ) ;
#16724 = FACE_OUTER_BOUND ( 'NONE', #45975, .T. ) ;
#16725 = CARTESIAN_POINT ( 'NONE',  ( 14.58750000122903323, 6.123233995736764310E-16, -4.999999999999998224 ) ) ;
#16726 = CARTESIAN_POINT ( 'NONE',  ( 22.28437500061451715, -4.541064518000419881, 2.621784821874995952 ) ) ;
#16727 = CARTESIAN_POINT ( 'NONE',  ( 15.55312500061451608, -4.541064518000417216, -2.621784821875001281 ) ) ;
#16728 = CARTESIAN_POINT ( 'NONE',  ( 4.243569643749999898, 10.54062500061459318, -27.54997392385601529 ) ) ;
#16729 = CARTESIAN_POINT ( 'NONE',  ( 6.703125000614516438, 4.541064518000418104, -2.621784821874998173 ) ) ;
#16730 = CARTESIAN_POINT ( 'NONE',  ( 27.93750000122903288, -4.330127018922194537, 2.499999999999995559 ) ) ;
#16731 = CARTESIAN_POINT ( 'NONE',  ( 23.29687500061451644, -2.746126346562641984, -4.756430356249999214 ) ) ;
#16732 = CARTESIAN_POINT ( 'NONE',  ( 19.64062500061451644, -3.027376345333610441, -5.243569643749999898 ) ) ;
#16733 = DIRECTION ( 'NONE',  ( 1.000000000000000000, -0.000000000000000000, 0.000000000000000000 ) ) ;
#16734 = CARTESIAN_POINT ( 'NONE',  ( -3.756430356250001434, 19.65312499938548640, 32.16877607737301048 ) ) ;
#16735 = CARTESIAN_POINT ( 'NONE',  ( 13.69687500061451679, -3.027376345333614438, 5.243569643749998122 ) ) ;
#16736 = CARTESIAN_POINT ( 'NONE',  ( 13.47187500061451537, 3.027376345333613106, -5.243569643749998122 ) ) ;
#16737 = CARTESIAN_POINT ( 'NONE',  ( 22.28437500061451715, -4.541064518000419881, 2.621784821874995952 ) ) ;
#16738 = VERTEX_POINT ( 'NONE', #21229 ) ;
#16739 = CARTESIAN_POINT ( 'NONE',  ( 19.98749999999999716, 5.773502691896255534, 3.535250795749688401E-16 ) ) ;
#16740 = CARTESIAN_POINT ( 'NONE',  ( 26.09062500061451573, 6.054752690667223547, 3.707466751127219781E-16 ) ) ;
#16741 = CARTESIAN_POINT ( 'NONE',  ( 27.47812500061451502, 4.541064518000418104, 2.621784821874999949 ) ) ;
#16742 = CARTESIAN_POINT ( 'NONE',  ( 14.98125000122903216, 6.123233995736764310E-16, -4.999999999999998224 ) ) ;
#16743 = CARTESIAN_POINT ( 'NONE',  ( 2.000000000000001332, 17.44999999999999929, 33.46410161513774995 ) ) ;
#16744 = CARTESIAN_POINT ( 'NONE',  ( 5.034375000614519813, 4.541064518000418104, 2.621784821874999949 ) ) ;
#16745 = CARTESIAN_POINT ( 'NONE',  ( 13.01250000122903394, 0.000000000000000000, 4.999999999999998224 ) ) ;
#16746 = CARTESIAN_POINT ( 'NONE',  ( 6.075000001229034829, 2.886751345948129099, -4.999999999999998224 ) ) ;
#16747 = CARTESIAN_POINT ( 'NONE',  ( 28.80000000122903003, -2.886751345948129988, 4.999999999999997335 ) ) ;
#16748 = CARTESIAN_POINT ( 'NONE',  ( 3.999999999999998668, 18.25624999877096499, 32.30940107675850470 ) ) ;
#16749 = CARTESIAN_POINT ( 'NONE',  ( 18.80625000122903501, 0.000000000000000000, 4.999999999999998224 ) ) ;
#16750 = CARTESIAN_POINT ( 'NONE',  ( 10.77187500061451786, 3.027376345333613106, -5.243569643749998122 ) ) ;
#16751 = CYLINDRICAL_SURFACE ( 'NONE', #43208, 4.999999999999998224 ) ;
#16752 = ORIENTED_EDGE ( 'NONE', *, *, #68046, .T. ) ;
#16753 = CARTESIAN_POINT ( 'NONE',  ( 20.12812500061451715, 6.421520780324663323E-16, -5.243569643749999010 ) ) ;
#16754 = CARTESIAN_POINT ( 'NONE',  ( 13.73437500061451821, -4.541064518000419881, 2.621784821874995952 ) ) ;
#16755 = CARTESIAN_POINT ( 'NONE',  ( 4.153125000614515727, 0.000000000000000000, 5.243569643749999010 ) ) ;
#16756 = CARTESIAN_POINT ( 'NONE',  ( 22.13437500061451502, 4.541064518000418104, 2.621784821874999949 ) ) ;
#16757 = CARTESIAN_POINT ( 'NONE',  ( 10.13437500061451679, -4.541064518000419881, 2.621784821874995952 ) ) ;
#16758 = CARTESIAN_POINT ( 'NONE',  ( 4.153125000614515727, 0.000000000000000000, 5.243569643749999010 ) ) ;
#16759 = DIRECTION ( 'NONE',  ( -0.000000000000000000, -1.000000000000000000, -0.000000000000000000 ) ) ;
#16760 = CARTESIAN_POINT ( 'NONE',  ( 5.962500001229033231, -4.330127018922190985, -2.500000000000001332 ) ) ;
#16761 = CARTESIAN_POINT ( 'NONE',  ( 20.87812500061451715, -4.541064518000419881, 2.621784821874995952 ) ) ;
#16762 = CARTESIAN_POINT ( 'NONE',  ( 8.700000001229032165, -2.886751345948125991, -5.000000000000000000 ) ) ;
#16763 = CARTESIAN_POINT ( 'NONE',  ( 17.84062500061451573, -3.027376345333610441, -5.243569643749999898 ) ) ;
#16764 = CARTESIAN_POINT ( 'NONE',  ( 16.15312500061451573, 4.541064518000418104, -2.621784821874998173 ) ) ;
#16765 = CARTESIAN_POINT ( 'NONE',  ( 24.79687500061451999, 5.492252693125287522, 3.363034840372157021E-16 ) ) ;
#16766 = CARTESIAN_POINT ( 'NONE',  ( 15.15000000000000036, 0.000000000000000000, 4.999999999999998224 ) ) ;
#16767 = CARTESIAN_POINT ( 'NONE',  ( 8.362500001229031810, 4.330127018922192761, -2.499999999999997780 ) ) ;
#16768 = CARTESIAN_POINT ( 'NONE',  ( 5.353125000614515905, 4.541064518000418104, -2.621784821874998173 ) ) ;
#16769 = AXIS2_PLACEMENT_3D ( 'NONE', #17122, #16759, #68469 ) ;
#16770 = CARTESIAN_POINT ( 'NONE',  ( 19.87500000122903288, -5.773502691896255534, -1.060575238724906372E-15 ) ) ;
#16771 = CARTESIAN_POINT ( 'NONE',  ( 27.71250000000000568, 2.886751345948126879, 4.999999999999999112 ) ) ;
#16772 = CARTESIAN_POINT ( 'NONE',  ( -4.243569643749997233, 9.996875000614517504, -27.54997392385601174 ) ) ;
#16773 = CARTESIAN_POINT ( 'NONE',  ( 5.000000000000000888, 2.882564675336284927E-11, 5.151554443534156036 ) ) ;
#16774 = CARTESIAN_POINT ( 'NONE',  ( 45.00000000000000000, 6.363961030679004871, 6.363961030678849440 ) ) ;
#16775 = CARTESIAN_POINT ( 'NONE',  ( 3.534375000614518036, 6.421520780324663323E-16, -5.243569643749999010 ) ) ;
#16776 = CARTESIAN_POINT ( 'NONE',  ( 20.67187500061451289, 3.027376345333613106, -5.243569643749998122 ) ) ;
#16777 = CARTESIAN_POINT ( 'NONE',  ( -1.243387493232115393E-14, 14.86250000000000071, 26.00000000000000000 ) ) ;
#16778 = CARTESIAN_POINT ( 'NONE',  ( 17.31562500061451715, -6.054752690667223547, -1.112240025338166033E-15 ) ) ;
#16779 = CARTESIAN_POINT ( 'NONE',  ( 12.09375000122903465, -2.886751345948129988, 4.999999999999997335 ) ) ;
#16780 = CARTESIAN_POINT ( 'NONE',  ( 13.31250000000000178, 2.886751345948126879, 4.999999999999998224 ) ) ;
#16781 = CARTESIAN_POINT ( 'NONE',  ( 26.81250000000000355, 2.886751345948135317, 4.999999999999984013 ) ) ;
#16782 = CARTESIAN_POINT ( 'NONE',  ( 28.02187500061451431, 3.027376345333611329, 5.243569643749999010 ) ) ;
#16783 = CARTESIAN_POINT ( 'NONE',  ( 20.85937500061451644, -5.492252693125287522, -1.008910452111647106E-15 ) ) ;
#16784 = CARTESIAN_POINT ( 'NONE',  ( 13.60312500061451679, 0.000000000000000000, 5.243569643749999010 ) ) ;
#16785 = CARTESIAN_POINT ( 'NONE',  ( 10.54687500061451644, -3.027376345333614438, 5.243569643749998122 ) ) ;
#16786 = VERTEX_POINT ( 'NONE', #15685 ) ;
#16787 = CARTESIAN_POINT ( 'NONE',  ( -2.000000000000000000, 14.07500000000000107, -33.46410161513775705 ) ) ;
#16788 = CARTESIAN_POINT ( 'NONE',  ( 23.20312500061451644, -4.541064518000417216, -2.621784821875001281 ) ) ;
#16789 = CARTESIAN_POINT ( 'NONE',  ( 17.51250000122903216, 0.000000000000000000, 4.999999999999998224 ) ) ;
#16790 = CARTESIAN_POINT ( 'NONE',  ( 20.92500000000000071, 4.330127018922191873, 2.499999999999999556 ) ) ;
#16791 = EDGE_CURVE ( 'NONE', #16738, #48333, #18211, .T. ) ;
#16792 = CARTESIAN_POINT ( 'NONE',  ( 11.32500000000000107, 6.123233995736764310E-16, -4.999999999999998224 ) ) ;
#16793 = CARTESIAN_POINT ( 'NONE',  ( 22.95000000122903216, -2.886751345948129988, 4.999999999999997335 ) ) ;
#16794 = CARTESIAN_POINT ( 'NONE',  ( 17.20312500061451644, 0.000000000000000000, 5.243569643749999010 ) ) ;
#16795 = CARTESIAN_POINT ( 'NONE',  ( 12.38437500061451502, -2.746126346562642428, -4.756430356249999214 ) ) ;
#16796 = ORIENTED_EDGE ( 'NONE', *, *, #54938, .F. ) ;
#16797 = CARTESIAN_POINT ( 'NONE',  ( 19.91250000000000142, 2.886751345948129099, -4.999999999999998224 ) ) ;
#16798 = CARTESIAN_POINT ( 'NONE',  ( 24.97499999999999787, 4.330127018922191873, 2.499999999999999556 ) ) ;
#16799 = CARTESIAN_POINT ( 'NONE',  ( 20.29687500061451644, 6.054752690667223547, 3.707466751127219781E-16 ) ) ;
#16800 = CARTESIAN_POINT ( 'NONE',  ( 28.19062500061451715, -3.027376345333610441, -5.243569643749999898 ) ) ;
#16801 = EDGE_CURVE ( 'NONE', #36412, #38182, #59644, .T. ) ;
#16802 = EDGE_LOOP ( 'NONE', ( #62939, #37394, #44312, #42136 ) ) ;
#16803 = LINE ( 'NONE', #56345, #2966 ) ;
#16804 = CARTESIAN_POINT ( 'NONE',  ( 8.915625000614515017, 3.027376345333613106, -5.243569643749998122 ) ) ;
#16805 = CARTESIAN_POINT ( 'NONE',  ( 12.37500000000000000, 4.330127018922191873, 2.499999999999999556 ) ) ;
#16806 = CARTESIAN_POINT ( 'NONE',  ( 15.22500000000000142, -4.330127018922194537, 2.499999999999995559 ) ) ;
#16807 = CARTESIAN_POINT ( 'NONE',  ( -2.121784821874996840, 19.42812500061451786, 33.67503911421598417 ) ) ;
#16808 = CARTESIAN_POINT ( 'NONE',  ( 4.921875000614518214, 3.027376345333613106, -5.243569643749998122 ) ) ;
#16809 = CARTESIAN_POINT ( 'NONE',  ( 28.99687500061451573, -3.027376345333614438, 5.243569643749998122 ) ) ;
#16810 = VERTEX_POINT ( 'NONE', #23046 ) ;
#16811 = CARTESIAN_POINT ( 'NONE',  ( 23.61562500061451431, -6.054752690667223547, -1.112240025338166033E-15 ) ) ;
#16812 = CARTESIAN_POINT ( 'NONE',  ( 25.77187500061451075, 3.027376345333611329, 5.243569643749999010 ) ) ;
#16813 = CARTESIAN_POINT ( 'NONE',  ( 9.001249775931846008E-16, 18.11562500061459602, -25.09994784771203058 ) ) ;
#16814 = CARTESIAN_POINT ( 'NONE',  ( 11.84999999999999964, 4.330127018922192761, -2.499999999999997780 ) ) ;
#16815 = CARTESIAN_POINT ( 'NONE',  ( 9.965625000614517504, 3.027376345333611329, 5.243569643749999010 ) ) ;
#16816 = CARTESIAN_POINT ( 'NONE',  ( 6.037500000000001421, 5.773502691896255534, 3.535250795749688401E-16 ) ) ;
#16817 = CYLINDRICAL_SURFACE ( 'NONE', #45497, 5.999999999999998224 ) ;
#16818 = CARTESIAN_POINT ( 'NONE',  ( 27.32812500061451644, 6.421520780324663323E-16, -5.243569643749999010 ) ) ;
#16819 = FACE_OUTER_BOUND ( 'NONE', #11227, .T. ) ;
#16820 = CARTESIAN_POINT ( 'NONE',  ( 16.28437500061452070, 4.119189519843966529, 2.378215178124999607 ) ) ;
#16821 = CARTESIAN_POINT ( 'NONE',  ( 3.365625000614516082, -6.054752690667223547, -1.112240025338166033E-15 ) ) ;
#16822 = CARTESIAN_POINT ( 'NONE',  ( 19.88437500061451857, 4.541064518000418104, 2.621784821874999949 ) ) ;
#16823 = CARTESIAN_POINT ( 'NONE',  ( 2.121784821874999061, 14.30937500061451750, 26.32496088578401583 ) ) ;
#16824 = CARTESIAN_POINT ( 'NONE',  ( 21.49687500061451573, -3.027376345333610441, -5.243569643749999898 ) ) ;
#16825 = CARTESIAN_POINT ( 'NONE',  ( 29.03437500061451715, -4.541064518000419881, 2.621784821874995952 ) ) ;
#16826 = CARTESIAN_POINT ( 'NONE',  ( -3.000416591977282496E-16, 18.84687500061451360, 25.09994784771203058 ) ) ;
#16827 = CARTESIAN_POINT ( 'NONE',  ( 10.04062500061451502, -3.027376345333614438, 5.243569643749998122 ) ) ;
#16828 = CARTESIAN_POINT ( 'NONE',  ( 2.775000001229033675, -5.773502691896255534, -1.060575238724906372E-15 ) ) ;
#16829 = VECTOR ( 'NONE', #49151, 1000.000000000000000 ) ;
#16830 = CARTESIAN_POINT ( 'NONE',  ( 8.034375000614518925, 6.421520780324663323E-16, -5.243569643749999010 ) ) ;
#16831 = CARTESIAN_POINT ( 'NONE',  ( 1.626862140677534273E-15, 16.17500000122903359, -26.00000000000000355 ) ) ;
#16832 = CARTESIAN_POINT ( 'NONE',  ( 8.240625000614516082, -3.027376345333614438, 5.243569643749998122 ) ) ;
#16833 = CARTESIAN_POINT ( 'NONE',  ( 12.72187500061451537, 3.027376345333611329, 5.243569643749999010 ) ) ;
#16834 = CARTESIAN_POINT ( 'NONE',  ( 18.86250000122903359, 0.000000000000000000, 4.999999999999998224 ) ) ;
#16835 = CARTESIAN_POINT ( 'NONE',  ( 8.859375000614518214, -4.541064518000417216, -2.621784821875001281 ) ) ;
#16836 = CARTESIAN_POINT ( 'NONE',  ( 10.00312500061451715, 0.000000000000000000, 5.243569643749999010 ) ) ;
#16837 = CARTESIAN_POINT ( 'NONE',  ( 5.578125000614518214, -4.541064518000419881, 2.621784821874995952 ) ) ;
#16838 = CARTESIAN_POINT ( 'NONE',  ( 25.06875000122903074, 2.886751345948126879, 4.999999999999999112 ) ) ;
#16839 = CARTESIAN_POINT ( 'NONE',  ( 18.94687500061451502, 6.054752690667223547, 3.707466751127219781E-16 ) ) ;
#16840 = CARTESIAN_POINT ( 'NONE',  ( 17.39999999999999858, 0.000000000000000000, 4.999999999999998224 ) ) ;
#16841 = CARTESIAN_POINT ( 'NONE',  ( 27.21562500061451928, -6.054752690667223547, -1.112240025338166033E-15 ) ) ;
#16842 = CARTESIAN_POINT ( 'NONE',  ( 11.01562500061451821, -6.054752690667223547, -1.112240025338166033E-15 ) ) ;
#16843 = CARTESIAN_POINT ( 'NONE',  ( 28.58437500061451786, -4.541064518000419881, 2.621784821874995952 ) ) ;
#16844 = CARTESIAN_POINT ( 'NONE',  ( 2.121784821874999061, 11.60937500061451821, -33.67503911421598417 ) ) ;
#16845 = CARTESIAN_POINT ( 'NONE',  ( 13.57500000122903572, -5.773502691896255534, -1.060575238724906372E-15 ) ) ;
#16846 = CARTESIAN_POINT ( 'NONE',  ( 27.96562500061451928, 3.027376345333611329, 5.243569643749999010 ) ) ;
#16847 = CARTESIAN_POINT ( 'NONE',  ( 9.001249775931846008E-16, 14.96562500061451750, -25.09994784771203058 ) ) ;
#16848 = CARTESIAN_POINT ( 'NONE',  ( 14.73750000122903359, 4.330127018922191873, 2.499999999999999556 ) ) ;
#16849 = CARTESIAN_POINT ( 'NONE',  ( 12.33750000000000036, 5.773502691896255534, 3.535250795749688894E-16 ) ) ;
#16850 = CARTESIAN_POINT ( 'NONE',  ( -5.810221930991193690E-16, 13.58750000000000036, 26.00000000000000355 ) ) ;
#16851 = CARTESIAN_POINT ( 'NONE',  ( 23.05312500061451431, 0.000000000000000000, 5.243569643749999010 ) ) ;
#16852 = CARTESIAN_POINT ( 'NONE',  ( 6.609375000614519102, -4.541064518000417216, -2.621784821875001281 ) ) ;
#16853 = CARTESIAN_POINT ( 'NONE',  ( 8.925000001229033586, 2.886751345948126879, 4.999999999999999112 ) ) ;
#16854 = CARTESIAN_POINT ( 'NONE',  ( 16.57500000122903216, 2.886751345948126879, 4.999999999999999112 ) ) ;
#16855 = CARTESIAN_POINT ( 'NONE',  ( 11.99062500061451608, -3.027376345333610441, -5.243569643749999898 ) ) ;
#16856 = CARTESIAN_POINT ( 'NONE',  ( 17.46562500061451217, 3.027376345333613106, -5.243569643749998122 ) ) ;
#16857 = CARTESIAN_POINT ( 'NONE',  ( 24.71250000122903145, 0.000000000000000000, 4.999999999999998224 ) ) ;
#16858 = CARTESIAN_POINT ( 'NONE',  ( 28.27500000122903145, 2.886751345948126879, 4.999999999999999112 ) ) ;
#16859 = CARTESIAN_POINT ( 'NONE',  ( 23.62500000000000000, 4.330127018922191873, 2.499999999999999556 ) ) ;
#16860 = CARTESIAN_POINT ( 'NONE',  ( 24.60937500061451644, -4.541064518000417216, -2.621784821875001281 ) ) ;
#16861 = DIRECTION ( 'NONE',  ( -1.000000000000000000, -0.000000000000000000, -0.000000000000000000 ) ) ;
#16862 = CARTESIAN_POINT ( 'NONE',  ( 10.27500000122903323, 2.886751345948126879, 4.999999999999999112 ) ) ;
#16863 = CARTESIAN_POINT ( 'NONE',  ( 28.80937500061451573, 4.541064518000418104, -2.621784821874998173 ) ) ;
#16864 =( BOUNDED_CURVE ( )  B_SPLINE_CURVE ( 2, ( #15375, #10577, #33104, #3950, #16464, #60435, #20918 ),
 .UNSPECIFIED., .F., .F. ) 
 B_SPLINE_CURVE_WITH_KNOTS ( ( 3, 2, 2, 3 ),
 ( 0.7299999999999999822, 0.7333333333333332815, 0.7366666666666666918, 0.7399999999999999911 ),
 .UNSPECIFIED. ) 
 CURVE ( )  GEOMETRIC_REPRESENTATION_ITEM ( )  RATIONAL_B_SPLINE_CURVE ( ( 1.000000000000000000, 0.8660254037844387076, 1.000000000000000000, 0.8660254037844387076, 1.000000000000000000, 0.8660254037844387076, 1.000000000000000000 ) ) 
 REPRESENTATION_ITEM ( '' )  );
#16865 = CARTESIAN_POINT ( 'NONE',  ( 4.921875000614518214, 3.027376345333613106, -5.243569643749998122 ) ) ;
#16866 = CARTESIAN_POINT ( 'NONE',  ( 22.82812500061451644, 6.421520780324663323E-16, -5.243569643749999010 ) ) ;
#16867 = CARTESIAN_POINT ( 'NONE',  ( -3.756430356250000102, 15.67812499938548143, 30.00000000000000000 ) ) ;
#16868 = CARTESIAN_POINT ( 'NONE',  ( -2.000000000000001776, 15.44374999877096677, 33.46410161513775705 ) ) ;
#16869 = CARTESIAN_POINT ( 'NONE',  ( 10.47187500061451715, 3.027376345333611329, 5.243569643749999010 ) ) ;
#16870 = B_SPLINE_CURVE_WITH_KNOTS ( 'NONE', 3,
 ( #21370, #61992, #55370, #15827, #27296, #28028, #50556, #38371, #50198, #21735, #60524, #28377, #72723, #33548, #66450, #22106, #32469, #44296, #9930, #16555, #60896, #4408, #26937, #61623, #11026, #4763, #49830, #72354, #45015, #67551, #11392, #33912, #56455, #5845, #51276, #70348, #12477, #52003, #53354, #8655, #17281, #8291, #14190, #40197, #58881, #28735 ),
 .UNSPECIFIED., .F., .F.,
 ( 4, 2, 2, 2, 2, 2, 2, 2, 2, 2, 2, 2, 2, 2, 2, 2, 2, 2, 2, 2, 2, 2, 4 ),
 ( 0.01924954336552996484, 0.02045024950336954417, 0.02105060257228933210, 0.02165095564120912003, 0.02225130871012891143, 0.02285166177904869936, 0.02405236791688827175, 0.02525307405472784761, 0.02645378019256742000, 0.02705413326148721140, 0.02765448633040700280, 0.02825483939932679073, 0.02885519246824658213, 0.03005589860608615452, 0.03125660474392572691, 0.03245731088176529583, 0.03365801701960486475, 0.03485872315744444061, 0.03545907622636421813, 0.03605942929528400259, 0.03726013543312356457, 0.03786048850204334210, 0.03846084157096311962 ),
 .UNSPECIFIED. ) ;
#16871 = CARTESIAN_POINT ( 'NONE',  ( 4.898587196589411843E-16, 20.00000000000000000, -26.00000000000000000 ) ) ;
#16872 = CARTESIAN_POINT ( 'NONE',  ( 3.796875000614517326, -3.027376345333614438, 5.243569643749998122 ) ) ;
#16873 = CARTESIAN_POINT ( 'NONE',  ( 6.721875000614518925, 3.027376345333613106, -5.243569643749998122 ) ) ;
#16874 = CARTESIAN_POINT ( 'NONE',  ( 27.49687500061451217, 6.054752690667223547, 3.707466751127219781E-16 ) ) ;
#16875 = CARTESIAN_POINT ( 'NONE',  ( 4.243569643749999898, 10.09062500061459566, 32.45002607614398471 ) ) ;
#16876 = CARTESIAN_POINT ( 'NONE',  ( 18.82500000000000284, -4.330127018922194537, 2.499999999999995559 ) ) ;
#16877 = VERTEX_POINT ( 'NONE', #40414 ) ;
#16878 = CARTESIAN_POINT ( 'NONE',  ( 26.09999999999999787, -4.330127018922190985, -2.500000000000001332 ) ) ;
#16879 = CARTESIAN_POINT ( 'NONE',  ( 27.53437500061451360, 4.541064518000418104, 2.621784821874999949 ) ) ;
#16880 = EDGE_CURVE ( 'NONE', #9370, #26592, #34626, .T. ) ;
#16881 = VERTEX_POINT ( 'NONE', #68489 ) ;
#16882 = CARTESIAN_POINT ( 'NONE',  ( 14.31562500061451537, 3.027376345333613106, -5.243569643749998122 ) ) ;
#16883 = CARTESIAN_POINT ( 'NONE',  ( 7.190625000614518036, 6.054752690667223547, 3.707466751127219781E-16 ) ) ;
#16884 = CARTESIAN_POINT ( 'NONE',  ( 19.02187500061451431, -4.119189519843968306, 2.378215178124996054 ) ) ;
#16885 = CARTESIAN_POINT ( 'NONE',  ( 4.921875000614518214, 3.027376345333613106, -5.243569643749998122 ) ) ;
#16886 = CARTESIAN_POINT ( 'NONE',  ( 18.33750000122903501, 4.330127018922191873, 2.499999999999999556 ) ) ;
#16887 = CARTESIAN_POINT ( 'NONE',  ( 25.19999999999999929, -4.330127018922190985, -2.500000000000001332 ) ) ;
#16888 = CARTESIAN_POINT ( 'NONE',  ( 15.82499999999999929, 6.123233995736764310E-16, -4.999999999999998224 ) ) ;
#16889 = CARTESIAN_POINT ( 'NONE',  ( 8.221875000614518925, 3.027376345333611329, 5.243569643749999010 ) ) ;
#16890 = CARTESIAN_POINT ( 'NONE',  ( 11.14687500061451608, -3.027376345333610441, -5.243569643749999898 ) ) ;
#16891 = CARTESIAN_POINT ( 'NONE',  ( 22.13437500061451502, 4.541064518000418104, 2.621784821874999949 ) ) ;
#16892 = VERTEX_POINT ( 'NONE', #68136 ) ;
#16893 = CARTESIAN_POINT ( 'NONE',  ( 5.296875000614518214, -3.027376345333610441, -5.243569643749999898 ) ) ;
#16894 = CARTESIAN_POINT ( 'NONE',  ( 6.459375000614518747, 0.000000000000000000, 5.243569643749999010 ) ) ;
#16895 = CARTESIAN_POINT ( 'NONE',  ( 17.58749999999999858, -2.886751345948125991, -5.000000000000000000 ) ) ;
#16896 = CARTESIAN_POINT ( 'NONE',  ( 16.86562500061451786, -6.054752690667223547, -1.112240025338166033E-15 ) ) ;
#16897 = CARTESIAN_POINT ( 'NONE',  ( 1.999999999999997335, 18.27499999999999858, 33.46410161513775705 ) ) ;
#16898 = CARTESIAN_POINT ( 'NONE',  ( 22.27499999999999858, 4.330127018922191873, 2.499999999999999556 ) ) ;
#16899 = CARTESIAN_POINT ( 'NONE',  ( 21.94687500061451857, -2.746126346562642428, -4.756430356249999214 ) ) ;
#16900 = CARTESIAN_POINT ( 'NONE',  ( 10.30312500061451431, 4.541064518000418104, -2.621784821874998173 ) ) ;
#16901 = CARTESIAN_POINT ( 'NONE',  ( 27.53437500061451360, 4.541064518000418104, 2.621784821874999949 ) ) ;
#16902 = CARTESIAN_POINT ( 'NONE',  ( 45.00000000000000000, 0.000000000000000000, 0.000000000000000000 ) ) ;
#16903 = CARTESIAN_POINT ( 'NONE',  ( 28.39687500061452141, 6.054752690667223547, 3.707466751127219781E-16 ) ) ;
#16904 = CARTESIAN_POINT ( 'NONE',  ( 11.10000000000000142, 0.000000000000000000, 4.999999999999998224 ) ) ;
#16905 = CARTESIAN_POINT ( 'NONE',  ( 4.000000000000000000, 16.70000000122903572, 32.30940107675849049 ) ) ;
#16906 = CARTESIAN_POINT ( 'NONE',  ( 10.27500000122903323, 2.886751345948126879, 4.999999999999999112 ) ) ;
#16907 = CARTESIAN_POINT ( 'NONE',  ( 20.14687500061451786, -3.027376345333610441, -5.243569643749999898 ) ) ;
#16908 = CARTESIAN_POINT ( 'NONE',  ( 15.08437500061451786, -4.541064518000419881, 2.621784821874995952 ) ) ;
#16909 = CARTESIAN_POINT ( 'NONE',  ( -2.928932188134524939, -4.999999999999996447, -2.928932188134524939 ) ) ;
#16910 = ORIENTED_EDGE ( 'NONE', *, *, #380, .F. ) ;
#16911 = CARTESIAN_POINT ( 'NONE',  ( 13.75312500061451715, -4.541064518000417216, -2.621784821875001281 ) ) ;
#16912 = CARTESIAN_POINT ( 'NONE',  ( 27.45000000122903572, -2.886751345948129988, 4.999999999999997335 ) ) ;
#16913 = CARTESIAN_POINT ( 'NONE',  ( 15.53437500061451715, -4.541064518000419881, 2.621784821874995952 ) ) ;
#16914 = CARTESIAN_POINT ( 'NONE',  ( 3.478125000614517237, 6.421520780324663323E-16, -5.243569643749999010 ) ) ;
#16915 = CARTESIAN_POINT ( 'NONE',  ( 15.89062500061451289, -3.027376345333614438, 5.243569643749998122 ) ) ;
#16916 = CARTESIAN_POINT ( 'NONE',  ( 3.999999999999998668, 20.05624999877096570, 32.30940107675850470 ) ) ;
#16917 = CARTESIAN_POINT ( 'NONE',  ( 25.62187500061451573, 3.027376345333613106, -5.243569643749998122 ) ) ;
#16918 = CARTESIAN_POINT ( 'NONE',  ( -4.243569643749997233, 9.940625000614515372, 32.45002607614398471 ) ) ;
#16919 = CARTESIAN_POINT ( 'NONE',  ( 15.75937500061451857, 4.541064518000418104, -2.621784821874998173 ) ) ;
#16920 =( BOUNDED_CURVE ( )  B_SPLINE_CURVE ( 2, ( #9338, #2698, #42222, #25213, #3063, #47760, #19668, #58827, #30408 ),
 .UNSPECIFIED., .F., .F. ) 
 B_SPLINE_CURVE_WITH_KNOTS ( ( 3, 2, 2, 2, 3 ),
 ( 0.4456521739130435145, 0.4492753623188405765, 0.4565217391304347561, 0.4637681159420289911, 0.4673913043478261087 ),
 .UNSPECIFIED. ) 
 CURVE ( )  GEOMETRIC_REPRESENTATION_ITEM ( )  RATIONAL_B_SPLINE_CURVE ( ( 0.9330127018922194093, 0.9330127018922198534, 1.000000000000000000, 0.8660254037844387076, 1.000000000000000000, 0.8660254037844387076, 1.000000000000000000, 0.9330127018922188542, 0.9330127018922194093 ) ) 
 REPRESENTATION_ITEM ( '' )  );
#16921 = CARTESIAN_POINT ( 'NONE',  ( 14.51250000122903394, -4.330127018922190985, -2.500000000000001332 ) ) ;
#16922 = DIRECTION ( 'NONE',  ( -1.000000000000000000, -0.000000000000000000, -0.000000000000000000 ) ) ;
#16923 = CARTESIAN_POINT ( 'NONE',  ( 0.000000000000000000, 20.00000000000000000, 30.00000000000000000 ) ) ;
#16924 = CARTESIAN_POINT ( 'NONE',  ( 17.14687500061451786, 6.054752690667223547, 3.707466751127219781E-16 ) ) ;
#16925 = CARTESIAN_POINT ( 'NONE',  ( 19.83750000122903145, -4.330127018922194537, 2.499999999999995559 ) ) ;
#16926 =( BOUNDED_CURVE ( )  B_SPLINE_CURVE ( 2, ( #44165, #50065, #49338, #21242, #72595, #27531, #43794 ),
 .UNSPECIFIED., .F., .F. ) 
 B_SPLINE_CURVE_WITH_KNOTS ( ( 3, 2, 2, 3 ),
 ( 0.03333333333333339532, 0.03611111111111116323, 0.03888888888888894502, 0.04166666666666671293 ),
 .UNSPECIFIED. ) 
 CURVE ( )  GEOMETRIC_REPRESENTATION_ITEM ( )  RATIONAL_B_SPLINE_CURVE ( ( 0.9999999999999968914, 0.8660254037844417052, 1.000000000000000000, 0.8660254037844387076, 1.000000000000000000, 0.8660254037844363761, 1.000000000000002442 ) ) 
 REPRESENTATION_ITEM ( '' )  );
#16927 = CARTESIAN_POINT ( 'NONE',  ( 13.65937500061451715, 0.000000000000000000, 5.243569643749999010 ) ) ;
#16928 = CARTESIAN_POINT ( 'NONE',  ( 2.121784821875001281, 12.80937500061451928, 33.67503911421598417 ) ) ;
#16929 = CARTESIAN_POINT ( 'NONE',  ( 22.20000000122903216, -2.886751345948125991, -5.000000000000000000 ) ) ;
#16930 = CARTESIAN_POINT ( 'NONE',  ( 18.51562500061451289, 3.027376345333611329, 5.243569643749999010 ) ) ;
#16931 = ORIENTED_EDGE ( 'NONE', *, *, #67466, .F. ) ;
#16932 = ORIENTED_EDGE ( 'NONE', *, *, #21809, .T. ) ;
#16933 = CARTESIAN_POINT ( 'NONE',  ( 21.52499999999999858, -4.330127018922194537, 2.499999999999995559 ) ) ;
#16934 = DIRECTION ( 'NONE',  ( -0.000000000000000000, -1.000000000000000000, -0.000000000000000000 ) ) ;
#16935 = CARTESIAN_POINT ( 'NONE',  ( 21.62812500061451360, 4.541064518000418104, 2.621784821874999949 ) ) ;
#16936 = CARTESIAN_POINT ( 'NONE',  ( 3.963750086740946088, 3.047826611959361554, 29.44540702803496401 ) ) ;
#16937 = CARTESIAN_POINT ( 'NONE',  ( 13.98750000122903359, -4.330127018922194537, 2.499999999999995559 ) ) ;
#16938 = CARTESIAN_POINT ( 'NONE',  ( 21.10312500061451502, 4.541064518000418104, -2.621784821874998173 ) ) ;
#16939 = CARTESIAN_POINT ( 'NONE',  ( 24.36562500061451786, 3.027376345333611329, 5.243569643749999010 ) ) ;
#16940 = CARTESIAN_POINT ( 'NONE',  ( 4.978125000614518569, 4.541064518000418104, 2.621784821874999949 ) ) ;
#16941 = EDGE_LOOP ( 'NONE', ( #36634, #63049, #21750, #41465 ) ) ;
#16942 = ADVANCED_FACE ( 'NONE', ( #1987 ), #11972, .F. ) ;
#16943 =( BOUNDED_CURVE ( )  B_SPLINE_CURVE ( 3, ( #31871, #20404, #71397, #66583 ),
 .UNSPECIFIED., .F., .F. ) 
 B_SPLINE_CURVE_WITH_KNOTS ( ( 4, 4 ),
 ( 3.903471329280879143, 3.934893574429339846 ),
 .UNSPECIFIED. ) 
 CURVE ( )  GEOMETRIC_REPRESENTATION_ITEM ( )  RATIONAL_B_SPLINE_CURVE ( ( 1.000000000000000000, 0.9999177219016296414, 0.9999177219016296414, 1.000000000000000000 ) ) 
 REPRESENTATION_ITEM ( '' )  );
#16944 = CARTESIAN_POINT ( 'NONE',  ( -3.999999999999999112, 10.21250000122903501, -30.00000000000000000 ) ) ;
#16945 = EDGE_CURVE ( 'NONE', #70308, #37144, #29328, .T. ) ;
#16946 = CARTESIAN_POINT ( 'NONE',  ( 10.88437500061451679, 4.119189519843966529, 2.378215178124999607 ) ) ;
#16947 = DIRECTION ( 'NONE',  ( -1.000000000000000000, -0.000000000000000000, -0.000000000000000000 ) ) ;
#16948 = CARTESIAN_POINT ( 'NONE',  ( -1.999999999999997113, 10.28750000122903430, -26.53589838486224295 ) ) ;
#16949 = CARTESIAN_POINT ( 'NONE',  ( -4.243569643749999898, 17.57187500061451502, -32.45002607614398471 ) ) ;
#16950 = CARTESIAN_POINT ( 'NONE',  ( 6.712500001229034119, 0.000000000000000000, 4.999999999999998224 ) ) ;
#16951 = CARTESIAN_POINT ( 'NONE',  ( 7.237500000000000711, -2.886751345948125991, -5.000000000000000000 ) ) ;
#16952 = EDGE_CURVE ( 'NONE', #42898, #69508, #44591, .T. ) ;
#16953 = CARTESIAN_POINT ( 'NONE',  ( 3.825000001229032609, 2.886751345948129099, -4.999999999999998224 ) ) ;
#16954 = CARTESIAN_POINT ( 'NONE',  ( 11.40937500061451892, 0.000000000000000000, 5.243569643749999010 ) ) ;
#16955 = CARTESIAN_POINT ( 'NONE',  ( 14.30625000122903145, 0.000000000000000000, 4.999999999999998224 ) ) ;
#16956 = CARTESIAN_POINT ( 'NONE',  ( 4.246875000614519280, -3.027376345333614438, 5.243569643749998122 ) ) ;
#16957 = CARTESIAN_POINT ( 'NONE',  ( 3.881554241669678884, -3.151751365348489653, -4.190642664303462439 ) ) ;
#16958 = EDGE_CURVE ( 'NONE', #66380, #15804, #51502, .T. ) ;
#16959 = CARTESIAN_POINT ( 'NONE',  ( 10.65937500061451715, -4.541064518000417216, -2.621784821875001281 ) ) ;
#16960 = CARTESIAN_POINT ( 'NONE',  ( 3.999999999999999112, 14.03750000122903430, -30.00000000000000000 ) ) ;
#16961 = CARTESIAN_POINT ( 'NONE',  ( 1.999999999999998668, 14.45000000000000107, 26.53589838486224650 ) ) ;
#16962 = CARTESIAN_POINT ( 'NONE',  ( 2.121784821874999061, 16.95312500061459815, 26.32496088578401583 ) ) ;
#16963 = CARTESIAN_POINT ( 'NONE',  ( 20.44687500061451857, -3.027376345333614438, 5.243569643749998122 ) ) ;
#16964 = CARTESIAN_POINT ( 'NONE',  ( 3.065625000614517592, 3.027376345333613106, -5.243569643749998122 ) ) ;
#16965 = CARTESIAN_POINT ( 'NONE',  ( 17.48437500061451644, 5.492252693125287522, 3.363034840372157021E-16 ) ) ;
#16966 = CARTESIAN_POINT ( 'NONE',  ( 25.79062500061451502, -3.027376345333614438, 5.243569643749998122 ) ) ;
#16967 = CARTESIAN_POINT ( 'NONE',  ( 16.67812500061451786, 4.541064518000418104, 2.621784821874999949 ) ) ;
#16968 = CARTESIAN_POINT ( 'NONE',  ( 13.51875000122903536, -5.773502691896255534, -1.060575238724906372E-15 ) ) ;
#16969 = CARTESIAN_POINT ( 'NONE',  ( 12.19687500061451679, 6.054752690667223547, 3.707466751127219781E-16 ) ) ;
#16970 = CARTESIAN_POINT ( 'NONE',  ( 29.47499999999999787, 4.330127018922191873, 2.499999999999999556 ) ) ;
#16971 = CARTESIAN_POINT ( 'NONE',  ( 25.83750000122903501, 6.123233995736764310E-16, -4.999999999999998224 ) ) ;
#16972 = CARTESIAN_POINT ( 'NONE',  ( 4.396875000614516971, -3.027376345333610441, -5.243569643749999898 ) ) ;
#16973 = CARTESIAN_POINT ( 'NONE',  ( 14.37187500061451928, 3.027376345333613106, -5.243569643749998122 ) ) ;
#16974 = CARTESIAN_POINT ( 'NONE',  ( 21.07499999999999929, -4.330127018922194537, 2.499999999999995559 ) ) ;
#16975 = CARTESIAN_POINT ( 'NONE',  ( 3.242103837493086330E-14, 11.33750000000000213, 26.00000000000000711 ) ) ;
#16976 = CARTESIAN_POINT ( 'NONE',  ( 29.80312500061451431, 0.000000000000000000, 4.756430356249998326 ) ) ;
#16977 = CARTESIAN_POINT ( 'NONE',  ( 23.52187500061451786, 3.027376345333611329, 5.243569643749999010 ) ) ;
#16978 = CARTESIAN_POINT ( 'NONE',  ( 14.44687500061451679, 6.054752690667223547, 3.707466751127219781E-16 ) ) ;
#16979 = CARTESIAN_POINT ( 'NONE',  ( -1.878215178125001827, 17.10312499938548214, 33.25316411605952283 ) ) ;
#16980 = CARTESIAN_POINT ( 'NONE',  ( 27.29999999999999716, 0.000000000000000000, 4.999999999999998224 ) ) ;
#16981 = DIRECTION ( 'NONE',  ( -0.000000000000000000, -1.000000000000000000, -0.000000000000000000 ) ) ;
#16982 = CARTESIAN_POINT ( 'NONE',  ( 29.25937500061451502, 4.119189519843966529, -2.378215178124998275 ) ) ;
#16983 = CARTESIAN_POINT ( 'NONE',  ( 16.75312500061451715, 0.000000000000000000, 5.243569643749999010 ) ) ;
#16984 = CARTESIAN_POINT ( 'NONE',  ( 7.537500000000002309, -2.886751345948129988, 4.999999999999997335 ) ) ;
#16985 = CARTESIAN_POINT ( 'NONE',  ( 26.68125000122903145, 6.123233995736764310E-16, -4.999999999999998224 ) ) ;
#16986 = CARTESIAN_POINT ( 'NONE',  ( 15.93750000000000000, 5.773502691896255534, 3.535250795749688894E-16 ) ) ;
#16987 = CARTESIAN_POINT ( 'NONE',  ( -4.243569643749999898, 12.11562500061451608, 27.54997392385601529 ) ) ;
#16988 = CARTESIAN_POINT ( 'NONE',  ( 45.00000000000000000, 0.000000000000000000, 4.999999999999998224 ) ) ;
#16989 = CARTESIAN_POINT ( 'NONE',  ( 20.21250000122903145, 0.000000000000000000, 4.999999999999998224 ) ) ;
#16990 = CYLINDRICAL_SURFACE ( 'NONE', #28859, 4.999999999999998224 ) ;
#16991 = CARTESIAN_POINT ( 'NONE',  ( 28.02187500061451431, 3.027376345333611329, 5.243569643749999010 ) ) ;
#16992 = ORIENTED_EDGE ( 'NONE', *, *, #3406, .F. ) ;
#16993 = CARTESIAN_POINT ( 'NONE',  ( 21.85312500061451502, -4.541064518000417216, -2.621784821875001281 ) ) ;
#16994 = CARTESIAN_POINT ( 'NONE',  ( 22.35937500061451644, -4.541064518000417216, -2.621784821875001281 ) ) ;
#16995 = B_SPLINE_CURVE_WITH_KNOTS ( 'NONE', 3,
 ( #14611, #60040, #9451, #31981, #47509, #36424, #26441, #64492, #30520, #69681 ),
 .UNSPECIFIED., .F., .F.,
 ( 4, 3, 3, 4 ),
 ( 1.664927911480095392E-16, 2.812505234851141628E-05, 5.777440207181503025E-05, 8.742424744633160846E-05 ),
 .UNSPECIFIED. ) ;
#16996 = CARTESIAN_POINT ( 'NONE',  ( 6.075000000000000178, 4.330127018922191873, 2.499999999999999556 ) ) ;
#16997 = CARTESIAN_POINT ( 'NONE',  ( 9.890625000614516438, 6.054752690667223547, 3.707466751127219781E-16 ) ) ;
#16998 = CARTESIAN_POINT ( 'NONE',  ( 23.65312500061451573, -4.541064518000417216, -2.621784821875001281 ) ) ;
#16999 = CARTESIAN_POINT ( 'NONE',  ( 13.58437500061451786, 4.541064518000418104, 2.621784821874999949 ) ) ;
#17000 = CARTESIAN_POINT ( 'NONE',  ( 17.63437500061451502, 4.541064518000418104, 2.621784821874999949 ) ) ;
#17001 = CARTESIAN_POINT ( 'NONE',  ( 19.42499999999999716, 6.123233995736764310E-16, -4.999999999999998224 ) ) ;
#17002 = CARTESIAN_POINT ( 'NONE',  ( 4.243569643749999898, 18.64062500061451644, 32.45002607614398471 ) ) ;
#17003 = CARTESIAN_POINT ( 'NONE',  ( 20.47500000122903074, 2.886751345948129099, -4.999999999999998224 ) ) ;
#17004 = CARTESIAN_POINT ( 'NONE',  ( 15.27187500061451786, 2.746126346562645981, -4.756430356249997438 ) ) ;
#17005 = CARTESIAN_POINT ( 'NONE',  ( 13.04062500061451502, 6.054752690667223547, 3.707466751127219781E-16 ) ) ;
#17006 = CARTESIAN_POINT ( 'NONE',  ( 5.784375000614517148, 6.421520780324663323E-16, -5.243569643749999010 ) ) ;
#17007 = CARTESIAN_POINT ( 'NONE',  ( 3.684375000614518836, 4.541064518000418104, 2.621784821874999949 ) ) ;
#17008 = ORIENTED_EDGE ( 'NONE', *, *, #19932, .F. ) ;
#17009 = CARTESIAN_POINT ( 'NONE',  ( 28.65937500061451715, -4.541064518000417216, -2.621784821875001281 ) ) ;
#17010 = CARTESIAN_POINT ( 'NONE',  ( 16.41562500061451857, -6.054752690667223547, -1.112240025338166033E-15 ) ) ;
#17011 = CARTESIAN_POINT ( 'NONE',  ( 27.11250000122903359, -4.330127018922190985, -2.500000000000001332 ) ) ;
#17012 = CARTESIAN_POINT ( 'NONE',  ( 28.90312500061451217, 0.000000000000000000, 5.243569643749999010 ) ) ;
#17013 = CARTESIAN_POINT ( 'NONE',  ( 21.42187500061451644, -6.054752690667223547, -1.112240025338166033E-15 ) ) ;
#17014 = CARTESIAN_POINT ( 'NONE',  ( 16.94062500061451715, -3.027376345333610441, -5.243569643749999898 ) ) ;
#17015 = CARTESIAN_POINT ( 'NONE',  ( 4.000000000000000000, 10.28750000000000142, 32.30940107675849049 ) ) ;
#17016 = CARTESIAN_POINT ( 'NONE',  ( 24.59062500061451573, -3.027376345333610441, -5.243569643749999898 ) ) ;
#17017 = CARTESIAN_POINT ( 'NONE',  ( 4.537500001229034297, -4.330127018922194537, 2.499999999999995559 ) ) ;
#17018 = VERTEX_POINT ( 'NONE', #1260 ) ;
#17019 = CARTESIAN_POINT ( 'NONE',  ( 26.66250000000000142, 2.886751345948129099, -4.999999999999998224 ) ) ;
#17020 = CARTESIAN_POINT ( 'NONE',  ( -1.999999999999997113, 11.97500000000000142, -26.53589838486224295 ) ) ;
#17021 = CARTESIAN_POINT ( 'NONE',  ( -1.878215178125001827, 16.65312499938548285, 33.25316411605952283 ) ) ;
#17022 = CARTESIAN_POINT ( 'NONE',  ( 5.034375000614519813, 4.541064518000418104, 2.621784821874999949 ) ) ;
#17023 = CARTESIAN_POINT ( 'NONE',  ( 10.45312500061451644, 0.000000000000000000, 5.243569643749999010 ) ) ;
#17024 = CARTESIAN_POINT ( 'NONE',  ( 7.321875000614516793, 3.027376345333611329, 5.243569643749999010 ) ) ;
#17025 = CARTESIAN_POINT ( 'NONE',  ( 25.42500000122903359, 2.886751345948129099, -4.999999999999998224 ) ) ;
#17026 = CARTESIAN_POINT ( 'NONE',  ( 12.94687500061451857, -3.027376345333610441, -5.243569643749999898 ) ) ;
#17027 = CARTESIAN_POINT ( 'NONE',  ( 3.684375000614518836, 4.541064518000418104, 2.621784821874999949 ) ) ;
#17028 = CARTESIAN_POINT ( 'NONE',  ( 26.66250000000000142, 2.886751345948129099, -4.999999999999998224 ) ) ;
#17029 = CARTESIAN_POINT ( 'NONE',  ( 14.81250000122903288, 0.000000000000000000, 4.999999999999998224 ) ) ;
#17030 = CARTESIAN_POINT ( 'NONE',  ( 13.49062500061451608, 6.054752690667223547, 3.707466751127219781E-16 ) ) ;
#17031 = ORIENTED_EDGE ( 'NONE', *, *, #65041, .T. ) ;
#17032 = EDGE_CURVE ( 'NONE', #61955, #20756, #52114, .T. ) ;
#17033 = CARTESIAN_POINT ( 'NONE',  ( 10.15312500061451750, -4.541064518000417216, -2.621784821875001281 ) ) ;
#17034 = VECTOR ( 'NONE', #26597, 1000.000000000000000 ) ;
#17035 = CARTESIAN_POINT ( 'NONE',  ( 4.978125000614518569, 4.541064518000418104, 2.621784821874999949 ) ) ;
#17036 = CARTESIAN_POINT ( 'NONE',  ( 17.67187500061451644, 2.746126346562643317, 4.756430356249998326 ) ) ;
#17037 = EDGE_CURVE ( 'NONE', #36109, #6463, #9164, .T. ) ;
#17038 = CYLINDRICAL_SURFACE ( 'NONE', #45630, 4.999999999999998224 ) ;
#17039 = CARTESIAN_POINT ( 'NONE',  ( 15.33750000000000036, -2.886751345948125991, -5.000000000000000000 ) ) ;
#17040 = EDGE_CURVE ( 'NONE', #65810, #41603, #3141, .T. ) ;
#17041 = CARTESIAN_POINT ( 'NONE',  ( 16.69687500061451502, 6.054752690667223547, 3.707466751127219781E-16 ) ) ;
#17042 = CARTESIAN_POINT ( 'NONE',  ( 11.40000000122903501, -2.886751345948125991, -5.000000000000000000 ) ) ;
#17043 = CARTESIAN_POINT ( 'NONE',  ( 19.43437500061451928, 4.541064518000418104, 2.621784821874999949 ) ) ;
#17044 = CARTESIAN_POINT ( 'NONE',  ( 20.13749999999999929, -2.886751345948129988, 4.999999999999997335 ) ) ;
#17045 = CARTESIAN_POINT ( 'NONE',  ( 21.53437500061451715, 6.421520780324663323E-16, -5.243569643749999010 ) ) ;
#17046 = CARTESIAN_POINT ( 'NONE',  ( -4.243569643749997233, 13.54062500061451679, -27.54997392385601174 ) ) ;
#17047 = VECTOR ( 'NONE', #24318, 1000.000000000000000 ) ;
#17048 = CARTESIAN_POINT ( 'NONE',  ( 7.387500000000001954, 5.773502691896255534, 3.535250795749688401E-16 ) ) ;
#17049 = CARTESIAN_POINT ( 'NONE',  ( 25.80937500061451573, -5.492252693125287522, -1.008910452111647106E-15 ) ) ;
#17050 = CARTESIAN_POINT ( 'NONE',  ( 4.126442089077904107, 2.823557275049659143, 4.418432631982811110 ) ) ;
#17051 = CARTESIAN_POINT ( 'NONE',  ( 26.61562500061451786, 3.027376345333611329, 5.243569643749999010 ) ) ;
#17052 = FACE_OUTER_BOUND ( 'NONE', #573, .T. ) ;
#17053 = CARTESIAN_POINT ( 'NONE',  ( 29.70937500061451431, 4.541064518000418104, -2.621784821874998173 ) ) ;
#17054 = CARTESIAN_POINT ( 'NONE',  ( 24.86250000000000071, 2.886751345948129099, -4.999999999999998224 ) ) ;
#17055 = CARTESIAN_POINT ( 'NONE',  ( 8.315625000614515372, -6.054752690667223547, -1.112240025338166033E-15 ) ) ;
#17056 = CARTESIAN_POINT ( 'NONE',  ( 27.98437500061451644, -2.746126346562646425, 4.756430356249996549 ) ) ;
#17057 = CARTESIAN_POINT ( 'NONE',  ( 19.28437500061451360, 6.421520780324663323E-16, -5.243569643749999010 ) ) ;
#17058 = CARTESIAN_POINT ( 'NONE',  ( 10.92187500061451644, -4.119189519843968306, 2.378215178124996054 ) ) ;
#17059 = CARTESIAN_POINT ( 'NONE',  ( 5.503125000614516260, 0.000000000000000000, 5.243569643749999010 ) ) ;
#17060 = CARTESIAN_POINT ( 'NONE',  ( 9.984375000614518214, 4.541064518000418104, 2.621784821874999949 ) ) ;
#17061 = ORIENTED_EDGE ( 'NONE', *, *, #17352, .F. ) ;
#17062 = CARTESIAN_POINT ( 'NONE',  ( 20.52187500061451786, -6.054752690667223547, -1.112240025338166033E-15 ) ) ;
#17063 = CARTESIAN_POINT ( 'NONE',  ( 16.53750000000000142, -2.886751345948130876, 4.999999999999996447 ) ) ;
#17064 = CARTESIAN_POINT ( 'NONE',  ( 20.99999999999999645, 0.000000000000000000, 4.999999999999998224 ) ) ;
#17066 = ADVANCED_FACE ( 'NONE', ( #64018 ), #26667, .T. ) ;
#17065 = CARTESIAN_POINT ( 'NONE',  ( 5.175000000000002487, 4.330127018922191873, 2.499999999999999556 ) ) ;
#17067 = CARTESIAN_POINT ( 'NONE',  ( 15.18750000122903465, 4.330127018922191873, 2.499999999999999556 ) ) ;
#17068 = CARTESIAN_POINT ( 'NONE',  ( 17.94375000122903074, -2.886751345948130876, 4.999999999999996447 ) ) ;
#17069 = ORIENTED_EDGE ( 'NONE', *, *, #5701, .T. ) ;
#17070 = CARTESIAN_POINT ( 'NONE',  ( 11.92500000000000071, 4.330127018922191873, 2.499999999999999556 ) ) ;
#17071 = CARTESIAN_POINT ( 'NONE',  ( 24.36562500061451786, 3.027376345333611329, 5.243569643749999010 ) ) ;
#17072 = CARTESIAN_POINT ( 'NONE',  ( 16.08749999999999503, -2.886751345948129988, 4.999999999999997335 ) ) ;
#17073 = CARTESIAN_POINT ( 'NONE',  ( 10.46250000122903323, -4.330127018922190985, -2.500000000000001332 ) ) ;
#17074 = CARTESIAN_POINT ( 'NONE',  ( 9.140625000614518214, -3.027376345333614438, 5.243569643749998122 ) ) ;
#17075 = CARTESIAN_POINT ( 'NONE',  ( 8.925000000000002487, -4.330127018922194537, 2.499999999999995559 ) ) ;
#17076 = DIRECTION ( 'NONE',  ( -1.000000000000000000, -0.000000000000000000, -0.000000000000000000 ) ) ;
#17077 = CARTESIAN_POINT ( 'NONE',  ( -4.243569643749999898, 13.97187500061451715, -32.45002607614398471 ) ) ;
#17078 = CARTESIAN_POINT ( 'NONE',  ( 26.92500000122903359, 2.886751345948126879, 4.999999999999999112 ) ) ;
#17079 = CARTESIAN_POINT ( 'NONE',  ( 1.878215178125000495, 14.06562499938548250, 26.74683588394047007 ) ) ;
#17080 = CARTESIAN_POINT ( 'NONE',  ( 7.087499999999999467, -2.886751345948129988, 4.999999999999997335 ) ) ;
#17081 = FACE_OUTER_BOUND ( 'NONE', #20364, .T. ) ;
#17082 = ORIENTED_EDGE ( 'NONE', *, *, #16407, .T. ) ;
#17083 = CARTESIAN_POINT ( 'NONE',  ( 23.42812500061451786, 4.541064518000418104, 2.621784821874999949 ) ) ;
#17084 = CARTESIAN_POINT ( 'NONE',  ( 14.92500000122903181, -5.773502691896255534, -1.060575238724906372E-15 ) ) ;
#17085 = CARTESIAN_POINT ( 'NONE',  ( 28.82812500061451644, 4.541064518000418104, 2.621784821874999949 ) ) ;
#17086 = CARTESIAN_POINT ( 'NONE',  ( 28.92187500061451644, 3.027376345333611329, 5.243569643749999010 ) ) ;
#17087 = CARTESIAN_POINT ( 'NONE',  ( 18.34687500061451715, -3.027376345333610441, -5.243569643749999898 ) ) ;
#17088 = CARTESIAN_POINT ( 'NONE',  ( 16.79062500061451857, -3.027376345333614438, 5.243569643749998122 ) ) ;
#17089 = CARTESIAN_POINT ( 'NONE',  ( -4.243569643749998122, 11.29062500061459495, -27.54997392385601174 ) ) ;
#17090 = CARTESIAN_POINT ( 'NONE',  ( 6.553125000614518747, -4.541064518000417216, -2.621784821875001281 ) ) ;
#17091 = AXIS2_PLACEMENT_3D ( 'NONE', #40349, #45541, #29266 ) ;
#17092 = CARTESIAN_POINT ( 'NONE',  ( 27.86250000122903359, 0.000000000000000000, 4.999999999999998224 ) ) ;
#17093 = CARTESIAN_POINT ( 'NONE',  ( 20.89687500061451786, -2.746126346562646425, 4.756430356249996549 ) ) ;
#17094 = CARTESIAN_POINT ( 'NONE',  ( 19.04062500061451146, -3.027376345333614438, 5.243569643749998122 ) ) ;
#17095 = CARTESIAN_POINT ( 'NONE',  ( -5.810221930991193690E-16, 10.10000000122903430, 26.00000000000000355 ) ) ;
#17096 = CARTESIAN_POINT ( 'NONE',  ( 2.655984681222220721E-16, 17.70312499938548356, 25.66244784525396483 ) ) ;
#17097 = CARTESIAN_POINT ( 'NONE',  ( 13.24687500061451750, -3.027376345333614438, 5.243569643749998122 ) ) ;
#17098 = CARTESIAN_POINT ( 'NONE',  ( 11.03437500061451715, -4.541064518000419881, 2.621784821874995952 ) ) ;
#17099 = CARTESIAN_POINT ( 'NONE',  ( 19.62187500061451573, -6.054752690667223547, -1.112240025338166033E-15 ) ) ;
#17100 = VERTEX_POINT ( 'NONE', #16251 ) ;
#17101 = CARTESIAN_POINT ( 'NONE',  ( 19.91250000000000142, 2.886751345948129099, -4.999999999999997335 ) ) ;
#17102 = CARTESIAN_POINT ( 'NONE',  ( 27.21562500061451928, -6.054752690667223547, -1.112240025338166033E-15 ) ) ;
#17103 = CARTESIAN_POINT ( 'NONE',  ( 25.19062500061451715, 6.054752690667223547, 3.707466751127219781E-16 ) ) ;
#17104 = DIRECTION ( 'NONE',  ( -1.000000000000000000, -0.000000000000000000, -0.000000000000000000 ) ) ;
#17105 = CARTESIAN_POINT ( 'NONE',  ( -3.999999999999999112, 17.30000000000000071, 30.00000000000000000 ) ) ;
#17106 = CARTESIAN_POINT ( 'NONE',  ( 4.959375000614516971, 4.541064518000418104, -2.621784821874998173 ) ) ;
#17107 = CARTESIAN_POINT ( 'NONE',  ( 11.85000000122903430, -2.886751345948125991, -5.000000000000000000 ) ) ;
#17108 = VECTOR ( 'NONE', #1308, 1000.000000000000000 ) ;
#17109 = CARTESIAN_POINT ( 'NONE',  ( 6.300000001229033586, -2.886751345948129988, 4.999999999999997335 ) ) ;
#17110 = PLANE ( 'NONE',  #38671 ) ;
#17111 = CARTESIAN_POINT ( 'NONE',  ( 28.42500000122904069, -5.773502691896255534, -1.060575238724906372E-15 ) ) ;
#17112 = CARTESIAN_POINT ( 'NONE',  ( 4.000000000000000000, 18.78124999877096357, 27.69059892324149530 ) ) ;
#17113 = CARTESIAN_POINT ( 'NONE',  ( 16.36875000122903145, 2.886751345948129099, -4.999999999999998224 ) ) ;
#17114 = CARTESIAN_POINT ( 'NONE',  ( 11.25937500061451679, 4.541064518000418104, -2.621784821874998173 ) ) ;
#17115 = CARTESIAN_POINT ( 'NONE',  ( 30.00000000000000000, 6.123233995736764310E-16, -4.999999999999998224 ) ) ;
#17116 = CARTESIAN_POINT ( 'NONE',  ( 17.80312500061451786, -4.541064518000417216, -2.621784821875001281 ) ) ;
#17117 = CARTESIAN_POINT ( 'NONE',  ( 13.69687500061451679, -3.027376345333614438, 5.243569643749998122 ) ) ;
#17118 = CARTESIAN_POINT ( 'NONE',  ( 4.865625000614517859, 3.027376345333613106, -5.243569643749998122 ) ) ;
#17119 = CARTESIAN_POINT ( 'NONE',  ( 22.39687500061451075, -3.027376345333610441, -5.243569643749999898 ) ) ;
#17120 = CARTESIAN_POINT ( 'NONE',  ( 9.909375000614517148, 4.541064518000418104, -2.621784821874998173 ) ) ;
#17121 = CARTESIAN_POINT ( 'NONE',  ( 4.003125000614518925, 4.541064518000418104, -2.621784821874998173 ) ) ;
#17122 = CARTESIAN_POINT ( 'NONE',  ( 0.000000000000000000, 27.50000000000000000, 30.00000000000000000 ) ) ;
#17123 = CARTESIAN_POINT ( 'NONE',  ( 6.000000001229033764, -2.886751345948125991, -5.000000000000000000 ) ) ;
#17124 = CARTESIAN_POINT ( 'NONE',  ( 20.76562500061451644, 3.027376345333611329, 5.243569643749999010 ) ) ;
#17125 = CARTESIAN_POINT ( 'NONE',  ( 7.200000001229035718, -2.886751345948129988, 4.999999999999997335 ) ) ;
#17126 = CARTESIAN_POINT ( 'NONE',  ( 17.76562500061451644, -6.054752690667223547, -1.112240025338166033E-15 ) ) ;
#17127 = CARTESIAN_POINT ( 'NONE',  ( 12.55312500061451786, 4.541064518000418104, -2.621784821874998173 ) ) ;
#17128 = CARTESIAN_POINT ( 'NONE',  ( 26.40937500061451715, -4.119189519843965641, -2.378215178125001383 ) ) ;
#17129 = CARTESIAN_POINT ( 'NONE',  ( 14.17500000000000071, 4.330127018922191873, 2.499999999999999556 ) ) ;
#17130 = CARTESIAN_POINT ( 'NONE',  ( 8.775000001229033231, 2.886751345948129099, -4.999999999999998224 ) ) ;
#17131 = CARTESIAN_POINT ( 'NONE',  ( 5.090625000614516615, -3.027376345333614438, 5.243569643749998122 ) ) ;
#17132 = ADVANCED_FACE ( 'NONE', ( #33252 ), #50612, .F. ) ;
#17133 = CARTESIAN_POINT ( 'NONE',  ( 17.62500000122903288, -5.773502691896255534, -1.060575238724906372E-15 ) ) ;
#17134 = CARTESIAN_POINT ( 'NONE',  ( 26.62500000000000000, 6.123233995736764310E-16, -4.999999999999998224 ) ) ;
#17135 = AXIS2_PLACEMENT_3D ( 'NONE', #16018, #9753, #67018 ) ;
#17136 = CARTESIAN_POINT ( 'NONE',  ( -4.243569643749997233, 11.79687500061451999, -27.54997392385601174 ) ) ;
#17137 = CARTESIAN_POINT ( 'NONE',  ( 24.00000000000000000, 4.330127018922192761, -2.499999999999997780 ) ) ;
#17138 = VECTOR ( 'NONE', #68347, 1000.000000000000000 ) ;
#17139 = DIRECTION ( 'NONE',  ( -1.000000000000000000, -0.000000000000000000, -0.000000000000000000 ) ) ;
#17140 = CARTESIAN_POINT ( 'NONE',  ( 20.48437500061451289, -4.541064518000419881, 2.621784821874995952 ) ) ;
#17141 =( BOUNDED_CURVE ( )  B_SPLINE_CURVE ( 2, ( #47714, #58418, #25173, #24809, #43195, #38004, #63970 ),
 .UNSPECIFIED., .F., .F. ) 
 B_SPLINE_CURVE_WITH_KNOTS ( ( 3, 2, 2, 3 ),
 ( 0.04000000000000007022, 0.04333333333333339726, 0.04666666666666672431, 0.05000000000000005135 ),
 .UNSPECIFIED. ) 
 CURVE ( )  GEOMETRIC_REPRESENTATION_ITEM ( )  RATIONAL_B_SPLINE_CURVE ( ( 0.9999999999999972244, 0.8660254037844414832, 1.000000000000000000, 0.8660254037844387076, 1.000000000000000000, 0.8660254037844367092, 1.000000000000001998 ) ) 
 REPRESENTATION_ITEM ( '' )  );
#17142 = CARTESIAN_POINT ( 'NONE',  ( 12.30000000000000249, 4.330127018922192761, -2.499999999999997780 ) ) ;
#17143 = VECTOR ( 'NONE', #65213, 1000.000000000000000 ) ;
#17144 = CARTESIAN_POINT ( 'NONE',  ( 16.30312500061451786, 0.000000000000000000, 5.243569643749999010 ) ) ;
#17145 = CARTESIAN_POINT ( 'NONE',  ( 12.31875000122903430, 2.886751345948129099, -4.999999999999998224 ) ) ;
#17146 = CARTESIAN_POINT ( 'NONE',  ( 2.411242101361345515E-14, 20.88124999877096499, 34.00000000000000000 ) ) ;
#17147 = CARTESIAN_POINT ( 'NONE',  ( 14.81250000122903288, 0.000000000000000000, 4.999999999999998224 ) ) ;
#17148 = CARTESIAN_POINT ( 'NONE',  ( 26.40937500061451715, -4.541064518000417216, -2.621784821875001281 ) ) ;
#17149 = CARTESIAN_POINT ( 'NONE',  ( 19.32187500061451857, 4.119189519843966529, 2.378215178124999607 ) ) ;
#17150 = CARTESIAN_POINT ( 'NONE',  ( 11.39062500061451644, -3.027376345333614438, 5.243569643749998122 ) ) ;
#17151 = CARTESIAN_POINT ( 'NONE',  ( 9.759375000614516793, -4.541064518000417216, -2.621784821875001281 ) ) ;
#17152 = VERTEX_POINT ( 'NONE', #39166 ) ;
#17153 = CARTESIAN_POINT ( 'NONE',  ( 2.830238065994760355, -4.121891707590733311, -2.867552304490421200 ) ) ;
#17154 = CARTESIAN_POINT ( 'NONE',  ( 19.30312500061451786, 4.541064518000418104, -2.621784821874998173 ) ) ;
#17155 = CARTESIAN_POINT ( 'NONE',  ( -5.000000000000000000, 39.99999999999999289, 30.00000000000000000 ) ) ;
#17156 = CARTESIAN_POINT ( 'NONE',  ( -3.999999999999999112, 12.91250000122903430, 30.00000000000000000 ) ) ;
#17157 = CARTESIAN_POINT ( 'NONE',  ( 11.21250000000000036, -5.773502691896255534, -1.060575238724906372E-15 ) ) ;
#17158 = CARTESIAN_POINT ( 'NONE',  ( 21.86250000122903003, 4.330127018922192761, -2.499999999999997780 ) ) ;
#17159 = CARTESIAN_POINT ( 'NONE',  ( 16.00312500061451715, -4.541064518000417216, -2.621784821875001281 ) ) ;
#17160 = CARTESIAN_POINT ( 'NONE',  ( 12.42187500061451466, 5.824947211148865298E-16, -4.756430356249998326 ) ) ;
#17161 = ORIENTED_EDGE ( 'NONE', *, *, #40617, .T. ) ;
#17162 = CARTESIAN_POINT ( 'NONE',  ( 20.24999999999999645, -4.330127018922190985, -2.500000000000001332 ) ) ;
#17163 = CARTESIAN_POINT ( 'NONE',  ( 24.22500000000000142, -4.330127018922194537, 2.499999999999995559 ) ) ;
#17164 = CARTESIAN_POINT ( 'NONE',  ( 20.97187500061451715, -6.054752690667223547, -1.112240025338166033E-15 ) ) ;
#17165 = CARTESIAN_POINT ( 'NONE',  ( 25.71562500061451573, 3.027376345333611329, 5.243569643749999010 ) ) ;
#17166 = VERTEX_POINT ( 'NONE', #43984 ) ;
#17167 = DIRECTION ( 'NONE',  ( -1.000000000000000000, -0.000000000000000000, -0.000000000000000000 ) ) ;
#17168 = CARTESIAN_POINT ( 'NONE',  ( 7.715625000614515727, 3.027376345333611329, 5.243569643749999010 ) ) ;
#17169 = LINE ( 'NONE', #72609, #54974 ) ;
#17170 = CARTESIAN_POINT ( 'NONE',  ( 15.26249999999999929, -5.773502691896255534, -1.060575238724906372E-15 ) ) ;
#17171 = CARTESIAN_POINT ( 'NONE',  ( 4.243569643749999010, 17.81562500061451715, 27.54997392385601174 ) ) ;
#17172 = CARTESIAN_POINT ( 'NONE',  ( 4.771875000614516971, -6.054752690667223547, -1.112240025338166033E-15 ) ) ;
#17173 = CARTESIAN_POINT ( 'NONE',  ( 27.27187500061451431, -6.054752690667223547, -1.112240025338166033E-15 ) ) ;
#17174 = ORIENTED_EDGE ( 'NONE', *, *, #8310, .F. ) ;
#17175 = CARTESIAN_POINT ( 'NONE',  ( 23.99062500061451786, -3.027376345333614438, 5.243569643749998122 ) ) ;
#17176 = CARTESIAN_POINT ( 'NONE',  ( 26.18437500061451573, 4.541064518000418104, 2.621784821874999949 ) ) ;
#17177 = EDGE_CURVE ( 'NONE', #23570, #35566, #71960, .T. ) ;
#17178 = CARTESIAN_POINT ( 'NONE',  ( 9.001249775931846008E-16, 19.01562500061459104, -25.09994784771203058 ) ) ;
#17179 = CARTESIAN_POINT ( 'NONE',  ( 11.88749999999999751, 5.773502691896255534, 3.535250795749688894E-16 ) ) ;
#17180 = CARTESIAN_POINT ( 'NONE',  ( 9.778125000614517504, 6.421520780324663323E-16, -5.243569643749999010 ) ) ;
#17181 = DIRECTION ( 'NONE',  ( 0.000000000000000000, 0.000000000000000000, -1.000000000000000000 ) ) ;
#17182 = CARTESIAN_POINT ( 'NONE',  ( 29.72812500061451502, 4.541064518000418104, 2.621784821874999949 ) ) ;
#17183 = CARTESIAN_POINT ( 'NONE',  ( 26.87812500061451360, 6.421520780324663323E-16, -5.243569643749999010 ) ) ;
#17184 = CARTESIAN_POINT ( 'NONE',  ( 12.67500000122903536, -5.773502691896255534, -1.060575238724906372E-15 ) ) ;
#17185 = CARTESIAN_POINT ( 'NONE',  ( 12.72187500061451537, 2.746126346562643317, 4.756430356249998326 ) ) ;
#17186 = CARTESIAN_POINT ( 'NONE',  ( 3.103125000614517237, 4.541064518000418104, -2.621784821874998173 ) ) ;
#17187 = CARTESIAN_POINT ( 'NONE',  ( 18.83437500061451431, 6.421520780324663323E-16, -5.243569643749999010 ) ) ;
#17188 = CARTESIAN_POINT ( 'NONE',  ( 4.243569643749999898, 14.64687500061451964, 32.45002607614398471 ) ) ;
#17189 = CARTESIAN_POINT ( 'NONE',  ( 19.24687500061452283, -3.027376345333610441, -5.243569643749999898 ) ) ;
#17190 = CARTESIAN_POINT ( 'NONE',  ( 29.67187500061451644, 3.027376345333613106, -5.243569643749998122 ) ) ;
#17191 = CARTESIAN_POINT ( 'NONE',  ( 2.121784821875001281, 18.20937500061451786, 33.67503911421598417 ) ) ;
#17192 = CARTESIAN_POINT ( 'NONE',  ( 10.71562500061451928, 3.027376345333613106, -5.243569643749998122 ) ) ;
#17193 = CARTESIAN_POINT ( 'NONE',  ( 7.809375000614519280, 0.000000000000000000, 5.243569643749999010 ) ) ;
#17194 = DIRECTION ( 'NONE',  ( -1.000000000000000000, -0.000000000000000000, -0.000000000000000000 ) ) ;
#17195 = AXIS2_PLACEMENT_3D ( 'NONE', #58964, #2467, #6923 ) ;
#17196 = CARTESIAN_POINT ( 'NONE',  ( 8.728125000614518569, -4.541064518000419881, 2.621784821874995952 ) ) ;
#17197 = CARTESIAN_POINT ( 'NONE',  ( 11.18437500061451928, 6.421520780324663323E-16, -5.243569643749999010 ) ) ;
#17198 = CARTESIAN_POINT ( 'NONE',  ( 19.05000000122903359, -2.886751345948125991, -5.000000000000000000 ) ) ;
#17199 = CARTESIAN_POINT ( 'NONE',  ( 5.971875000614516260, 3.027376345333611329, 5.243569643749999010 ) ) ;
#17200 = CARTESIAN_POINT ( 'NONE',  ( 8.728125000614518569, -4.541064518000419881, 2.621784821874995952 ) ) ;
#17201 = CARTESIAN_POINT ( 'NONE',  ( 1.071796769724490783, 12.59240381056766722, 26.00000000000000000 ) ) ;
#17202 = CARTESIAN_POINT ( 'NONE',  ( 22.55625000122903145, -4.330127018922190985, -2.500000000000001332 ) ) ;
#17203 = CARTESIAN_POINT ( 'NONE',  ( 18.98437500061451644, 4.541064518000418104, 2.621784821874999949 ) ) ;
#17204 = CARTESIAN_POINT ( 'NONE',  ( -3.999999999999999112, 11.56250000122903465, 30.00000000000000000 ) ) ;
#17205 = ORIENTED_EDGE ( 'NONE', *, *, #55050, .F. ) ;
#17206 = CARTESIAN_POINT ( 'NONE',  ( 27.44062500061451715, 6.054752690667223547, 3.707466751127219781E-16 ) ) ;
#17207 = CARTESIAN_POINT ( 'NONE',  ( 13.22812500061451502, -4.541064518000419881, 2.621784821874995952 ) ) ;
#17208 = CARTESIAN_POINT ( 'NONE',  ( 28.47187500061451715, 3.027376345333611329, 5.243569643749999010 ) ) ;
#17209 = CARTESIAN_POINT ( 'NONE',  ( 12.51562500061451821, 3.027376345333613106, -5.243569643749998122 ) ) ;
#17210 = CARTESIAN_POINT ( 'NONE',  ( 4.527409397281981995, -2.122320272585544565, -4.559184932251166167 ) ) ;
#17211 = CARTESIAN_POINT ( 'NONE',  ( 12.18750000122903465, -4.330127018922194537, 2.499999999999995559 ) ) ;
#17212 = CARTESIAN_POINT ( 'NONE',  ( 26.61562500061451786, 3.027376345333611329, 5.243569643749999010 ) ) ;
#17213 = CARTESIAN_POINT ( 'NONE',  ( 4.243569643749999898, 14.59062500061451750, -27.54997392385601529 ) ) ;
#17214 = CARTESIAN_POINT ( 'NONE',  ( 16.16250000122903430, 0.000000000000000000, 4.999999999999998224 ) ) ;
#17215 = VECTOR ( 'NONE', #5085, 1000.000000000000000 ) ;
#17216 = CARTESIAN_POINT ( 'NONE',  ( 13.95000000000000107, -4.330127018922190985, -2.500000000000001332 ) ) ;
#17217 = CARTESIAN_POINT ( 'NONE',  ( 19.71562500061451928, 3.027376345333613106, -5.243569643749998122 ) ) ;
#17218 = CARTESIAN_POINT ( 'NONE',  ( 7.359375000614516438, 0.000000000000000000, 5.243569643749999010 ) ) ;
#17219 = CARTESIAN_POINT ( 'NONE',  ( 7.275000001229035007, -5.773502691896255534, -1.060575238724906372E-15 ) ) ;
#17220 = CARTESIAN_POINT ( 'NONE',  ( 15.78750000122903430, -4.330127018922194537, 2.499999999999995559 ) ) ;
#17221 = CARTESIAN_POINT ( 'NONE',  ( 12.06562500061451537, 3.027376345333613106, -5.243569643749998122 ) ) ;
#17222 = CARTESIAN_POINT ( 'NONE',  ( 15.17812500061451608, 6.421520780324663323E-16, -5.243569643749999010 ) ) ;
#17223 = EDGE_CURVE ( 'NONE', #7111, #27030, #21034, .T. ) ;
#17224 = CARTESIAN_POINT ( 'NONE',  ( 28.01250000122903216, -4.330127018922190985, -2.500000000000001332 ) ) ;
#17225 = CARTESIAN_POINT ( 'NONE',  ( 23.17500000000000071, 4.330127018922191873, 2.499999999999999556 ) ) ;
#17226 = CARTESIAN_POINT ( 'NONE',  ( 23.67187500061451999, -6.054752690667223547, -1.112240025338166033E-15 ) ) ;
#17227 = LINE ( 'NONE', #11699, #38230 ) ;
#17228 = CARTESIAN_POINT ( 'NONE',  ( 9.937500001229032875, -4.330127018922194537, 2.499999999999995559 ) ) ;
#17229 = CARTESIAN_POINT ( 'NONE',  ( 27.53437500061451360, 4.541064518000418104, 2.621784821874999949 ) ) ;
#17230 = CARTESIAN_POINT ( 'NONE',  ( 4.621875000614516615, 3.027376345333611329, 5.243569643749999010 ) ) ;
#17231 = CARTESIAN_POINT ( 'NONE',  ( 22.86562500061451431, 3.027376345333613106, -5.243569643749998122 ) ) ;
#17232 = CARTESIAN_POINT ( 'NONE',  ( 3.756430356250000546, 15.49062499938548321, 27.83122392262697886 ) ) ;
#17233 = CARTESIAN_POINT ( 'NONE',  ( 6.825000000000001066, 6.123233995736764310E-16, -4.999999999999998224 ) ) ;
#17234 = AXIS2_PLACEMENT_3D ( 'NONE', #54953, #60472, #70844 ) ;
#17235 = CARTESIAN_POINT ( 'NONE',  ( 9.234375000614518214, -4.541064518000419881, 2.621784821874995952 ) ) ;
#17236 = CARTESIAN_POINT ( 'NONE',  ( 15.93750000000000000, 5.773502691896255534, 3.535250795749688401E-16 ) ) ;
#17237 = CARTESIAN_POINT ( 'NONE',  ( 29.20312500061451644, 4.541064518000418104, -2.621784821874998173 ) ) ;
#17238 = CARTESIAN_POINT ( 'NONE',  ( 6.984375000614516438, -4.541064518000419881, 2.621784821874995952 ) ) ;
#17239 = CARTESIAN_POINT ( 'NONE',  ( -1.071796769724491005, 14.50759618943233420, 26.00000000000000355 ) ) ;
#17240 = CARTESIAN_POINT ( 'NONE',  ( 25.65937500061451715, 4.541064518000418104, -2.621784821874998173 ) ) ;
#17241 = CARTESIAN_POINT ( 'NONE',  ( -2.121784821874996840, 10.87812500061459531, 33.67503911421598417 ) ) ;
#17242 = CARTESIAN_POINT ( 'NONE',  ( 18.41250000000000142, -5.773502691896255534, -1.060575238724906372E-15 ) ) ;
#17243 = ORIENTED_EDGE ( 'NONE', *, *, #72027, .T. ) ;
#17244 = CARTESIAN_POINT ( 'NONE',  ( 27.37500000000000000, -4.330127018922194537, 2.499999999999995559 ) ) ;
#17245 = CARTESIAN_POINT ( 'NONE',  ( 28.39687500061452141, 6.054752690667223547, 3.707466751127219781E-16 ) ) ;
#17246 = ORIENTED_EDGE ( 'NONE', *, *, #27246, .F. ) ;
#17247 = CARTESIAN_POINT ( 'NONE',  ( 16.67812500061451786, 4.541064518000418104, 2.621784821874999949 ) ) ;
#17248 = CARTESIAN_POINT ( 'NONE',  ( 8.803125000614517859, -4.541064518000417216, -2.621784821875001281 ) ) ;
#17249 = CARTESIAN_POINT ( 'NONE',  ( 18.45937500061451431, 2.746126346562643317, 4.756430356249998326 ) ) ;
#17250 = CARTESIAN_POINT ( 'NONE',  ( 4.284375000614518925, -4.541064518000419881, 2.621784821874995952 ) ) ;
#17251 = CARTESIAN_POINT ( 'NONE',  ( 18.00000000122903288, -2.886751345948129988, 4.999999999999997335 ) ) ;
#17252 = CARTESIAN_POINT ( 'NONE',  ( 22.46250000000000213, -5.773502691896255534, -1.060575238724906372E-15 ) ) ;
#17253 = CARTESIAN_POINT ( 'NONE',  ( 15.75000000000000000, -4.330127018922190985, -2.500000000000001332 ) ) ;
#17254 = CARTESIAN_POINT ( 'NONE',  ( 5.484375000614518214, 4.541064518000418104, 2.621784821874999949 ) ) ;
#17255 = CARTESIAN_POINT ( 'NONE',  ( 11.97187500061451892, -6.054752690667223547, -1.112240025338166033E-15 ) ) ;
#17256 = CARTESIAN_POINT ( 'NONE',  ( 21.30937500061451573, 0.000000000000000000, 5.243569643749999010 ) ) ;
#17257 = CARTESIAN_POINT ( 'NONE',  ( -1.999999999999997113, 16.47500000000000142, 33.46410161513775705 ) ) ;
#17258 = ORIENTED_EDGE ( 'NONE', *, *, #32653, .F. ) ;
#17259 = CARTESIAN_POINT ( 'NONE',  ( 4.959375000614516971, 4.541064518000418104, -2.621784821874998173 ) ) ;
#17260 = CARTESIAN_POINT ( 'NONE',  ( 6.534375000614517148, -4.541064518000419881, 2.621784821874995952 ) ) ;
#17261 = CARTESIAN_POINT ( 'NONE',  ( 18.45000000000000284, -4.330127018922190985, -2.500000000000001332 ) ) ;
#17262 = CARTESIAN_POINT ( 'NONE',  ( 14.95312500061451644, 0.000000000000000000, 5.243569643749999010 ) ) ;
#17263 = CARTESIAN_POINT ( 'NONE',  ( -4.000000000000000888, 18.61250000000000426, 32.30940107675850470 ) ) ;
#17264 = CARTESIAN_POINT ( 'NONE',  ( 26.17500000000000071, 6.123233995736764310E-16, -4.999999999999998224 ) ) ;
#17265 = CARTESIAN_POINT ( 'NONE',  ( 20.14687500061451786, -2.746126346562642428, -4.756430356249999214 ) ) ;
#17266 = CARTESIAN_POINT ( 'NONE',  ( 10.04062500061451502, -3.027376345333614438, 5.243569643749998122 ) ) ;
#17267 = CARTESIAN_POINT ( 'NONE',  ( 26.22187500061451715, 3.027376345333611329, 5.243569643749999010 ) ) ;
#17268 = CARTESIAN_POINT ( 'NONE',  ( 12.71250000000000036, 2.886751345948073588, -5.000000000000094147 ) ) ;
#17269 = CARTESIAN_POINT ( 'NONE',  ( 28.99687500061451573, -3.027376345333614438, 5.243569643749998122 ) ) ;
#17270 = CARTESIAN_POINT ( 'NONE',  ( 10.46249999999999858, 2.886751345948129099, -4.999999999999998224 ) ) ;
#17271 = CARTESIAN_POINT ( 'NONE',  ( 8.484601909799253346E-16, 14.37500000122903288, 34.61880215351700230 ) ) ;
#17272 = CARTESIAN_POINT ( 'NONE',  ( 8.962500001229033231, 0.000000000000000000, 4.999999999999998224 ) ) ;
#17273 = CARTESIAN_POINT ( 'NONE',  ( 19.65937500061451360, -4.541064518000417216, -2.621784821875001281 ) ) ;
#17274 = CARTESIAN_POINT ( 'NONE',  ( 13.32187500061451502, -6.054752690667223547, -1.112240025338166033E-15 ) ) ;
#17275 = CARTESIAN_POINT ( 'NONE',  ( 3.999999999999998668, 13.75624999877096677, 32.30940107675850470 ) ) ;
#17276 = EDGE_LOOP ( 'NONE', ( #61359, #68784, #50990, #14661 ) ) ;
#17277 = CARTESIAN_POINT ( 'NONE',  ( 13.60312500061451679, 0.000000000000000000, 5.243569643749999010 ) ) ;
#17278 = CARTESIAN_POINT ( 'NONE',  ( 26.81250000122903288, 4.330127018922192761, -2.499999999999997780 ) ) ;
#17279 = CARTESIAN_POINT ( 'NONE',  ( 14.37187500061451928, 3.027376345333613106, -5.243569643749998122 ) ) ;
#17280 = AXIS2_PLACEMENT_3D ( 'NONE', #20994, #70882, #43546 ) ;
#17281 = CARTESIAN_POINT ( 'NONE',  ( 1.594043775273461083, 9.879932731042712746, -35.79803503059465442 ) ) ;
#17282 = CARTESIAN_POINT ( 'NONE',  ( 18.02812500061451573, 4.541064518000418104, 2.621784821874999949 ) ) ;
#17283 = DIRECTION ( 'NONE',  ( -1.000000000000000000, -0.000000000000000000, -0.000000000000000000 ) ) ;
#17284 = CARTESIAN_POINT ( 'NONE',  ( 27.08437500061451786, 4.541064518000418104, 2.621784821874999949 ) ) ;
#17285 = CARTESIAN_POINT ( 'NONE',  ( 4.243569643749999898, 10.09062500061451928, 32.45002607614398471 ) ) ;
#17286 = CARTESIAN_POINT ( 'NONE',  ( 14.52187500061451608, 3.027376345333611329, 5.243569643749999010 ) ) ;
#17287 = CARTESIAN_POINT ( 'NONE',  ( 15.33750000122903323, -4.330127018922194537, 2.499999999999995559 ) ) ;
#17288 = CARTESIAN_POINT ( 'NONE',  ( 7.959375000614516971, -4.119189519843965641, -2.378215178125001383 ) ) ;
#17289 = CARTESIAN_POINT ( 'NONE',  ( 2.121784821875001281, 17.75937500061451502, -26.32496088578401938 ) ) ;
#17290 = CARTESIAN_POINT ( 'NONE',  ( 19.32187500061451857, 3.027376345333613106, -5.243569643749998122 ) ) ;
#17291 = CARTESIAN_POINT ( 'NONE',  ( 20.25000000122903288, -2.886751345948129988, 4.999999999999997335 ) ) ;
#17292 = CARTESIAN_POINT ( 'NONE',  ( 14.14687500061451786, -3.027376345333614438, 5.243569643749998122 ) ) ;
#17293 = EDGE_CURVE ( 'NONE', #28919, #42612, #69157, .T. ) ;
#17294 = CARTESIAN_POINT ( 'NONE',  ( 4.243569643749999898, 12.88437500061451857, 30.00000000000000000 ) ) ;
#17295 = CARTESIAN_POINT ( 'NONE',  ( 23.21250000122903501, 4.330127018922192761, -2.499999999999997780 ) ) ;
#17296 = AXIS2_PLACEMENT_3D ( 'NONE', #35839, #51761, #30668 ) ;
#17297 = CARTESIAN_POINT ( 'NONE',  ( 16.11562500061451786, 3.027376345333613106, -5.243569643749998122 ) ) ;
#17298 = DIRECTION ( 'NONE',  ( 0.000000000000000000, 0.000000000000000000, -1.000000000000000000 ) ) ;
#17299 = VERTEX_POINT ( 'NONE', #7351 ) ;
#17300 = ORIENTED_EDGE ( 'NONE', *, *, #1804, .F. ) ;
#17301 = CARTESIAN_POINT ( 'NONE',  ( 21.44999999999999929, 0.000000000000000000, 4.999999999999998224 ) ) ;
#17302 = CARTESIAN_POINT ( 'NONE',  ( -2.000000000000000000, 17.78750000122903430, 26.53589838486224650 ) ) ;
#17303 = CARTESIAN_POINT ( 'NONE',  ( 3.553125000614516082, 4.541064518000418104, -2.621784821874998173 ) ) ;
#17304 = CARTESIAN_POINT ( 'NONE',  ( 14.51250000122903394, -4.330127018922190985, -2.500000000000001332 ) ) ;
#17305 = CARTESIAN_POINT ( 'NONE',  ( 18.89062500061451644, 6.054752690667223547, 3.707466751127219781E-16 ) ) ;
#17306 =( BOUNDED_CURVE ( )  B_SPLINE_CURVE ( 2, ( #20770, #42950, #65478, #20029, #14135, #33232, #2697, #60287, #36311 ),
 .UNSPECIFIED., .F., .F. ) 
 B_SPLINE_CURVE_WITH_KNOTS ( ( 3, 2, 2, 2, 3 ),
 ( 0.9305555555555555802, 0.9351851851851852304, 0.9444444444444444198, 0.9537037037037037202, 0.9583333333333333703 ),
 .UNSPECIFIED. ) 
 CURVE ( )  GEOMETRIC_REPRESENTATION_ITEM ( )  RATIONAL_B_SPLINE_CURVE ( ( 0.9330127018922194093, 0.9330127018922194093, 1.000000000000000000, 0.8660254037844387076, 1.000000000000000000, 0.8660254037844387076, 1.000000000000000000, 0.9330127018922185211, 0.9330127018922192983 ) ) 
 REPRESENTATION_ITEM ( '' )  );
#17307 = CARTESIAN_POINT ( 'NONE',  ( 22.41562500061451502, 3.027376345333613106, -5.243569643749998122 ) ) ;
#17308 = CARTESIAN_POINT ( 'NONE',  ( 5.953125000614519102, 0.000000000000000000, 5.243569643749999010 ) ) ;
#17309 = ADVANCED_FACE ( 'NONE', ( #51334 ), #18054, .F. ) ;
#17310 = CARTESIAN_POINT ( 'NONE',  ( 29.55000000000000071, 0.000000000000000000, 4.999999999999998224 ) ) ;
#17311 = CARTESIAN_POINT ( 'NONE',  ( 9.684375000614517504, -4.119189519843968306, 2.378215178124996054 ) ) ;
#17312 = DIRECTION ( 'NONE',  ( 0.000000000000000000, 0.000000000000000000, -1.000000000000000000 ) ) ;
#17313 = CARTESIAN_POINT ( 'NONE',  ( -3.999999999999997335, 10.25000000122903288, -27.69059892324149175 ) ) ;
#17314 = CARTESIAN_POINT ( 'NONE',  ( -3.000416591977282496E-16, 18.84687500061452070, -34.90005215228797653 ) ) ;
#17315 = CARTESIAN_POINT ( 'NONE',  ( 6.412500001229036073, -4.330127018922190985, -2.500000000000001332 ) ) ;
#17316 = CARTESIAN_POINT ( 'NONE',  ( 9.412499999999999645, -5.773502691896255534, -1.060575238724906372E-15 ) ) ;
#17317 = ADVANCED_FACE ( 'NONE', ( #6636 ), #68694, .T. ) ;
#17318 = CARTESIAN_POINT ( 'NONE',  ( 5.212500001229032343, 4.330127018922192761, -2.499999999999997780 ) ) ;
#17319 = CARTESIAN_POINT ( 'NONE',  ( 11.85937500061451644, 0.000000000000000000, 5.243569643749999010 ) ) ;
#17320 = CARTESIAN_POINT ( 'NONE',  ( 23.58750000122903145, 6.123233995736764310E-16, -4.999999999999998224 ) ) ;
#17321 = CARTESIAN_POINT ( 'NONE',  ( 4.771875000614516971, -6.054752690667223547, -1.112240025338166033E-15 ) ) ;
#17322 = CARTESIAN_POINT ( 'NONE',  ( -1.626862140677534273E-15, 17.78749999999999787, 34.00000000000000000 ) ) ;
#17323 = CARTESIAN_POINT ( 'NONE',  ( 29.51250000122903216, 4.330127018922192761, -2.499999999999997780 ) ) ;
#17324 = CARTESIAN_POINT ( 'NONE',  ( 10.77187500061451786, 3.027376345333613106, -5.243569643749998122 ) ) ;
#17325 = CARTESIAN_POINT ( 'NONE',  ( 14.67187500061451821, -6.054752690667223547, -1.112240025338166033E-15 ) ) ;
#17326 = CARTESIAN_POINT ( 'NONE',  ( 7.320879633048903241E-15, 17.30000000122903003, -34.00000000000000000 ) ) ;
#17327 = CARTESIAN_POINT ( 'NONE',  ( 6.150000000000003020, 0.000000000000000000, 4.999999999999998224 ) ) ;
#17328 = CARTESIAN_POINT ( 'NONE',  ( 2.121784821875001281, 16.35312500061459318, 33.67503911421598417 ) ) ;
#17329 = CARTESIAN_POINT ( 'NONE',  ( 20.78437500061451715, 4.541064518000418104, 2.621784821874999949 ) ) ;
#17330 = CARTESIAN_POINT ( 'NONE',  ( 9.750000000000001776, 0.000000000000000000, 4.999999999999998224 ) ) ;
#17331 = CARTESIAN_POINT ( 'NONE',  ( 27.71250000122903145, 4.330127018922192761, -2.499999999999997780 ) ) ;
#17332 = CARTESIAN_POINT ( 'NONE',  ( 18.19687500061451502, -4.119189519843965641, -2.378215178125001383 ) ) ;
#17333 = CARTESIAN_POINT ( 'NONE',  ( 22.30312500061451431, -4.541064518000417216, -2.621784821875001281 ) ) ;
#17334 = CARTESIAN_POINT ( 'NONE',  ( 14.95312500061451644, 0.000000000000000000, 5.243569643749999010 ) ) ;
#17335 = CARTESIAN_POINT ( 'NONE',  ( 25.69687500061451502, 0.000000000000000000, 4.756430356249998326 ) ) ;
#17336 = CARTESIAN_POINT ( 'NONE',  ( 12.23437500061451821, 4.541064518000418104, 2.621784821874999949 ) ) ;
#17337 = CARTESIAN_POINT ( 'NONE',  ( 27.59999999999999787, 4.330127018922192761, -2.499999999999997780 ) ) ;
#17338 = CARTESIAN_POINT ( 'NONE',  ( 24.71250000122903145, 0.000000000000000000, 4.999999999999998224 ) ) ;
#17339 = CARTESIAN_POINT ( 'NONE',  ( 3.346875000614518036, -3.027376345333614438, 5.243569643749998122 ) ) ;
#17340 = CARTESIAN_POINT ( 'NONE',  ( 14.03437500061451715, 4.541064518000418104, 2.621784821874999949 ) ) ;
#17341 = CARTESIAN_POINT ( 'NONE',  ( 29.37187500061451928, 3.027376345333611329, 5.243569643749999010 ) ) ;
#17342 = CARTESIAN_POINT ( 'NONE',  ( 21.86250000000000426, 2.886751345948126879, 4.999999999999998224 ) ) ;
#17343 = CARTESIAN_POINT ( 'NONE',  ( 18.45000000000000284, -4.330127018922190985, -2.500000000000001332 ) ) ;
#17344 = CARTESIAN_POINT ( 'NONE',  ( 23.55937500061451573, 0.000000000000000000, 5.243569643749999010 ) ) ;
#17345 = CARTESIAN_POINT ( 'NONE',  ( 14.22187500061451537, -6.054752690667223547, -1.112240025338166033E-15 ) ) ;
#17346 = CARTESIAN_POINT ( 'NONE',  ( -3.756430356250000102, 15.22812499938548392, 30.00000000000000000 ) ) ;
#17347 = CARTESIAN_POINT ( 'NONE',  ( 25.23749999999999716, -2.886751345948125991, -5.000000000000000000 ) ) ;
#17348 = CARTESIAN_POINT ( 'NONE',  ( 3.337500001229034563, 6.123233995736764310E-16, -4.999999999999998224 ) ) ;
#17349 = CARTESIAN_POINT ( 'NONE',  ( 28.09687500061451360, -2.746126346562646425, 4.756430356249996549 ) ) ;
#17350 = CARTESIAN_POINT ( 'NONE',  ( 16.15312500061451573, 4.541064518000418104, -2.621784821874998173 ) ) ;
#17351 = CARTESIAN_POINT ( 'NONE',  ( 6.225000000000001421, -4.330127018922194537, 2.499999999999995559 ) ) ;
#17352 = EDGE_CURVE ( 'NONE', #20497, #11634, #13242, .T. ) ;
#17353 = CARTESIAN_POINT ( 'NONE',  ( -3.999999999999999112, 14.11250000000000071, 27.69059892324149885 ) ) ;
#17354 =( BOUNDED_CURVE ( )  B_SPLINE_CURVE ( 3, ( #19593, #58027, #20327, #42881 ),
 .UNSPECIFIED., .F., .F. ) 
 B_SPLINE_CURVE_WITH_KNOTS ( ( 4, 4 ),
 ( 0.8238030042635362538, 0.8534874751081462652 ),
 .UNSPECIFIED. ) 
 CURVE ( )  GEOMETRIC_REPRESENTATION_ITEM ( )  RATIONAL_B_SPLINE_CURVE ( ( 1.000000000000000000, 0.9999265706972281231, 0.9999265706972281231, 1.000000000000000000 ) ) 
 REPRESENTATION_ITEM ( '' )  );
#17355 = CARTESIAN_POINT ( 'NONE',  ( 16.31250000000000000, 2.886751345948129099, -4.999999999999998224 ) ) ;
#17356 = CARTESIAN_POINT ( 'NONE',  ( 9.001249775931846008E-16, 12.71562500061451750, 34.90005215228797653 ) ) ;
#17357 = CARTESIAN_POINT ( 'NONE',  ( -1.071796769724496334, 16.23259618943233562, 26.00000000000000355 ) ) ;
#17358 = CARTESIAN_POINT ( 'NONE',  ( 21.82500000122903572, 2.886751345948129099, -4.999999999999998224 ) ) ;
#17359 = CARTESIAN_POINT ( 'NONE',  ( 27.75937500061451502, -4.541064518000417216, -2.621784821875001281 ) ) ;
#17360 = EDGE_LOOP ( 'NONE', ( #935, #29743, #66525, #11899 ) ) ;
#17361 = CARTESIAN_POINT ( 'NONE',  ( 21.10312500061451502, 4.541064518000418104, -2.621784821874998173 ) ) ;
#17362 = CARTESIAN_POINT ( 'NONE',  ( 21.45937500061451786, -4.541064518000417216, -2.621784821875001281 ) ) ;
#17363 = CARTESIAN_POINT ( 'NONE',  ( 3.450000000000001510, 0.000000000000000000, 4.999999999999998224 ) ) ;
#17364 = CARTESIAN_POINT ( 'NONE',  ( 10.30312500061451431, 4.541064518000418104, -2.621784821874998173 ) ) ;
#17365 = CARTESIAN_POINT ( 'NONE',  ( 23.84062500061451928, 6.054752690667223547, 3.707466751127219781E-16 ) ) ;
#17366 = CARTESIAN_POINT ( 'NONE',  ( 13.13437500061451857, 4.541064518000418104, 2.621784821874999949 ) ) ;
#17367 = CARTESIAN_POINT ( 'NONE',  ( 15.87187500061451573, 3.027376345333611329, 5.243569643749999010 ) ) ;
#17368 = CARTESIAN_POINT ( 'NONE',  ( 2.121784821875001281, 17.70312500061451644, 33.67503911421598417 ) ) ;
#17369 = CARTESIAN_POINT ( 'NONE',  ( 20.66250000122903074, 0.000000000000000000, 4.999999999999998224 ) ) ;
#17370 = CARTESIAN_POINT ( 'NONE',  ( 14.07187500061451679, 2.746126346562643317, 4.756430356249998326 ) ) ;
#17371 = CARTESIAN_POINT ( 'NONE',  ( 10.97812500061451679, -4.541064518000419881, 2.621784821874995952 ) ) ;
#17372 = CARTESIAN_POINT ( 'NONE',  ( 4.846875000614519813, -3.027376345333610441, -5.243569643749999898 ) ) ;
#17373 = CARTESIAN_POINT ( 'NONE',  ( 3.646875000614520079, 6.054752690667223547, 3.707466751127219781E-16 ) ) ;
#17374 = ORIENTED_EDGE ( 'NONE', *, *, #431, .F. ) ;
#17375 = CARTESIAN_POINT ( 'NONE',  ( 25.73437500061451644, 4.541064518000418104, 2.621784821874999949 ) ) ;
#17376 = CARTESIAN_POINT ( 'NONE',  ( 17.95312500061451644, 4.541064518000418104, -2.621784821874998173 ) ) ;
#17377 = CARTESIAN_POINT ( 'NONE',  ( 28.46250000122903145, -4.330127018922190985, -2.500000000000001332 ) ) ;
#17378 = CARTESIAN_POINT ( 'NONE',  ( 28.82812500061451644, 4.541064518000418104, 2.621784821874999949 ) ) ;
#17379 = CARTESIAN_POINT ( 'NONE',  ( 22.54687500061451999, 6.054752690667223547, 3.707466751127219781E-16 ) ) ;
#17380 = CARTESIAN_POINT ( 'NONE',  ( 17.09062500061451573, 6.054752690667223547, 3.707466751127219781E-16 ) ) ;
#17381 = CARTESIAN_POINT ( 'NONE',  ( 9.001249775931846008E-16, 19.07187500061451502, 34.90005215228797653 ) ) ;
#17382 = CARTESIAN_POINT ( 'NONE',  ( 23.27812500061451573, 6.421520780324663323E-16, -5.243569643749999010 ) ) ;
#17383 = CARTESIAN_POINT ( 'NONE',  ( 3.787500001229033408, 6.123233995736764310E-16, -4.999999999999998224 ) ) ;
#17384 = ORIENTED_EDGE ( 'NONE', *, *, #26884, .F. ) ;
#17385 = CARTESIAN_POINT ( 'NONE',  ( 27.67499999999999716, 4.330127018922191873, 2.499999999999999556 ) ) ;
#17386 = CARTESIAN_POINT ( 'NONE',  ( -3.999999999999999556, 11.86250000000000071, -32.30940107675850470 ) ) ;
#17387 = CARTESIAN_POINT ( 'NONE',  ( 1.878215178125000495, 17.77812499938548285, 26.74683588394047007 ) ) ;
#17388 = ADVANCED_FACE ( 'NONE', ( #63133 ), #68331, .F. ) ;
#17389 = CARTESIAN_POINT ( 'NONE',  ( 3.384375000614517237, -4.541064518000419881, 2.621784821874995952 ) ) ;
#17390 = CARTESIAN_POINT ( 'NONE',  ( 11.31562500061451892, 3.027376345333611329, 5.243569643749999010 ) ) ;
#17391 = CARTESIAN_POINT ( 'NONE',  ( 23.36250000122903359, 0.000000000000000000, 4.999999999999998224 ) ) ;
#17392 = CARTESIAN_POINT ( 'NONE',  ( 12.60937500061451821, 4.541064518000418104, -2.621784821874998173 ) ) ;
#17393 = CARTESIAN_POINT ( 'NONE',  ( 26.16562500061451502, 3.027376345333611329, 5.243569643749999010 ) ) ;
#17394 = CARTESIAN_POINT ( 'NONE',  ( 27.37500000000000000, -4.330127018922194537, 2.499999999999995559 ) ) ;
#17395 = CARTESIAN_POINT ( 'NONE',  ( 3.999999999999998668, 17.67500000122903359, -32.30940107675850470 ) ) ;
#17396 = CARTESIAN_POINT ( 'NONE',  ( -1.071796769724496556, 15.70490381179669903, -26.00000000000000355 ) ) ;
#17397 = CARTESIAN_POINT ( 'NONE',  ( 11.95312500061451644, -4.541064518000417216, -2.621784821875001281 ) ) ;
#17398 = ORIENTED_EDGE ( 'NONE', *, *, #19782, .F. ) ;
#17399 = CARTESIAN_POINT ( 'NONE',  ( 6.965625000614518392, -6.054752690667223547, -1.112240025338166033E-15 ) ) ;
#17400 = CARTESIAN_POINT ( 'NONE',  ( 6.890625000614516438, -3.027376345333614438, 5.243569643749998122 ) ) ;
#17401 = CARTESIAN_POINT ( 'NONE',  ( 16.73437500061451644, 4.119189519843966529, 2.378215178124999607 ) ) ;
#17402 = CARTESIAN_POINT ( 'NONE',  ( 14.02500000122903323, -5.773502691896255534, -1.060575238724906372E-15 ) ) ;
#17403 = CARTESIAN_POINT ( 'NONE',  ( 15.15000000000000036, 0.000000000000000000, 4.999999999999998224 ) ) ;
#17404 = CARTESIAN_POINT ( 'NONE',  ( 16.43437500061451573, -4.541064518000419881, 2.621784821874995952 ) ) ;
#17405 = CARTESIAN_POINT ( 'NONE',  ( 10.65000000122903323, 5.773502691896255534, 3.535250795749688894E-16 ) ) ;
#17406 = CARTESIAN_POINT ( 'NONE',  ( 19.95937500061451786, 0.000000000000000000, 5.243569643749999010 ) ) ;
#17407 = CARTESIAN_POINT ( 'NONE',  ( 19.98749999999999716, 5.773502691896255534, 3.535250795749688894E-16 ) ) ;
#17408 = CARTESIAN_POINT ( 'NONE',  ( 19.69687500061451857, -3.027376345333610441, -5.243569643749999898 ) ) ;
#17409 = CARTESIAN_POINT ( 'NONE',  ( 4.243569643749999898, 14.59062500061451750, -27.54997392385601529 ) ) ;
#17410 = CARTESIAN_POINT ( 'NONE',  ( -2.000000000000000000, 16.77500000000000213, 26.53589838486224650 ) ) ;
#17411 = CARTESIAN_POINT ( 'NONE',  ( 24.57187500061451502, 5.824947211148865298E-16, -4.756430356249998326 ) ) ;
#17412 = CARTESIAN_POINT ( 'NONE',  ( 4.133697246135442427, 2.812954343170202431, 4.425208334576621105 ) ) ;
#17413 = CARTESIAN_POINT ( 'NONE',  ( 26.95312500061451644, 4.541064518000418104, -2.621784821874998173 ) ) ;
#17414 = CARTESIAN_POINT ( 'NONE',  ( 17.17500000122903359, -5.773502691896255534, -1.060575238724906372E-15 ) ) ;
#17415 = CARTESIAN_POINT ( 'NONE',  ( 28.32187500061451502, 3.027376345333613106, -5.243569643749998122 ) ) ;
#17416 = CARTESIAN_POINT ( 'NONE',  ( 24.33749999999999858, -2.886751345948125991, -5.000000000000000000 ) ) ;
#17417 = CARTESIAN_POINT ( 'NONE',  ( 8.990625000614516082, 6.054752690667223547, 3.707466751127219781E-16 ) ) ;
#17418 = CARTESIAN_POINT ( 'NONE',  ( 24.19687500061451502, 4.119189519843966529, -2.378215178124998275 ) ) ;
#17419 = CARTESIAN_POINT ( 'NONE',  ( 18.53437500061451715, 4.541064518000418104, 2.621784821874999949 ) ) ;
#17420 = CARTESIAN_POINT ( 'NONE',  ( 10.84687500061451715, 0.000000000000000000, 4.756430356249998326 ) ) ;
#17421 = CARTESIAN_POINT ( 'NONE',  ( 5.803125000614517859, 4.541064518000418104, -2.621784821874998173 ) ) ;
#17422 = CARTESIAN_POINT ( 'NONE',  ( 10.02187500061451964, 3.027376345333611329, 5.243569643749999010 ) ) ;
#17423 = VERTEX_POINT ( 'NONE', #57944 ) ;
#17424 = CARTESIAN_POINT ( 'NONE',  ( 21.23437500061451644, 4.541064518000418104, 2.621784821874999949 ) ) ;
#17425 = CARTESIAN_POINT ( 'NONE',  ( 8.118750001229031454, -5.773502691896255534, -1.060575238724906372E-15 ) ) ;
#17426 = CARTESIAN_POINT ( 'NONE',  ( 29.40937500061451715, 0.000000000000000000, 5.243569643749999010 ) ) ;
#17427 = AXIS2_PLACEMENT_3D ( 'NONE', #61543, #5407, #27944 ) ;
#17428 = DIRECTION ( 'NONE',  ( 0.000000000000000000, 0.000000000000000000, 1.000000000000000000 ) ) ;
#17429 = CARTESIAN_POINT ( 'NONE',  ( 3.365625000614516082, -6.054752690667223547, -1.112240025338166033E-15 ) ) ;
#17430 = EDGE_LOOP ( 'NONE', ( #11648, #46745, #28254, #37515 ) ) ;
#17431 = CARTESIAN_POINT ( 'NONE',  ( 10.38750000000000107, -2.886751345948125991, -5.000000000000000000 ) ) ;
#17432 = CARTESIAN_POINT ( 'NONE',  ( 13.43437500061451750, 5.492252693125287522, 3.363034840372157021E-16 ) ) ;
#17433 = CARTESIAN_POINT ( 'NONE',  ( 24.55312500061451786, -4.541064518000417216, -2.621784821875001281 ) ) ;
#17434 = CARTESIAN_POINT ( 'NONE',  ( 14.36249999999999893, -5.773502691896255534, -1.060575238724906372E-15 ) ) ;
#17435 = CARTESIAN_POINT ( 'NONE',  ( 10.98750000122903536, 6.123233995736764310E-16, -4.999999999999998224 ) ) ;
#17436 = CARTESIAN_POINT ( 'NONE',  ( 7.790625000614518569, -3.027376345333614438, 5.243569643749998122 ) ) ;
#17437 = EDGE_CURVE ( 'NONE', #61419, #36820, #57589, .T. ) ;
#17438 = CARTESIAN_POINT ( 'NONE',  ( 9.674999999999998934, 4.330127018922191873, 2.499999999999999556 ) ) ;
#17439 = DIRECTION ( 'NONE',  ( -0.000000000000000000, -1.000000000000000000, -0.000000000000000000 ) ) ;
#17440 = CARTESIAN_POINT ( 'NONE',  ( 29.06250000122903288, 4.330127018922192761, -2.499999999999997780 ) ) ;
#17441 = CARTESIAN_POINT ( 'NONE',  ( 1.878215178124997609, 16.61562499938548143, 33.25316411605952993 ) ) ;
#17442 = CARTESIAN_POINT ( 'NONE',  ( 7.912499999999999645, 2.886751345948126879, 4.999999999999999112 ) ) ;
#17443 = LINE ( 'NONE', #33719, #6693 ) ;
#17444 = ORIENTED_EDGE ( 'NONE', *, *, #33444, .T. ) ;
#17445 = CARTESIAN_POINT ( 'NONE',  ( 23.09062500061451573, -3.027376345333614438, 5.243569643749998122 ) ) ;
#17446 = CARTESIAN_POINT ( 'NONE',  ( 28.26562500061451289, 3.027376345333613106, -5.243569643749998122 ) ) ;
#17447 = CARTESIAN_POINT ( 'NONE',  ( 29.52187500061451431, -6.054752690667223547, -1.112240025338166033E-15 ) ) ;
#17448 = CARTESIAN_POINT ( 'NONE',  ( 19.47187500061451360, 3.027376345333611329, 5.243569643749999010 ) ) ;
#17449 = CARTESIAN_POINT ( 'NONE',  ( 16.19062500061451715, 6.054752690667223547, 3.707466751127219781E-16 ) ) ;
#17450 = CARTESIAN_POINT ( 'NONE',  ( -3.000416591977282496E-16, 10.69062500061459531, -34.90005215228797653 ) ) ;
#17451 = CARTESIAN_POINT ( 'NONE',  ( 5.240625000614516971, -3.027376345333610441, -5.243569643749999898 ) ) ;
#17452 = CARTESIAN_POINT ( 'NONE',  ( 27.82500000122903572, 2.886751345948126879, 4.999999999999999112 ) ) ;
#17453 = CARTESIAN_POINT ( 'NONE',  ( 22.05937500061451573, 4.119189519843966529, -2.378215178124998275 ) ) ;
#17454 = CARTESIAN_POINT ( 'NONE',  ( 19.07812500061451644, -4.541064518000419881, 2.621784821874995952 ) ) ;
#17455 = DIRECTION ( 'NONE',  ( 0.000000000000000000, 0.000000000000000000, 1.000000000000000000 ) ) ;
#17456 = CARTESIAN_POINT ( 'NONE',  ( 4.087500001229035007, -4.330127018922194537, 2.499999999999995559 ) ) ;
#17457 = CARTESIAN_POINT ( 'NONE',  ( 12.42187500061451821, -6.054752690667223547, -1.112240025338166033E-15 ) ) ;
#17458 = CARTESIAN_POINT ( 'NONE',  ( 13.09687500061451892, 6.054752690667223547, 3.707466751127219781E-16 ) ) ;
#17459 = CARTESIAN_POINT ( 'NONE',  ( 20.48437500061451289, -4.541064518000419881, 2.621784821874995952 ) ) ;
#17460 = ORIENTED_EDGE ( 'NONE', *, *, #60559, .F. ) ;
#17461 = CARTESIAN_POINT ( 'NONE',  ( 25.11562500061451431, 3.027376345333613106, -5.243569643749998122 ) ) ;
#17462 = CARTESIAN_POINT ( 'NONE',  ( 18.34687500061451715, -3.027376345333610441, -5.243569643749999898 ) ) ;
#17463 = CARTESIAN_POINT ( 'NONE',  ( 24.89062500061451644, -3.027376345333614438, 5.243569643749998122 ) ) ;
#17464 = CARTESIAN_POINT ( 'NONE',  ( 15.16875000122903394, 2.886751345948182834, 4.999999999999902300 ) ) ;
#17465 = CARTESIAN_POINT ( 'NONE',  ( -3.999999999999999556, 15.91249999999999964, 27.69059892324149530 ) ) ;
#17466 = CARTESIAN_POINT ( 'NONE',  ( 29.24062500061451431, 6.054752690667223547, 3.707466751127219781E-16 ) ) ;
#17467 = CARTESIAN_POINT ( 'NONE',  ( 12.30000000122903181, -2.886751345948125991, -5.000000000000000000 ) ) ;
#17468 = CARTESIAN_POINT ( 'NONE',  ( 7.125000001229033764, 2.886751345948126879, 4.999999999999999112 ) ) ;
#17469 = CARTESIAN_POINT ( 'NONE',  ( -2.000000000000000000, 19.92500000000000071, -33.46410161513775705 ) ) ;
#17470 = CARTESIAN_POINT ( 'NONE',  ( 27.37500000122903288, 2.886751345948126879, 4.999999999999999112 ) ) ;
#17471 = CARTESIAN_POINT ( 'NONE',  ( 4.000000000000000000, 18.33124999877096784, 27.69059892324149530 ) ) ;
#17472 = CARTESIAN_POINT ( 'NONE',  ( 15.50625000122903430, 4.330127018922192761, -2.499999999999997780 ) ) ;
#17473 = CARTESIAN_POINT ( 'NONE',  ( 9.834375000614517859, 6.421520780324663323E-16, -5.243569643749999010 ) ) ;
#17474 = CARTESIAN_POINT ( 'NONE',  ( -2.672702088255949472E-15, 13.06250000000000355, 26.00000000000000000 ) ) ;
#17475 = CARTESIAN_POINT ( 'NONE',  ( 16.64062500061451289, 6.054752690667223547, 3.707466751127219781E-16 ) ) ;
#17476 = CARTESIAN_POINT ( 'NONE',  ( 12.45937500061451786, -4.541064518000417216, -2.621784821875001281 ) ) ;
#17477 = CARTESIAN_POINT ( 'NONE',  ( 28.83750000122903145, -4.330127018922194537, 2.499999999999995559 ) ) ;
#17478 = CARTESIAN_POINT ( 'NONE',  ( 20.59687500061451715, -3.027376345333610441, -5.243569643749999898 ) ) ;
#17479 = CARTESIAN_POINT ( 'NONE',  ( 6.421875000614519102, 3.027376345333611329, 5.243569643749999010 ) ) ;
#17480 = CARTESIAN_POINT ( 'NONE',  ( 3.590625000614518836, 6.054752690667223547, 3.707466751127219781E-16 ) ) ;
#17481 = CARTESIAN_POINT ( 'NONE',  ( 22.34999999999999787, 0.000000000000000000, 4.999999999999998224 ) ) ;
#17482 = CARTESIAN_POINT ( 'NONE',  ( 10.90312500061451928, 0.000000000000000000, 5.243569643749999010 ) ) ;
#17483 = CARTESIAN_POINT ( 'NONE',  ( 20.24062500061451431, 6.054752690667223547, 3.707466751127219781E-16 ) ) ;
#17484 = VERTEX_POINT ( 'NONE', #29523 ) ;
#17485 = CARTESIAN_POINT ( 'NONE',  ( 5.925000001229033586, -5.773502691896255534, -1.060575238724906372E-15 ) ) ;
#17486 = CARTESIAN_POINT ( 'NONE',  ( 17.35312500061451502, -4.541064518000417216, -2.621784821875001281 ) ) ;
#17487 = CARTESIAN_POINT ( 'NONE',  ( 12.36562500061451608, -6.054752690667223547, -1.112240025338166033E-15 ) ) ;
#17488 = CARTESIAN_POINT ( 'NONE',  ( 22.39687500061451075, -2.746126346562642428, -4.756430356249999214 ) ) ;
#17489 = CARTESIAN_POINT ( 'NONE',  ( 12.93750000000000178, -2.886751345948129988, 4.999999999999997335 ) ) ;
#17490 = CARTESIAN_POINT ( 'NONE',  ( 8.437500001229034652, 4.330127018922191873, 2.499999999999999556 ) ) ;
#17491 = EDGE_CURVE ( 'NONE', #40395, #64264, #53607, .T. ) ;
#17492 = CARTESIAN_POINT ( 'NONE',  ( 6.140625000614516438, -3.027376345333610441, -5.243569643749999898 ) ) ;
#17493 = CARTESIAN_POINT ( 'NONE',  ( 17.81250000122903288, 4.330127018922192761, -2.499999999999997780 ) ) ;
#17494 = CARTESIAN_POINT ( 'NONE',  ( 27.11249999999999716, 2.886751345948129099, -4.999999999999998224 ) ) ;
#17495 = CARTESIAN_POINT ( 'NONE',  ( -4.243569643749997233, 10.89687500061451786, -27.54997392385601174 ) ) ;
#17496 = CARTESIAN_POINT ( 'NONE',  ( -2.498395430326213790E-14, 20.65624999877097068, 26.00000000000000000 ) ) ;
#17497 = CARTESIAN_POINT ( 'NONE',  ( 3.375000001229033320, 2.886751345948129099, -4.999999999999998224 ) ) ;
#17498 = CYLINDRICAL_SURFACE ( 'NONE', #3331, 4.000000000000000000 ) ;
#17499 = CARTESIAN_POINT ( 'NONE',  ( 18.19687500061451502, -3.027376345333614438, 5.243569643749998122 ) ) ;
#17500 = CARTESIAN_POINT ( 'NONE',  ( -3.999999999999999112, 16.47500000122903430, 27.69059892324149885 ) ) ;
#17501 = CARTESIAN_POINT ( 'NONE',  ( 15.62812500061451537, 6.421520780324663323E-16, -5.243569643749999010 ) ) ;
#17502 = CARTESIAN_POINT ( 'NONE',  ( 9.356250001229033941, 0.000000000000000000, 4.999999999999998224 ) ) ;
#17503 = CARTESIAN_POINT ( 'NONE',  ( 9.000000000000001776, -4.330127018922190985, -2.500000000000001332 ) ) ;
#17504 = CARTESIAN_POINT ( 'NONE',  ( 29.40937500061451715, 0.000000000000000000, 5.243569643749999010 ) ) ;
#17505 = CARTESIAN_POINT ( 'NONE',  ( 25.09687500061451715, -3.027376345333610441, -5.243569643749999898 ) ) ;
#17506 = CARTESIAN_POINT ( 'NONE',  ( 18.15937500061451360, -5.492252693125287522, -1.008910452111647106E-15 ) ) ;
#17507 = CARTESIAN_POINT ( 'NONE',  ( 12.44062500061451537, -3.027376345333610441, -5.243569643749999898 ) ) ;
#17508 = CARTESIAN_POINT ( 'NONE',  ( 10.47187500061451715, 3.027376345333611329, 5.243569643749999010 ) ) ;
#17509 = VERTEX_POINT ( 'NONE', #63498 ) ;
#17510 = CARTESIAN_POINT ( 'NONE',  ( 29.50312500061451360, -4.541064518000417216, -2.621784821875001281 ) ) ;
#17511 = CARTESIAN_POINT ( 'NONE',  ( 21.21562500061451573, 3.027376345333611329, 5.243569643749999010 ) ) ;
#17512 = CARTESIAN_POINT ( 'NONE',  ( 27.78750000000000142, -2.886751345948157965, 4.999999999999948486 ) ) ;
#17513 = CARTESIAN_POINT ( 'NONE',  ( 4.907911205059083602E-16, 5.000000000000000000, -26.00000000000000000 ) ) ;
#17514 = CARTESIAN_POINT ( 'NONE',  ( 10.87500000000000000, 6.123233995736764310E-16, -4.999999999999998224 ) ) ;
#17515 = CARTESIAN_POINT ( 'NONE',  ( 21.75000000122903288, -2.886751345948125991, -5.000000000000000000 ) ) ;
#17516 = CARTESIAN_POINT ( 'NONE',  ( 15.36562500061451608, 3.027376345333611329, 5.243569643749999010 ) ) ;
#17517 = CARTESIAN_POINT ( 'NONE',  ( 13.92187500061451644, 4.119189519843966529, 2.378215178124999607 ) ) ;
#17518 = VERTEX_POINT ( 'NONE', #35419 ) ;
#17519 = CARTESIAN_POINT ( 'NONE',  ( 20.17499999999999716, -4.330127018922194537, 2.499999999999995559 ) ) ;
#17520 = CARTESIAN_POINT ( 'NONE',  ( 21.22500000000000142, 6.123233995736764310E-16, -4.999999999999998224 ) ) ;
#17521 = CARTESIAN_POINT ( 'NONE',  ( 21.04687500061451644, -3.027376345333610441, -5.243569643749999898 ) ) ;
#17522 = CARTESIAN_POINT ( 'NONE',  ( 25.79062500061451502, -3.027376345333614438, 5.243569643749998122 ) ) ;
#17523 = ORIENTED_EDGE ( 'NONE', *, *, #5583, .F. ) ;
#17524 = DIRECTION ( 'NONE',  ( 0.000000000000000000, 0.000000000000000000, -1.000000000000000000 ) ) ;
#17525 = CARTESIAN_POINT ( 'NONE',  ( 7.378125000614518036, -4.541064518000419881, 2.621784821874995952 ) ) ;
#17526 = CARTESIAN_POINT ( 'NONE',  ( 65.00000000000000000, -7.332543590861048344, 5.218601775200187198 ) ) ;
#17527 = CARTESIAN_POINT ( 'NONE',  ( 14.10000000000000142, 4.330127018922192761, -2.499999999999997780 ) ) ;
#17528 = CARTESIAN_POINT ( 'NONE',  ( 4.243569643749999898, 16.87812500061451715, 30.00000000000000000 ) ) ;
#17529 = CARTESIAN_POINT ( 'NONE',  ( 29.54062500061451502, -3.027376345333610441, -5.243569643749999898 ) ) ;
#17530 = CARTESIAN_POINT ( 'NONE',  ( 26.25937500061451857, 0.000000000000000000, 5.243569643749999010 ) ) ;
#17531 = VERTEX_POINT ( 'NONE', #58303 ) ;
#17532 = CARTESIAN_POINT ( 'NONE',  ( 25.04062500061451502, -3.027376345333610441, -5.243569643749999898 ) ) ;
#17533 = CARTESIAN_POINT ( 'NONE',  ( 24.87187500061451573, 3.027376345333611329, 5.243569643749999010 ) ) ;
#17534 = CARTESIAN_POINT ( 'NONE',  ( 2.121784821874999061, 17.85312500061459318, -33.67503911421598417 ) ) ;
#17535 = CARTESIAN_POINT ( 'NONE',  ( 11.32500000000000107, 6.123233995736764310E-16, -4.999999999999998224 ) ) ;
#17536 = CARTESIAN_POINT ( 'NONE',  ( 9.815625000614518925, 3.027376345333613106, -5.243569643749998122 ) ) ;
#17537 = CARTESIAN_POINT ( 'NONE',  ( 27.94687500061451502, 5.492252693125287522, 3.363034840372157021E-16 ) ) ;
#17538 = CARTESIAN_POINT ( 'NONE',  ( 28.79062500061451502, 6.054752690667223547, 3.707466751127219781E-16 ) ) ;
#17539 = CARTESIAN_POINT ( 'NONE',  ( 26.76562500061451644, -6.054752690667223547, -1.112240025338166033E-15 ) ) ;
#17540 = CARTESIAN_POINT ( 'NONE',  ( 22.40625000122903288, 0.000000000000000000, 4.999999999999998224 ) ) ;
#17541 = CARTESIAN_POINT ( 'NONE',  ( 11.63437500061451857, 5.824947211148865298E-16, -4.756430356249998326 ) ) ;
#17542 = CARTESIAN_POINT ( 'NONE',  ( 20.03437500061451715, -4.541064518000419881, 2.621784821874995952 ) ) ;
#17543 = CARTESIAN_POINT ( 'NONE',  ( -3.000416591977282496E-16, 15.69687500061451857, 25.09994784771203058 ) ) ;
#17544 = EDGE_CURVE ( 'NONE', #28339, #45340, #23400, .T. ) ;
#17545 = CARTESIAN_POINT ( 'NONE',  ( 18.15937500061451715, 0.000000000000000000, 5.243569643749999010 ) ) ;
#17546 = CARTESIAN_POINT ( 'NONE',  ( 27.38437500061451857, 6.421520780324663323E-16, -5.243569643749999010 ) ) ;
#17547 = CARTESIAN_POINT ( 'NONE',  ( 9.001249775931846008E-16, 16.37187500061451573, 34.90005215228797653 ) ) ;
#17548 = CARTESIAN_POINT ( 'NONE',  ( 9.665625000614515017, -6.054752690667223547, -1.112240025338166033E-15 ) ) ;
#17549 = CARTESIAN_POINT ( 'NONE',  ( 4.907911205059083602E-16, 5.000000000000000000, 33.99999999999999289 ) ) ;
#17550 = CARTESIAN_POINT ( 'NONE',  ( 5.371875000614516615, 3.027376345333613106, -5.243569643749998122 ) ) ;
#17551 = FACE_OUTER_BOUND ( 'NONE', #26812, .T. ) ;
#17552 = CARTESIAN_POINT ( 'NONE',  ( 8.540625000614518569, 6.054752690667223547, 3.707466751127219781E-16 ) ) ;
#17553 = CARTESIAN_POINT ( 'NONE',  ( 11.78437500061451892, 4.541064518000418104, 2.621784821874999949 ) ) ;
#17554 = CARTESIAN_POINT ( 'NONE',  ( 18.82500000122903216, 2.886751345948126879, 4.999999999999999112 ) ) ;
#17555 = CARTESIAN_POINT ( 'NONE',  ( 6.271875000614517859, 3.027376345333613106, -5.243569643749998122 ) ) ;
#17556 = CARTESIAN_POINT ( 'NONE',  ( 6.703125000614516438, 4.541064518000418104, -2.621784821874998173 ) ) ;
#17557 = CARTESIAN_POINT ( 'NONE',  ( 5.090625000614516615, -3.027376345333614438, 5.243569643749998122 ) ) ;
#17558 = CARTESIAN_POINT ( 'NONE',  ( 24.31875000122902719, -5.773502691896255534, -1.060575238724906372E-15 ) ) ;
#17559 = CARTESIAN_POINT ( 'NONE',  ( 19.50937500061451857, 0.000000000000000000, 5.243569643749999010 ) ) ;
#17560 = CARTESIAN_POINT ( 'NONE',  ( 2.000000000000001332, 13.06250000122903465, 33.46410161513774995 ) ) ;
#17561 = ORIENTED_EDGE ( 'NONE', *, *, #65041, .F. ) ;
#17562 = CARTESIAN_POINT ( 'NONE',  ( 23.57812500061451289, -4.541064518000419881, 2.621784821874995952 ) ) ;
#17563 = CARTESIAN_POINT ( 'NONE',  ( 12.17812500061451608, 4.541064518000418104, 2.621784821874999949 ) ) ;
#17564 = CARTESIAN_POINT ( 'NONE',  ( 27.08437500061451786, 4.541064518000418104, 2.621784821874999949 ) ) ;
#17565 = CARTESIAN_POINT ( 'NONE',  ( 10.45312500061451644, 0.000000000000000000, 5.243569643749999010 ) ) ;
#17566 = CARTESIAN_POINT ( 'NONE',  ( -1.473772837211104303, 9.872922166578582903, -34.04916900799978663 ) ) ;
#17567 = CARTESIAN_POINT ( 'NONE',  ( 12.11250000122903181, 0.000000000000000000, 4.999999999999998224 ) ) ;
#17568 = CARTESIAN_POINT ( 'NONE',  ( 27.81562500061452070, 3.027376345333613106, -5.243569643749998122 ) ) ;
#17569 = CARTESIAN_POINT ( 'NONE',  ( 2.121784821874999061, 12.90312500061451750, -33.67503911421598417 ) ) ;
#17570 = CARTESIAN_POINT ( 'NONE',  ( 14.40000000122903323, -2.886751345948129988, 4.999999999999997335 ) ) ;
#17571 = CARTESIAN_POINT ( 'NONE',  ( 11.21250000000000036, -5.773502691896255534, -1.060575238724906372E-15 ) ) ;
#17572 = CARTESIAN_POINT ( 'NONE',  ( 20.72812500061451502, 4.541064518000418104, 2.621784821874999949 ) ) ;
#17573 = CARTESIAN_POINT ( 'NONE',  ( 8.634375000614518569, 4.541064518000418104, 2.621784821874999949 ) ) ;
#17574 = CARTESIAN_POINT ( 'NONE',  ( 7.500000001229034652, 5.773502691896255534, 3.535250795749688894E-16 ) ) ;
#17575 = CARTESIAN_POINT ( 'NONE',  ( 17.28750000122903430, 6.123233995736764310E-16, -4.999999999999998224 ) ) ;
#17576 = CARTESIAN_POINT ( 'NONE',  ( 13.56562500061451892, 3.027376345333611329, 5.243569643749999010 ) ) ;
#17577 = CARTESIAN_POINT ( 'NONE',  ( 15.40312500061451573, 0.000000000000000000, 5.243569643749999010 ) ) ;
#17578 =( BOUNDED_CURVE ( )  B_SPLINE_CURVE ( 2, ( #39288, #56977, #28556, #6381, #23362, #57701, #40364, #34811, #61802 ),
 .UNSPECIFIED., .F., .F. ) 
 B_SPLINE_CURVE_WITH_KNOTS ( ( 3, 2, 2, 2, 3 ),
 ( 0.5760869565217391353, 0.5797101449275362528, 0.5869565217391304879, 0.5942028985507246119, 0.5978260869565217295 ),
 .UNSPECIFIED. ) 
 CURVE ( )  GEOMETRIC_REPRESENTATION_ITEM ( )  RATIONAL_B_SPLINE_CURVE ( ( 0.9330127018922194093, 0.9330127018922194093, 1.000000000000000000, 0.8660254037844387076, 1.000000000000000000, 0.8660254037844387076, 1.000000000000000000, 0.9330127018922194093, 0.9330127018922194093 ) ) 
 REPRESENTATION_ITEM ( '' )  );
#17579 = CARTESIAN_POINT ( 'NONE',  ( 25.20000000122903216, -2.886751345948129988, 4.999999999999997335 ) ) ;
#17580 = CARTESIAN_POINT ( 'NONE',  ( 20.51249999999999929, 2.886751345948126879, 4.999999999999999112 ) ) ;
#17581 = CARTESIAN_POINT ( 'NONE',  ( 22.17187500061451644, 3.027376345333611329, 5.243569643749999010 ) ) ;
#17582 = CARTESIAN_POINT ( 'NONE',  ( 34.99999999999999289, 6.363961030679004871, 6.363961030678849440 ) ) ;
#17583 = EDGE_CURVE ( 'NONE', #47866, #54008, #25057, .T. ) ;
#17584 = CARTESIAN_POINT ( 'NONE',  ( 10.46250000122903323, -4.330127018922190985, -2.500000000000001332 ) ) ;
#17585 = EDGE_CURVE ( 'NONE', #58199, #68160, #8743, .T. ) ;
#17586 = CARTESIAN_POINT ( 'NONE',  ( 8.184375000614515727, 4.541064518000418104, 2.621784821874999949 ) ) ;
#17587 = CARTESIAN_POINT ( 'NONE',  ( 29.22187500061451715, 3.027376345333613106, -5.243569643749998122 ) ) ;
#17588 = CARTESIAN_POINT ( 'NONE',  ( 3.346875000614518036, -3.027376345333614438, 5.243569643749998122 ) ) ;
#17589 = CARTESIAN_POINT ( 'NONE',  ( 24.47812500061451502, -4.541064518000419881, 2.621784821874995952 ) ) ;
#17590 = CARTESIAN_POINT ( 'NONE',  ( -3.756430356250000990, 15.26562499938548356, 32.16877607737301048 ) ) ;
#17591 = CARTESIAN_POINT ( 'NONE',  ( -2.000000000000001776, 14.09374999877096535, 33.46410161513775705 ) ) ;
#17592 = CARTESIAN_POINT ( 'NONE',  ( 8.596875000614518925, 6.054752690667223547, 3.707466751127219781E-16 ) ) ;
#17593 = CARTESIAN_POINT ( 'NONE',  ( 15.82499999999999929, 6.123233995736764310E-16, -4.999999999999998224 ) ) ;
#17594 = CARTESIAN_POINT ( 'NONE',  ( 26.84062500061451573, -3.027376345333610441, -5.243569643749999898 ) ) ;
#17595 = CARTESIAN_POINT ( 'NONE',  ( 6.384375000614516793, 4.541064518000418104, 2.621784821874999949 ) ) ;
#17596 = CARTESIAN_POINT ( 'NONE',  ( -3.999999999999999112, 16.51250000122903216, -30.00000000000000000 ) ) ;
#17597 = CARTESIAN_POINT ( 'NONE',  ( 26.29687500061451644, -3.027376345333614438, 5.243569643749998122 ) ) ;
#17598 = CARTESIAN_POINT ( 'NONE',  ( -3.000416591977282496E-16, 10.24062500061459424, 25.09994784771203058 ) ) ;
#17599 = CARTESIAN_POINT ( 'NONE',  ( 18.52499999999999858, 6.123233995736764310E-16, -4.999999999999998224 ) ) ;
#17600 = VERTEX_POINT ( 'NONE', #20240 ) ;
#17601 = CARTESIAN_POINT ( 'NONE',  ( 27.59999999999999787, 4.330127018922192761, -2.499999999999997780 ) ) ;
#17602 = CARTESIAN_POINT ( 'NONE',  ( 27.64687500061452141, -3.027376345333614438, 5.243569643749998122 ) ) ;
#17603 = ORIENTED_EDGE ( 'NONE', *, *, #63887, .F. ) ;
#17604 = CARTESIAN_POINT ( 'NONE',  ( 16.56562500061451715, 3.027376345333613106, -5.243569643749998122 ) ) ;
#17605 = CARTESIAN_POINT ( 'NONE',  ( 7.640625000614517326, 6.054752690667223547, 3.707466751127219781E-16 ) ) ;
#17606 = CARTESIAN_POINT ( 'NONE',  ( 19.28437500061451715, 5.492252693125287522, 3.363034840372157021E-16 ) ) ;
#17607 = CARTESIAN_POINT ( 'NONE',  ( 3.984375000614517326, 6.421520780324663323E-16, -5.243569643749999010 ) ) ;
#17608 = CARTESIAN_POINT ( 'NONE',  ( 16.42500000122903359, 2.886751345948129099, -4.999999999999998224 ) ) ;
#17609 = CARTESIAN_POINT ( 'NONE',  ( 22.34999999999999787, 0.000000000000000000, 4.999999999999998224 ) ) ;
#17610 = CARTESIAN_POINT ( 'NONE',  ( 29.06250000000000000, 2.886751345948126879, 4.999999999999999112 ) ) ;
#17611 = CARTESIAN_POINT ( 'NONE',  ( 4.846875000614519813, -3.027376345333610441, -5.243569643749999898 ) ) ;
#17612 = CARTESIAN_POINT ( 'NONE',  ( 9.721875000614517148, -6.054752690667223547, -1.112240025338166033E-15 ) ) ;
#17613 = CARTESIAN_POINT ( 'NONE',  ( 22.20937500061451431, 0.000000000000000000, 5.243569643749999010 ) ) ;
#17614 = CARTESIAN_POINT ( 'NONE',  ( 9.528763966825557376E-15, 17.41249999999999787, -26.00000000000000000 ) ) ;
#17615 = ORIENTED_EDGE ( 'NONE', *, *, #21641, .F. ) ;
#17616 = CARTESIAN_POINT ( 'NONE',  ( 3.196875000614516793, 6.054752690667223547, 3.707466751127219781E-16 ) ) ;
#17617 = CARTESIAN_POINT ( 'NONE',  ( 6.984375000614516438, -4.541064518000419881, 2.621784821874995952 ) ) ;
#17618 = CARTESIAN_POINT ( 'NONE',  ( 17.66249999999999787, 2.886751345948129099, -4.999999999999998224 ) ) ;
#17619 = CARTESIAN_POINT ( 'NONE',  ( 17.01562500061451644, 3.027376345333613106, -5.243569643749998122 ) ) ;
#17620 = CARTESIAN_POINT ( 'NONE',  ( -2.000000000000001776, 18.64999999999999858, 33.46410161513775705 ) ) ;
#17621 = CARTESIAN_POINT ( 'NONE',  ( 45.00000000000000000, 0.000000000000000000, 4.999999999999998224 ) ) ;
#17622 = EDGE_CURVE ( 'NONE', #18316, #54892, #56420, .T. ) ;
#17623 = CARTESIAN_POINT ( 'NONE',  ( 20.03437500061451715, -4.119189519843968306, 2.378215178124996054 ) ) ;
#17624 = CARTESIAN_POINT ( 'NONE',  ( 9.365625000614519635, 3.027376345333613106, -5.243569643749998122 ) ) ;
#17625 = CARTESIAN_POINT ( 'NONE',  ( 27.42187500061451644, 3.027376345333613106, -5.243569643749998122 ) ) ;
#17626 = CARTESIAN_POINT ( 'NONE',  ( 27.49687500061451217, 6.054752690667223547, 3.707466751127219781E-16 ) ) ;
#17627 = CARTESIAN_POINT ( 'NONE',  ( 7.500000000000000000, 0.000000000000000000, 4.999999999999998224 ) ) ;
#17628 = CARTESIAN_POINT ( 'NONE',  ( -2.000000000000000000, 14.18750000122903288, 26.53589838486224650 ) ) ;
#17629 = CARTESIAN_POINT ( 'NONE',  ( 8.662500001229034297, -4.330127018922190985, -2.500000000000001332 ) ) ;
#17630 = CARTESIAN_POINT ( 'NONE',  ( 21.12187500061451573, 3.027376345333613106, -5.243569643749998122 ) ) ;
#17631 = CARTESIAN_POINT ( 'NONE',  ( 10.69687500061451679, -3.027376345333610441, -5.243569643749999898 ) ) ;
#17632 = CARTESIAN_POINT ( 'NONE',  ( 1.071796769724490561, 13.70134618820330097, 34.00000000000000000 ) ) ;
#17633 = ORIENTED_EDGE ( 'NONE', *, *, #33344, .T. ) ;
#17634 = CARTESIAN_POINT ( 'NONE',  ( 15.62812500061451537, 6.421520780324663323E-16, -5.243569643749999010 ) ) ;
#17635 = CARTESIAN_POINT ( 'NONE',  ( 27.41250000122903430, 0.000000000000000000, 4.999999999999998224 ) ) ;
#17636 = CARTESIAN_POINT ( 'NONE',  ( 13.02187500061451608, 3.027376345333613106, -5.243569643749998122 ) ) ;
#17637 = CARTESIAN_POINT ( 'NONE',  ( 2.000000000000001332, 12.61250000122903536, 33.46410161513774995 ) ) ;
#17638 = CARTESIAN_POINT ( 'NONE',  ( 15.66562500061451857, 3.027376345333613106, -5.243569643749998122 ) ) ;
#17639 = CARTESIAN_POINT ( 'NONE',  ( 1.999999999999998668, 18.95000000000000284, -33.46410161513775705 ) ) ;
#17640 = CARTESIAN_POINT ( 'NONE',  ( 26.37187500061451217, -6.054752690667223547, -1.112240025338166033E-15 ) ) ;
#17641 = CARTESIAN_POINT ( 'NONE',  ( 2.904760919847030110, -4.069688439982819261, 3.306457108496466901 ) ) ;
#17642 = CARTESIAN_POINT ( 'NONE',  ( 12.63750000122903394, -4.330127018922194537, 2.499999999999995559 ) ) ;
#17643 = CARTESIAN_POINT ( 'NONE',  ( 7.359375000614516438, 0.000000000000000000, 4.756430356249998326 ) ) ;
#17644 = CARTESIAN_POINT ( 'NONE',  ( -4.243569643749998122, 18.09687500061451715, -27.54997392385601174 ) ) ;
#17645 = CARTESIAN_POINT ( 'NONE',  ( 18.27187500061451431, -6.054752690667223547, -1.112240025338166033E-15 ) ) ;
#17646 = CARTESIAN_POINT ( 'NONE',  ( 19.35000000122903430, -2.886751345948129988, 4.999999999999997335 ) ) ;
#17647 = CARTESIAN_POINT ( 'NONE',  ( 14.93437500061451750, 4.541064518000418104, 2.621784821874999949 ) ) ;
#17648 = CARTESIAN_POINT ( 'NONE',  ( 9.001249775931846008E-16, 19.46562500061451573, -25.09994784771203058 ) ) ;
#17649 = CARTESIAN_POINT ( 'NONE',  ( 21.45000000122903216, 5.773502691896255534, 3.535250795749688894E-16 ) ) ;
#17650 = CARTESIAN_POINT ( 'NONE',  ( 16.19062500061451715, 6.054752690667223547, 3.707466751127219781E-16 ) ) ;
#17651 = CARTESIAN_POINT ( 'NONE',  ( 28.86562500061451786, 3.027376345333611329, 5.243569643749999010 ) ) ;
#17652 = VERTEX_POINT ( 'NONE', #3642 ) ;
#17653 = VERTEX_POINT ( 'NONE', #20977 ) ;
#17654 = CARTESIAN_POINT ( 'NONE',  ( 18.07499999999999929, 6.123233995736764310E-16, -4.999999999999998224 ) ) ;
#17655 = CARTESIAN_POINT ( 'NONE',  ( 27.44999999999999929, -4.330127018922190985, -2.500000000000001332 ) ) ;
#17656 = CARTESIAN_POINT ( 'NONE',  ( 2.064291216241245230, 4.560108959200714907, 33.43572587555581066 ) ) ;
#17657 = CARTESIAN_POINT ( 'NONE',  ( 14.55000000122903181, -2.886751345948125991, -5.000000000000000000 ) ) ;
#17658 = CARTESIAN_POINT ( 'NONE',  ( 20.16562500061451146, 3.027376345333613106, -5.243569643749998122 ) ) ;
#17659 = CARTESIAN_POINT ( 'NONE',  ( 23.72812500061451502, 6.421520780324663323E-16, -5.243569643749999010 ) ) ;
#17660 = CARTESIAN_POINT ( 'NONE',  ( 4.378125000614518925, 6.421520780324663323E-16, -5.243569643749999010 ) ) ;
#17661 = CARTESIAN_POINT ( 'NONE',  ( -4.000000000000000000, 20.31874999877096499, 30.00000000000000000 ) ) ;
#17662 = CARTESIAN_POINT ( 'NONE',  ( -5.810221930991193690E-16, 11.90000000122903501, 26.00000000000000355 ) ) ;
#17663 = CARTESIAN_POINT ( 'NONE',  ( 9.909375000614517148, 4.119189519843966529, -2.378215178124998275 ) ) ;
#17664 = CARTESIAN_POINT ( 'NONE',  ( 29.48437500061451644, -4.541064518000419881, 2.621784821874995952 ) ) ;
#17665 = CARTESIAN_POINT ( 'NONE',  ( -3.999999999999999112, 10.21250000122903501, -30.00000000000000000 ) ) ;
#17666 = CARTESIAN_POINT ( 'NONE',  ( -3.000416591977282496E-16, 15.69687500061451857, -34.90005215228797653 ) ) ;
#17667 = CARTESIAN_POINT ( 'NONE',  ( 5.737500001229033586, 4.330127018922191873, 2.499999999999999556 ) ) ;
#17668 = CARTESIAN_POINT ( 'NONE',  ( 7.724999999999999645, 6.123233995736764310E-16, -4.999999999999998224 ) ) ;
#17669 = ADVANCED_FACE ( 'NONE', ( #71228 ), #43530, .F. ) ;
#17670 = CARTESIAN_POINT ( 'NONE',  ( 3.937500001229034208, 4.330127018922191873, 2.499999999999999556 ) ) ;
#17671 = CARTESIAN_POINT ( 'NONE',  ( 9.121875000614517504, 3.027376345333611329, 5.243569643749999010 ) ) ;
#17672 = DIRECTION ( 'NONE',  ( 0.000000000000000000, 0.000000000000000000, 1.000000000000000000 ) ) ;
#17673 = CARTESIAN_POINT ( 'NONE',  ( 3.009375000614516793, -4.541064518000417216, -2.621784821875001281 ) ) ;
#17674 = VECTOR ( 'NONE', #51140, 1000.000000000000000 ) ;
#17675 = CARTESIAN_POINT ( 'NONE',  ( -1.394453263437886604E-15, 19.32500000122903216, 33.99999999999999289 ) ) ;
#17676 = CARTESIAN_POINT ( 'NONE',  ( 6.684375000614518392, 6.421520780324663323E-16, -5.243569643749999010 ) ) ;
#17677 = CARTESIAN_POINT ( 'NONE',  ( 13.28437500061451715, -4.541064518000419881, 2.621784821874995952 ) ) ;
#17678 = FACE_OUTER_BOUND ( 'NONE', #44379, .T. ) ;
#17679 = CARTESIAN_POINT ( 'NONE',  ( 7.162500000000001421, -5.773502691896255534, -1.060575238724906372E-15 ) ) ;
#17680 = CARTESIAN_POINT ( 'NONE',  ( -4.243569643749998122, 17.59062500061459744, 32.45002607614398471 ) ) ;
#17681 = CARTESIAN_POINT ( 'NONE',  ( 22.17187500061451644, 3.027376345333611329, 5.243569643749999010 ) ) ;
#17682 = FILL_AREA_STYLE ('',( #45061 ) ) ;
#17683 = CARTESIAN_POINT ( 'NONE',  ( 26.96250000122903145, 0.000000000000000000, 4.999999999999998224 ) ) ;
#17684 = CARTESIAN_POINT ( 'NONE',  ( 16.99687500061451573, 4.119189519843966529, -2.378215178124998275 ) ) ;
#17685 = CARTESIAN_POINT ( 'NONE',  ( 22.49062500061451431, 6.054752690667223547, 3.707466751127219781E-16 ) ) ;
#17686 = CARTESIAN_POINT ( 'NONE',  ( 16.11562500061451786, 3.027376345333613106, -5.243569643749998122 ) ) ;
#17687 = CARTESIAN_POINT ( 'NONE',  ( 27.15937500061451360, -5.492252693125287522, -1.008910452111647106E-15 ) ) ;
#17688 = CARTESIAN_POINT ( 'NONE',  ( 12.75937500061451857, 0.000000000000000000, 5.243569643749999010 ) ) ;
#17689 = CARTESIAN_POINT ( 'NONE',  ( 29.36250000000000071, 2.886751345948129099, -4.999999999999998224 ) ) ;
#17690 = CARTESIAN_POINT ( 'NONE',  ( 23.96250000122903145, -4.330127018922190985, -2.500000000000001332 ) ) ;
#17691 = CARTESIAN_POINT ( 'NONE',  ( 28.68749999999999289, -2.886751345948110004, 5.000000000000031974 ) ) ;
#17692 = CARTESIAN_POINT ( 'NONE',  ( 11.70937500061451608, 4.541064518000418104, -2.621784821874998173 ) ) ;
#17693 = CARTESIAN_POINT ( 'NONE',  ( 29.29687500061451644, 6.054752690667223547, 3.707466751127219781E-16 ) ) ;
#17694 = CARTESIAN_POINT ( 'NONE',  ( 3.834375000614519635, -4.541064518000419881, 2.621784821874995952 ) ) ;
#17695 = CARTESIAN_POINT ( 'NONE',  ( 18.52499999999999858, 6.123233995736764310E-16, -4.999999999999998224 ) ) ;
#17696 = CARTESIAN_POINT ( 'NONE',  ( 23.22187500061451715, -6.054752690667223547, -1.112240025338166033E-15 ) ) ;
#17697 = CARTESIAN_POINT ( 'NONE',  ( 15.27187500061451786, 3.027376345333613106, -5.243569643749998122 ) ) ;
#17698 = CARTESIAN_POINT ( 'NONE',  ( -3.756430356250001434, 18.86562499938548498, 32.16877607737301048 ) ) ;
#17699 = CARTESIAN_POINT ( 'NONE',  ( 24.97499999999999787, 4.330127018922191873, 2.499999999999999556 ) ) ;
#17700 = CARTESIAN_POINT ( 'NONE',  ( -2.000000000000001776, 12.80000000000000071, 33.46410161513775705 ) ) ;
#17701 = CARTESIAN_POINT ( 'NONE',  ( 26.29687500061451644, -2.746126346562646425, 4.756430356249996549 ) ) ;
#17702 = CARTESIAN_POINT ( 'NONE',  ( 17.42812500061451786, 6.421520780324663323E-16, -5.243569643749999010 ) ) ;
#17703 = CARTESIAN_POINT ( 'NONE',  ( 6.075000000000000178, 4.330127018922191873, 2.499999999999999556 ) ) ;
#17704 = CARTESIAN_POINT ( 'NONE',  ( 3.999999999999999112, 13.58750000122903323, 30.00000000000000000 ) ) ;
#17705 = CARTESIAN_POINT ( 'NONE',  ( 17.10000000000000142, -4.330127018922190985, -2.500000000000001332 ) ) ;
#17706 = ADVANCED_FACE ( 'NONE', ( #59396 ), #42792, .T. ) ;
#17707 = CARTESIAN_POINT ( 'NONE',  ( -3.000416591977282496E-16, 12.49062500061451608, 25.09994784771203058 ) ) ;
#17708 = CARTESIAN_POINT ( 'NONE',  ( 14.51249999999999929, 2.886751345948073588, -5.000000000000094147 ) ) ;
#17709 = CARTESIAN_POINT ( 'NONE',  ( 27.42187500061451644, 3.027376345333613106, -5.243569643749998122 ) ) ;
#17710 = ORIENTED_EDGE ( 'NONE', *, *, #47762, .T. ) ;
#17711 = CARTESIAN_POINT ( 'NONE',  ( 22.79062500061451502, -3.027376345333610441, -5.243569643749999898 ) ) ;
#17712 = CARTESIAN_POINT ( 'NONE',  ( 21.08437500061451786, 6.421520780324663323E-16, -5.243569643749999010 ) ) ;
#17713 = CARTESIAN_POINT ( 'NONE',  ( 4.425000000000001599, -4.330127018922194537, 2.499999999999995559 ) ) ;
#17714 = CARTESIAN_POINT ( 'NONE',  ( 7.978125000614517681, 6.421520780324663323E-16, -5.243569643749999010 ) ) ;
#17715 = CARTESIAN_POINT ( 'NONE',  ( 23.99062500061451786, -3.027376345333614438, 5.243569643749998122 ) ) ;
#17716 = CARTESIAN_POINT ( 'NONE',  ( 11.52187500061451608, -6.054752690667223547, -1.112240025338166033E-15 ) ) ;
#17717 = CARTESIAN_POINT ( 'NONE',  ( 17.89687500061451431, -3.027376345333610441, -5.243569643749999898 ) ) ;
#17718 = CARTESIAN_POINT ( 'NONE',  ( -4.243569643749999898, 18.45312500061451644, 30.00000000000000000 ) ) ;
#17719 = CARTESIAN_POINT ( 'NONE',  ( 19.72500000122903074, 2.886751345948126879, 4.999999999999999112 ) ) ;
#17720 = CARTESIAN_POINT ( 'NONE',  ( 14.82187500061451502, 2.746126346562645981, -4.756430356249997438 ) ) ;
#17721 = CARTESIAN_POINT ( 'NONE',  ( 9.740625000614519635, -3.027376345333610441, -5.243569643749999898 ) ) ;
#17722 = CARTESIAN_POINT ( 'NONE',  ( 6.721875000614518925, 3.027376345333613106, -5.243569643749998122 ) ) ;
#17723 = CARTESIAN_POINT ( 'NONE',  ( 5.034375000614519813, 4.541064518000418104, 2.621784821874999949 ) ) ;
#17724 =( BOUNDED_CURVE ( )  B_SPLINE_CURVE ( 2, ( #41458, #51458, #35900, #58424, #29286, #18540, #12647 ),
 .UNSPECIFIED., .F., .F. ) 
 B_SPLINE_CURVE_WITH_KNOTS ( ( 3, 2, 2, 3 ),
 ( 0.1999999999999999556, 0.2027777777777777235, 0.2055555555555554914, 0.2083333333333332871 ),
 .UNSPECIFIED. ) 
 CURVE ( )  GEOMETRIC_REPRESENTATION_ITEM ( )  RATIONAL_B_SPLINE_CURVE ( ( 1.000000000000002665, 0.8660254037844360431, 1.000000000000000000, 0.8660254037844387076, 1.000000000000000000, 0.8660254037844413721, 0.9999999999999973355 ) ) 
 REPRESENTATION_ITEM ( '' )  );
#17725 = ORIENTED_EDGE ( 'NONE', *, *, #5848, .T. ) ;
#17726 = CARTESIAN_POINT ( 'NONE',  ( 24.23437500061451644, 6.421520780324663323E-16, -5.243569643749999010 ) ) ;
#17727 = CARTESIAN_POINT ( 'NONE',  ( 15.81562500061451537, 3.027376345333611329, 5.243569643749999010 ) ) ;
#17728 = CARTESIAN_POINT ( 'NONE',  ( 26.36250000122903003, 4.330127018922192761, -2.499999999999997780 ) ) ;
#17729 = CARTESIAN_POINT ( 'NONE',  ( 28.97812500061451502, -4.541064518000419881, 2.621784821874995952 ) ) ;
#17730 = CARTESIAN_POINT ( 'NONE',  ( 21.75937500061451502, 0.000000000000000000, 5.243569643749999010 ) ) ;
#17731 = CARTESIAN_POINT ( 'NONE',  ( 16.82812500061451644, -4.541064518000419881, 2.621784821874995952 ) ) ;
#17732 = CARTESIAN_POINT ( 'NONE',  ( -3.000416591977282496E-16, 19.74687500061451928, 25.09994784771203058 ) ) ;
#17733 = CARTESIAN_POINT ( 'NONE',  ( 22.11562500061451786, 3.027376345333611329, 5.243569643749999010 ) ) ;
#17734 = CARTESIAN_POINT ( 'NONE',  ( 29.34375000122902932, -2.886751345948115777, -5.000000000000017764 ) ) ;
#17735 = ORIENTED_EDGE ( 'NONE', *, *, #49537, .F. ) ;
#17736 = CARTESIAN_POINT ( 'NONE',  ( 26.73749999999999716, 5.773502691896255534, 3.535250795749688894E-16 ) ) ;
#17737 = CARTESIAN_POINT ( 'NONE',  ( 4.000000000000000000, 12.53749999999999964, -27.69059892324149530 ) ) ;
#17738 = CARTESIAN_POINT ( 'NONE',  ( -1.878215178125001827, 18.90312499938548285, 33.25316411605952283 ) ) ;
#17739 = CARTESIAN_POINT ( 'NONE',  ( 29.20312500061451644, 4.541064518000418104, -2.621784821874998173 ) ) ;
#17740 = CARTESIAN_POINT ( 'NONE',  ( 9.965625000614517504, 3.027376345333611329, 5.243569643749999010 ) ) ;
#17741 = CARTESIAN_POINT ( 'NONE',  ( 22.12500000122903288, -5.773502691896255534, -1.060575238724906372E-15 ) ) ;
#17742 = CARTESIAN_POINT ( 'NONE',  ( 27.14062500061451644, -3.027376345333614438, 5.243569643749998122 ) ) ;
#17743 = CARTESIAN_POINT ( 'NONE',  ( 27.59999999999999787, 4.330127018922192761, -2.499999999999997780 ) ) ;
#17744 = CARTESIAN_POINT ( 'NONE',  ( -1.999999999999997113, 17.93750000122903288, -26.53589838486224295 ) ) ;
#17745 = CARTESIAN_POINT ( 'NONE',  ( -3.999999999999997335, 12.50000000122903465, 32.30940107675850470 ) ) ;
#17746 = CARTESIAN_POINT ( 'NONE',  ( 11.12812500061451715, 6.421520780324663323E-16, -5.243569643749999010 ) ) ;
#17747 = EDGE_LOOP ( 'NONE', ( #41863, #72371, #21386, #59473 ) ) ;
#17748 = CARTESIAN_POINT ( 'NONE',  ( 8.203125000614518214, 0.000000000000000000, 5.243569643749999010 ) ) ;
#17749 = CARTESIAN_POINT ( 'NONE',  ( 4.790625000614518569, -3.027376345333610441, -5.243569643749999898 ) ) ;
#17750 = CARTESIAN_POINT ( 'NONE',  ( 16.80937500061451573, 0.000000000000000000, 4.756430356249998326 ) ) ;
#17751 = CARTESIAN_POINT ( 'NONE',  ( 0.000000000000000000, 27.50000000000000000, 30.00000000000000000 ) ) ;
#17752 = CARTESIAN_POINT ( 'NONE',  ( 14.69999999999999929, 0.000000000000000000, 4.999999999999998224 ) ) ;
#17753 = CARTESIAN_POINT ( 'NONE',  ( 15.19687500061451857, -3.027376345333610441, -5.243569643749999898 ) ) ;
#17754 = CARTESIAN_POINT ( 'NONE',  ( 10.35000000122903074, -2.886751345948129988, 4.999999999999997335 ) ) ;
#17755 = CARTESIAN_POINT ( 'NONE',  ( 19.13437500061451857, -4.541064518000419881, 2.621784821874995952 ) ) ;
#17756 = CARTESIAN_POINT ( 'NONE',  ( 18.59999999999999787, 4.330127018922192761, -2.499999999999997780 ) ) ;
#17757 = CARTESIAN_POINT ( 'NONE',  ( 21.19687500061451502, 6.054752690667223547, 3.707466751127219781E-16 ) ) ;
#17758 = CARTESIAN_POINT ( 'NONE',  ( 4.243569643749999898, 13.24062500061451786, -27.54997392385601529 ) ) ;
#17759 = CARTESIAN_POINT ( 'NONE',  ( -1.071796769724483234, 16.75759618943233420, 25.99999999999999645 ) ) ;
#17760 = CARTESIAN_POINT ( 'NONE',  ( 26.37187500061451573, 5.824947211148865298E-16, -4.756430356249998326 ) ) ;
#17761 = CARTESIAN_POINT ( 'NONE',  ( 3.999999999999998668, 15.10624999877096641, 32.30940107675850470 ) ) ;
#17762 = CARTESIAN_POINT ( 'NONE',  ( 27.96562500061451928, 3.027376345333611329, 5.243569643749999010 ) ) ;
#17763 = CARTESIAN_POINT ( 'NONE',  ( 5.287500001229035185, 4.330127018922191873, 2.499999999999999556 ) ) ;
#17764 = CARTESIAN_POINT ( 'NONE',  ( 28.05937500061451573, 0.000000000000000000, 5.243569643749999010 ) ) ;
#17765 =( BOUNDED_CURVE ( )  B_SPLINE_CURVE ( 2, ( #55430, #5182, #33254, #4100, #37337, #55792, #44718, #54696, #55066 ),
 .UNSPECIFIED., .F., .F. ) 
 B_SPLINE_CURVE_WITH_KNOTS ( ( 3, 2, 2, 2, 3 ),
 ( 0.7717391304347825942, 0.7753623188405797118, 0.7826086956521739468, 0.7898550724637680709, 0.7934782608695651884 ),
 .UNSPECIFIED. ) 
 CURVE ( )  GEOMETRIC_REPRESENTATION_ITEM ( )  RATIONAL_B_SPLINE_CURVE ( ( 0.9330127018922194093, 0.9330127018922194093, 1.000000000000000000, 0.8660254037844387076, 1.000000000000000000, 0.8660254037844387076, 1.000000000000000000, 0.9330127018922194093, 0.9330127018922194093 ) ) 
 REPRESENTATION_ITEM ( '' )  );
#17766 = CARTESIAN_POINT ( 'NONE',  ( 24.11249999999999716, 2.886751345948126879, 4.999999999999999112 ) ) ;
#17767 = CARTESIAN_POINT ( 'NONE',  ( 6.178125000614518747, 6.421520780324663323E-16, -5.243569643749999010 ) ) ;
#17768 = CARTESIAN_POINT ( 'NONE',  ( 24.60937500061451644, 2.746126346562645981, -4.756430356249997438 ) ) ;
#17769 = CARTESIAN_POINT ( 'NONE',  ( 19.92187500061451644, 3.027376345333611329, 5.243569643749999010 ) ) ;
#17770 = CARTESIAN_POINT ( 'NONE',  ( 12.38437500061451502, -2.746126346562641984, -4.756430356249999214 ) ) ;
#17771 = CARTESIAN_POINT ( 'NONE',  ( 4.715625000614516615, -6.054752690667223547, -1.112240025338166033E-15 ) ) ;
#17772 = CARTESIAN_POINT ( 'NONE',  ( 11.03437500061451715, -4.541064518000419881, 2.621784821874995952 ) ) ;
#17773 = ORIENTED_EDGE ( 'NONE', *, *, #11270, .F. ) ;
#17774 = CARTESIAN_POINT ( 'NONE',  ( 19.20937500061451786, -4.541064518000417216, -2.621784821875001281 ) ) ;
#17775 = LINE ( 'NONE', #28521, #48919 ) ;
#17776 = CARTESIAN_POINT ( 'NONE',  ( 28.46249999999999858, 2.886751345948129099, -4.999999999999998224 ) ) ;
#17777 = CARTESIAN_POINT ( 'NONE',  ( 3.637500000000001954, -2.886751345948125991, -5.000000000000000000 ) ) ;
#17778 = DIRECTION ( 'NONE',  ( 1.000000000000000000, -0.000000000000000000, -0.000000000000000000 ) ) ;
#17779 = CARTESIAN_POINT ( 'NONE',  ( 27.93750000000000355, -2.886751345948109559, -5.000000000000028422 ) ) ;
#17780 = EDGE_LOOP ( 'NONE', ( #11002, #46327, #45545, #71962 ) ) ;
#17781 = CARTESIAN_POINT ( 'NONE',  ( 9.937500000000001776, -2.886751345948125991, -5.000000000000000000 ) ) ;
#17782 = CARTESIAN_POINT ( 'NONE',  ( 11.18437500061451573, 5.492252693125287522, 3.363034840372157021E-16 ) ) ;
#17783 = CARTESIAN_POINT ( 'NONE',  ( 25.37812500061451715, -4.541064518000419881, 2.621784821874995952 ) ) ;
#17784 = CARTESIAN_POINT ( 'NONE',  ( 14.43750000000000000, -2.886751345948125991, -5.000000000000000000 ) ) ;
#17785 = CARTESIAN_POINT ( 'NONE',  ( 11.73750000122903181, -4.330127018922194537, 2.499999999999995559 ) ) ;
#17786 = CARTESIAN_POINT ( 'NONE',  ( 8.765625000614518214, -6.054752690667223547, -1.112240025338166033E-15 ) ) ;
#17787 = CARTESIAN_POINT ( 'NONE',  ( 23.28750000000000142, -2.886751345948129988, 4.999999999999997335 ) ) ;
#17788 = EDGE_CURVE ( 'NONE', #1656, #34631, #65313, .T. ) ;
#17789 = CARTESIAN_POINT ( 'NONE',  ( 21.44062500061452070, -3.027376345333610441, -5.243569643749999898 ) ) ;
#17790 = CARTESIAN_POINT ( 'NONE',  ( 5.362500001229033586, 0.000000000000000000, 4.999999999999998224 ) ) ;
#17791 = CARTESIAN_POINT ( 'NONE',  ( 28.91250000122903074, -4.330127018922190985, -2.500000000000001332 ) ) ;
#17792 = CARTESIAN_POINT ( 'NONE',  ( -3.756430356249999214, 16.87812499938548427, 27.83122392262697176 ) ) ;
#17793 = CARTESIAN_POINT ( 'NONE',  ( 6.937499999999999112, 5.773502691896255534, 3.535250795749688894E-16 ) ) ;
#17794 = VERTEX_POINT ( 'NONE', #59034 ) ;
#17795 = CARTESIAN_POINT ( 'NONE',  ( 21.14062500061451289, 6.054752690667223547, 3.707466751127219781E-16 ) ) ;
#17796 = CARTESIAN_POINT ( 'NONE',  ( 28.15312500061451573, -4.541064518000417216, -2.621784821875001281 ) ) ;
#17797 = CARTESIAN_POINT ( 'NONE',  ( 28.98750000122903359, 6.123233995736764310E-16, -4.999999999999998224 ) ) ;
#17798 = CARTESIAN_POINT ( 'NONE',  ( 19.50937500061451857, 0.000000000000000000, 5.243569643749999010 ) ) ;
#17799 = CARTESIAN_POINT ( 'NONE',  ( 13.41562500061451502, 3.027376345333613106, -5.243569643749998122 ) ) ;
#17800 = CARTESIAN_POINT ( 'NONE',  ( 11.51249999999999929, 2.886751345948182834, 4.999999999999902300 ) ) ;
#17801 = CARTESIAN_POINT ( 'NONE',  ( 29.47500000122903430, 2.886751345948129099, -4.999999999999998224 ) ) ;
#17802 = CARTESIAN_POINT ( 'NONE',  ( 21.30937500061451573, 0.000000000000000000, 4.756430356249998326 ) ) ;
#17803 = CARTESIAN_POINT ( 'NONE',  ( 16.15312500061451573, 4.541064518000418104, -2.621784821874998173 ) ) ;
#17804 = DIRECTION ( 'NONE',  ( -1.000000000000000000, -0.000000000000000000, -0.000000000000000000 ) ) ;
#17805 = CARTESIAN_POINT ( 'NONE',  ( 3.487500001229035362, 4.330127018922191873, 2.499999999999999556 ) ) ;
#17806 = CARTESIAN_POINT ( 'NONE',  ( 13.65937500061451715, 0.000000000000000000, 5.243569643749999010 ) ) ;
#17807 = CARTESIAN_POINT ( 'NONE',  ( 12.60937500061451821, 4.541064518000418104, -2.621784821874998173 ) ) ;
#17808 = CARTESIAN_POINT ( 'NONE',  ( 20.07187500061451857, -6.054752690667223547, -1.112240025338166033E-15 ) ) ;
#17809 = ORIENTED_EDGE ( 'NONE', *, *, #71833, .T. ) ;
#17810 = CARTESIAN_POINT ( 'NONE',  ( -5.840105773466367722, 8.117609419225253475, 31.39035167484127697 ) ) ;
#17811 = CARTESIAN_POINT ( 'NONE',  ( 24.40312500061451573, 0.000000000000000000, 5.243569643749999010 ) ) ;
#17812 = CARTESIAN_POINT ( 'NONE',  ( 17.74687500061451928, -3.027376345333614438, 5.243569643749998122 ) ) ;
#17813 = CARTESIAN_POINT ( 'NONE',  ( 25.26562500061451289, 3.027376345333611329, 5.243569643749999010 ) ) ;
#17814 = LINE ( 'NONE', #45920, #19079 ) ;
#17815 = CARTESIAN_POINT ( 'NONE',  ( 8.484601909799253346E-16, 15.61250000000000249, 34.61880215351700230 ) ) ;
#17816 = CARTESIAN_POINT ( 'NONE',  ( 28.45312500061451289, 0.000000000000000000, 5.243569643749999010 ) ) ;
#17817 = CARTESIAN_POINT ( 'NONE',  ( 8.737500001229033586, 6.123233995736764310E-16, -4.999999999999998224 ) ) ;
#17818 = CARTESIAN_POINT ( 'NONE',  ( 5.925000001229033586, -5.773502691896255534, -1.060575238724906372E-15 ) ) ;
#17819 = CARTESIAN_POINT ( 'NONE',  ( 28.53749999999999787, 5.773502691896255534, 3.535250795749688401E-16 ) ) ;
#17820 = CARTESIAN_POINT ( 'NONE',  ( 27.30000000122903359, 5.773502691896255534, 3.535250795749688894E-16 ) ) ;
#17821 = CARTESIAN_POINT ( 'NONE',  ( -2.000000000000001776, 19.49374999877096570, 33.46410161513775705 ) ) ;
#17822 = CARTESIAN_POINT ( 'NONE',  ( 16.03125000122903288, 4.330127018922191873, 2.499999999999999556 ) ) ;
#17823 = CARTESIAN_POINT ( 'NONE',  ( 9.909375000614517148, 4.541064518000418104, -2.621784821874998173 ) ) ;
#17824 = DIRECTION ( 'NONE',  ( -1.000000000000000000, -0.000000000000000000, -0.000000000000000000 ) ) ;
#17825 = CARTESIAN_POINT ( 'NONE',  ( 18.02812500061451573, 4.541064518000418104, 2.621784821874999949 ) ) ;
#17826 = CARTESIAN_POINT ( 'NONE',  ( 10.88437500061451679, 4.541064518000418104, 2.621784821874999949 ) ) ;
#17827 = CARTESIAN_POINT ( 'NONE',  ( 29.62500000122903288, 2.886751345948126879, 4.999999999999999112 ) ) ;
#17828 = CARTESIAN_POINT ( 'NONE',  ( 20.89687500061451786, -3.027376345333614438, 5.243569643749998122 ) ) ;
#17829 = CARTESIAN_POINT ( 'NONE',  ( 6.271875000614517859, 3.027376345333613106, -5.243569643749998122 ) ) ;
#17830 = CARTESIAN_POINT ( 'NONE',  ( 3.160880256176461511, -3.874123901750303300, -3.160880256176591185 ) ) ;
#17831 = CARTESIAN_POINT ( 'NONE',  ( 4.000000000000000000, 16.10000000000000142, 30.00000000000000000 ) ) ;
#17832 = CARTESIAN_POINT ( 'NONE',  ( 8.315625000614515372, -6.054752690667223547, -1.112240025338166033E-15 ) ) ;
#17833 = CARTESIAN_POINT ( 'NONE',  ( 21.17812500061451431, 4.541064518000418104, 2.621784821874999949 ) ) ;
#17834 = ORIENTED_EDGE ( 'NONE', *, *, #9426, .T. ) ;
#17835 = CARTESIAN_POINT ( 'NONE',  ( 5.850000001229035185, -2.886751345948129988, 4.999999999999997335 ) ) ;
#17836 = CARTESIAN_POINT ( 'NONE',  ( 14.72812500061451679, 6.421520780324663323E-16, -5.243569643749999010 ) ) ;
#17837 = CARTESIAN_POINT ( 'NONE',  ( 13.04062500061451502, 6.054752690667223547, 3.707466751127219781E-16 ) ) ;
#17838 = CARTESIAN_POINT ( 'NONE',  ( 23.37187500061451573, 2.746126346562645981, -4.756430356249997438 ) ) ;
#17839 = CARTESIAN_POINT ( 'NONE',  ( 12.18750000000000000, -2.886751345948125991, -5.000000000000000000 ) ) ;
#17840 = CARTESIAN_POINT ( 'NONE',  ( 8.925000001229033586, 2.886751345948126879, 4.999999999999999112 ) ) ;
#17841 = CARTESIAN_POINT ( 'NONE',  ( 5.915625000614515905, 3.027376345333611329, 5.243569643749999010 ) ) ;
#17842 = ADVANCED_FACE ( 'NONE', ( #47973 ), #60131, .F. ) ;
#17843 = CARTESIAN_POINT ( 'NONE',  ( 17.96250000122903501, 0.000000000000000000, 4.999999999999998224 ) ) ;
#17844 = CARTESIAN_POINT ( 'NONE',  ( 23.51249999999999574, 2.886751345948129099, -4.999999999999998224 ) ) ;
#17845 = EDGE_CURVE ( 'NONE', #54880, #36109, #44143, .T. ) ;
#17846 = CARTESIAN_POINT ( 'NONE',  ( -2.121784821874996840, 10.93437500061451928, -26.32496088578401583 ) ) ;
#17847 = FACE_OUTER_BOUND ( 'NONE', #39264, .T. ) ;
#17848 = CARTESIAN_POINT ( 'NONE',  ( 4.125000001229034652, -5.773502691896255534, -1.060575238724906372E-15 ) ) ;
#17849 = CARTESIAN_POINT ( 'NONE',  ( 28.50000000122903643, -2.886751345948155745, -4.999999999999948486 ) ) ;
#17850 = FACE_OUTER_BOUND ( 'NONE', #7257, .T. ) ;
#17851 = CARTESIAN_POINT ( 'NONE',  ( 18.12187500061451573, 3.027376345333611329, 5.243569643749999010 ) ) ;
#17852 = COLOUR_RGB ( '',0.8941176470588234615, 0.8941176470588234615, 0.8941176470588234615 ) ;
#17853 = EDGE_CURVE ( 'NONE', #24521, #12847, #63953, .T. ) ;
#17854 = CARTESIAN_POINT ( 'NONE',  ( 30.00000000000000000, 0.000000000000000000, 0.000000000000000000 ) ) ;
#17855 = CARTESIAN_POINT ( 'NONE',  ( 12.89062500061451821, -3.027376345333610441, -5.243569643749999898 ) ) ;
#17856 = CARTESIAN_POINT ( 'NONE',  ( 8.718750001229032875, 2.886751345948129099, -4.999999999999998224 ) ) ;
#17857 = CARTESIAN_POINT ( 'NONE',  ( 0.000000000000000000, 20.00000000000000000, 30.00000000000000000 ) ) ;
#17858 = CARTESIAN_POINT ( 'NONE',  ( 28.80937500061451573, 4.541064518000418104, -2.621784821874998173 ) ) ;
#17859 = CARTESIAN_POINT ( 'NONE',  ( 26.10937500061451644, 4.541064518000418104, -2.621784821874998173 ) ) ;
#17860 = CARTESIAN_POINT ( 'NONE',  ( 19.05937500061451573, -5.492252693125287522, -1.008910452111647106E-15 ) ) ;
#17861 = CARTESIAN_POINT ( 'NONE',  ( 13.19062500061451537, -3.027376345333614438, 5.243569643749998122 ) ) ;
#17862 = CARTESIAN_POINT ( 'NONE',  ( 9.834375000614517859, 6.421520780324663323E-16, -5.243569643749999010 ) ) ;
#17863 = ORIENTED_EDGE ( 'NONE', *, *, #50844, .T. ) ;
#17864 = CARTESIAN_POINT ( 'NONE',  ( 2.896627646276317858, -4.075481355475408130, -3.116761479535832713 ) ) ;
#17865 = CARTESIAN_POINT ( 'NONE',  ( 20.91562500061451502, -6.054752690667223547, -1.112240025338166033E-15 ) ) ;
#17866 = DIRECTION ( 'NONE',  ( -1.000000000000000000, -0.000000000000000000, -0.000000000000000000 ) ) ;
#17867 = EDGE_CURVE ( 'NONE', #57346, #55447, #50856, .T. ) ;
#17868 = CARTESIAN_POINT ( 'NONE',  ( 9.299999999999998934, 0.000000000000000000, 4.999999999999998224 ) ) ;
#17869 = CARTESIAN_POINT ( 'NONE',  ( 22.91250000122903430, 0.000000000000000000, 4.999999999999998224 ) ) ;
#17870 = CARTESIAN_POINT ( 'NONE',  ( 17.09062500061451573, 6.054752690667223547, 3.707466751127219781E-16 ) ) ;
#17871 = CARTESIAN_POINT ( 'NONE',  ( 10.99687500061451573, -4.119189519843965641, -2.378215178125001383 ) ) ;
#17872 = ORIENTED_EDGE ( 'NONE', *, *, #68046, .F. ) ;
#17873 = CARTESIAN_POINT ( 'NONE',  ( 17.66249999999999787, 2.886751345948129099, -4.999999999999998224 ) ) ;
#17874 = CARTESIAN_POINT ( 'NONE',  ( 20.85000000000000142, 4.330127018922192761, -2.499999999999997780 ) ) ;
#17875 = CARTESIAN_POINT ( 'NONE',  ( 18.75937500061451857, -4.541064518000417216, -2.621784821875001281 ) ) ;
#17876 = CARTESIAN_POINT ( 'NONE',  ( 25.07812500061451644, 6.421520780324663323E-16, -5.243569643749999010 ) ) ;
#17877 = ORIENTED_EDGE ( 'NONE', *, *, #72232, .F. ) ;
#17878 = CARTESIAN_POINT ( 'NONE',  ( 9.528763966825557376E-15, 17.07500000122903572, 34.00000000000000000 ) ) ;
#17879 = CARTESIAN_POINT ( 'NONE',  ( 7.115625000614516082, 3.027376345333613106, -5.243569643749998122 ) ) ;
#17880 = CARTESIAN_POINT ( 'NONE',  ( 3.999999999999998668, 15.42500000122903359, 27.69059892324149530 ) ) ;
#17881 = CARTESIAN_POINT ( 'NONE',  ( 15.41250000000000142, 2.886751345948129099, -4.999999999999998224 ) ) ;
#17882 = CARTESIAN_POINT ( 'NONE',  ( -4.243569643749997233, 18.49062500061451431, 32.45002607614398471 ) ) ;
#17883 = CARTESIAN_POINT ( 'NONE',  ( 27.92812500061451431, 4.541064518000418104, 2.621784821874999949 ) ) ;
#17884 = CARTESIAN_POINT ( 'NONE',  ( 11.66249999999999964, -5.773502691896255534, -1.060575238724906372E-15 ) ) ;
#17885 = CARTESIAN_POINT ( 'NONE',  ( 3.756430356249998770, 15.30312499938548498, 32.16877607737302469 ) ) ;
#17886 = CARTESIAN_POINT ( 'NONE',  ( 25.62187500061451573, 3.027376345333613106, -5.243569643749998122 ) ) ;
#17887 = EDGE_LOOP ( 'NONE', ( #62637, #44690, #48899, #5718 ) ) ;
#17888 = CARTESIAN_POINT ( 'NONE',  ( 23.76562500061451644, 3.027376345333613106, -5.243569643749998122 ) ) ;
#17889 = CARTESIAN_POINT ( 'NONE',  ( 25.84687500061451360, -3.027376345333614438, 5.243569643749998122 ) ) ;
#17890 = CARTESIAN_POINT ( 'NONE',  ( 4.243569643749999898, 17.32812500061459460, -30.00000000000000000 ) ) ;
#17891 = CARTESIAN_POINT ( 'NONE',  ( 11.70000000000000284, -4.330127018922190985, -2.500000000000001332 ) ) ;
#17892 = CARTESIAN_POINT ( 'NONE',  ( 8.315625000614515372, -6.054752690667223547, -1.112240025338166033E-15 ) ) ;
#17893 = CARTESIAN_POINT ( 'NONE',  ( 28.20937500061451786, -4.119189519843965641, -2.378215178125001383 ) ) ;
#17894 = CARTESIAN_POINT ( 'NONE',  ( 28.26562500061451289, 3.027376345333613106, -5.243569643749998122 ) ) ;
#17895 = CARTESIAN_POINT ( 'NONE',  ( 26.31562500061451715, -6.054752690667223547, -1.112240025338166033E-15 ) ) ;
#17896 = CARTESIAN_POINT ( 'NONE',  ( 28.43437500061451573, -2.746126346562646425, 4.756430356249996549 ) ) ;
#17897 = CARTESIAN_POINT ( 'NONE',  ( 12.90937500061451537, -4.119189519843965641, -2.378215178125001383 ) ) ;
#17898 = CARTESIAN_POINT ( 'NONE',  ( 19.65937500061451360, -4.541064518000417216, -2.621784821875001281 ) ) ;
#17899 = CARTESIAN_POINT ( 'NONE',  ( 4.243569643749999898, 12.43437500061451750, 30.00000000000000000 ) ) ;
#17900 = CARTESIAN_POINT ( 'NONE',  ( 19.88437500061451857, 4.541064518000418104, 2.621784821874999949 ) ) ;
#17901 = CARTESIAN_POINT ( 'NONE',  ( 26.70937500061451431, 0.000000000000000000, 5.243569643749999010 ) ) ;
#17902 = CARTESIAN_POINT ( 'NONE',  ( -2.121784821874996840, 16.78437500061452070, 33.67503911421598417 ) ) ;
#17903 = CARTESIAN_POINT ( 'NONE',  ( 7.640625000614517326, 6.054752690667223547, 3.707466751127219781E-16 ) ) ;
#17904 = CARTESIAN_POINT ( 'NONE',  ( 4.059375000614519280, 4.541064518000418104, -2.621784821874998173 ) ) ;
#17905 = CYLINDRICAL_SURFACE ( 'NONE', #46620, 4.999999999999998224 ) ;
#17906 = CARTESIAN_POINT ( 'NONE',  ( 4.265625000614517326, -6.054752690667223547, -1.112240025338166033E-15 ) ) ;
#17907 = CARTESIAN_POINT ( 'NONE',  ( 10.65937500061451715, -4.541064518000417216, -2.621784821875001281 ) ) ;
#17908 = CARTESIAN_POINT ( 'NONE',  ( 19.91250000122903074, -4.330127018922190985, -2.500000000000001332 ) ) ;
#17909 = CARTESIAN_POINT ( 'NONE',  ( 5.559375000614517504, 0.000000000000000000, 5.243569643749999010 ) ) ;
#17910 = CARTESIAN_POINT ( 'NONE',  ( 6.628125000614517148, 6.421520780324663323E-16, -5.243569643749999010 ) ) ;
#17911 = CARTESIAN_POINT ( 'NONE',  ( 5.315625000614516260, 3.027376345333612662, -5.243569643749998122 ) ) ;
#17912 = CARTESIAN_POINT ( 'NONE',  ( 24.39375000122903003, -2.886751345948125991, -5.000000000000000000 ) ) ;
#17913 = CARTESIAN_POINT ( 'NONE',  ( 17.44687500061451857, -3.027376345333610441, -5.243569643749999898 ) ) ;
#17914 = CARTESIAN_POINT ( 'NONE',  ( 2.000000000000000444, 19.26874999877096784, 26.53589838486224650 ) ) ;
#17915 = ORIENTED_EDGE ( 'NONE', *, *, #49500, .F. ) ;
#17916 = CARTESIAN_POINT ( 'NONE',  ( 24.10312500061451502, -4.541064518000417216, -2.621784821875001281 ) ) ;
#17917 = CARTESIAN_POINT ( 'NONE',  ( 9.328125000614518214, 6.421520780324663323E-16, -5.243569643749999010 ) ) ;
#17918 = CARTESIAN_POINT ( 'NONE',  ( 27.42187500061451644, 3.027376345333612662, -5.243569643749998122 ) ) ;
#17919 = CARTESIAN_POINT ( 'NONE',  ( 9.553125000614517859, 0.000000000000000000, 5.243569643749999010 ) ) ;
#17920 = CARTESIAN_POINT ( 'NONE',  ( -2.121784821874996840, 10.48437500061451821, -26.32496088578401583 ) ) ;
#17921 = CARTESIAN_POINT ( 'NONE',  ( 13.68750000122903288, 6.123233995736764310E-16, -4.999999999999998224 ) ) ;
#17922 = CARTESIAN_POINT ( 'NONE',  ( 26.27812500061451573, -4.541064518000419881, 2.621784821874995952 ) ) ;
#17923 = VECTOR ( 'NONE', #47022, 1000.000000000000000 ) ;
#17924 = CARTESIAN_POINT ( 'NONE',  ( 2.121784821875001281, 14.10312500061451679, -26.32496088578401938 ) ) ;
#17925 = CARTESIAN_POINT ( 'NONE',  ( 12.41250000122903430, 4.330127018922192761, -2.499999999999997780 ) ) ;
#17926 = CARTESIAN_POINT ( 'NONE',  ( 10.61250000000000071, 2.886751345948126879, 4.999999999999999112 ) ) ;
#17927 = CARTESIAN_POINT ( 'NONE',  ( 20.46562500061451928, -6.054752690667223547, -1.112240025338166033E-15 ) ) ;
#17928 = CARTESIAN_POINT ( 'NONE',  ( 4.996875000614516615, 6.054752690667223547, 3.707466751127219781E-16 ) ) ;
#17929 = CARTESIAN_POINT ( 'NONE',  ( 19.50000000000000000, 4.330127018922192761, -2.499999999999997780 ) ) ;
#17930 = CARTESIAN_POINT ( 'NONE',  ( 8.962500001229033231, 0.000000000000000000, 4.999999999999998224 ) ) ;
#17931 = CARTESIAN_POINT ( 'NONE',  ( 16.12500000122903288, 2.886751345948126879, 4.999999999999999112 ) ) ;
#17932 = CARTESIAN_POINT ( 'NONE',  ( 12.25312500061451537, 0.000000000000000000, 5.243569643749999010 ) ) ;
#17933 =( BOUNDED_CURVE ( )  B_SPLINE_CURVE ( 2, ( #35173, #17800, #6742, #47349, #40360, #58052, #41448 ),
 .UNSPECIFIED., .F., .F. ) 
 B_SPLINE_CURVE_WITH_KNOTS ( ( 3, 2, 2, 3 ),
 ( 0.8200000000000000622, 0.8233333333333334725, 0.8266666666666667718, 0.8300000000000000711 ),
 .UNSPECIFIED. ) 
 CURVE ( )  GEOMETRIC_REPRESENTATION_ITEM ( )  RATIONAL_B_SPLINE_CURVE ( ( 0.9999999999999955591, 0.8660254037844431485, 1.000000000000000000, 0.8660254037844387076, 1.000000000000000000, 0.8660254037844342667, 1.000000000000004441 ) ) 
 REPRESENTATION_ITEM ( '' )  );
#17934 = CARTESIAN_POINT ( 'NONE',  ( 15.51562500061451644, -6.054752690667223547, -1.112240025338166033E-15 ) ) ;
#17935 = CARTESIAN_POINT ( 'NONE',  ( 25.53750000122903074, 4.330127018922191873, 2.499999999999999556 ) ) ;
#17936 = CARTESIAN_POINT ( 'NONE',  ( 20.66250000000000142, -5.773502691896255534, -1.060575238724906372E-15 ) ) ;
#17937 = CARTESIAN_POINT ( 'NONE',  ( 23.52187500061451786, 3.027376345333611329, 5.243569643749999010 ) ) ;
#17938 = CARTESIAN_POINT ( 'NONE',  ( 4.898587196589411843E-16, 20.00000000000000000, -26.00000000000000000 ) ) ;
#17939 = CARTESIAN_POINT ( 'NONE',  ( 9.487500001229033586, -4.330127018922194537, 2.499999999999995559 ) ) ;
#17940 = CARTESIAN_POINT ( 'NONE',  ( 8.146875000614516082, 6.054752690667223547, 3.707466751127219781E-16 ) ) ;
#17941 = CARTESIAN_POINT ( 'NONE',  ( 25.65937500061451715, 4.541064518000418104, -2.621784821874998173 ) ) ;
#17942 = EDGE_CURVE ( 'NONE', #68198, #58357, #60495, .T. ) ;
#17943 = FACE_OUTER_BOUND ( 'NONE', #17360, .T. ) ;
#17944 = CARTESIAN_POINT ( 'NONE',  ( 22.30312500061451431, -4.541064518000417216, -2.621784821875001281 ) ) ;
#17945 = CARTESIAN_POINT ( 'NONE',  ( 27.23437500061451644, -4.541064518000419881, 2.621784821874995952 ) ) ;
#17946 = CARTESIAN_POINT ( 'NONE',  ( 3.756430356250000102, 18.15312499938548285, 30.00000000000000000 ) ) ;
#17947 = CARTESIAN_POINT ( 'NONE',  ( 3.296756130434198351, -3.759222042027491995, 3.619358968842379287 ) ) ;
#17948 = CARTESIAN_POINT ( 'NONE',  ( 6.871875000614517504, 3.027376345333611329, 5.243569643749999010 ) ) ;
#17949 = CARTESIAN_POINT ( 'NONE',  ( 18.70312500061451644, -4.541064518000417216, -2.621784821875001281 ) ) ;
#17950 = CARTESIAN_POINT ( 'NONE',  ( 4.490625000614516971, 6.054752690667223547, 3.707466751127219781E-16 ) ) ;
#17951 = CARTESIAN_POINT ( 'NONE',  ( 28.11562500061451431, -6.054752690667223547, -1.112240025338166033E-15 ) ) ;
#17952 = CARTESIAN_POINT ( 'NONE',  ( 3.796875000614517326, -3.027376345333614438, 5.243569643749998122 ) ) ;
#17953 = CARTESIAN_POINT ( 'NONE',  ( 22.91250000122903430, 0.000000000000000000, 4.999999999999998224 ) ) ;
#17954 = LINE ( 'NONE', #70031, #67950 ) ;
#17955 = CARTESIAN_POINT ( 'NONE',  ( 16.91250000000000142, 2.886751345948126879, 4.999999999999999112 ) ) ;
#17956 = ORIENTED_EDGE ( 'NONE', *, *, #25821, .F. ) ;
#17957 = CARTESIAN_POINT ( 'NONE',  ( 25.64999999999999858, -4.330127018922190985, -2.500000000000001332 ) ) ;
#17958 = CARTESIAN_POINT ( 'NONE',  ( 26.59687500061451360, 6.054752690667223547, 3.707466751127219781E-16 ) ) ;
#17959 = ORIENTED_EDGE ( 'NONE', *, *, #24471, .T. ) ;
#17960 = AXIS2_PLACEMENT_3D ( 'NONE', #33999, #44748, #5576 ) ;
#17961 = CARTESIAN_POINT ( 'NONE',  ( 14.99062500061451786, -3.027376345333614438, 5.243569643749998122 ) ) ;
#17962 = CARTESIAN_POINT ( 'NONE',  ( 6.440625000614517148, -3.027376345333614438, 5.243569643749998122 ) ) ;
#17963 = CARTESIAN_POINT ( 'NONE',  ( 19.20937500061451786, 2.746126346562645981, -4.756430356249997438 ) ) ;
#17964 = CARTESIAN_POINT ( 'NONE',  ( 4.471875000614518925, 3.027376345333613106, -5.243569643749998122 ) ) ;
#17965 = CARTESIAN_POINT ( 'NONE',  ( 15.60000000122903607, 5.773502691896255534, 3.535250795749688894E-16 ) ) ;
#17966 = CARTESIAN_POINT ( 'NONE',  ( 21.18749999999999645, -2.886751345948125991, -5.000000000000000000 ) ) ;
#17967 = CARTESIAN_POINT ( 'NONE',  ( 28.53749999999999787, 5.773502691896255534, 3.535250795749688894E-16 ) ) ;
#17968 = CARTESIAN_POINT ( 'NONE',  ( 4.584375000614516971, 4.541064518000418104, 2.621784821874999949 ) ) ;
#17969 = CARTESIAN_POINT ( 'NONE',  ( 10.24687500061451750, -3.027376345333610441, -5.243569643749999898 ) ) ;
#17970 = CARTESIAN_POINT ( 'NONE',  ( 22.58437500061451431, 4.541064518000418104, 2.621784821874999949 ) ) ;
#17971 = CARTESIAN_POINT ( 'NONE',  ( -1.626862140677534273E-15, 16.83124999877096428, 34.00000000000000000 ) ) ;
#17972 = ORIENTED_EDGE ( 'NONE', *, *, #12479, .T. ) ;
#17973 = CARTESIAN_POINT ( 'NONE',  ( 4.471875000614518925, 3.027376345333613106, -5.243569643749998122 ) ) ;
#17974 = CARTESIAN_POINT ( 'NONE',  ( 5.175000000000002487, 4.330127018922191873, 2.499999999999999556 ) ) ;
#17975 =( BOUNDED_SURFACE ( )  B_SPLINE_SURFACE ( 1, 2, ( 
 ( #59491, #25520, #38066, #19596, #4106, #59124, #48797, #25894, #36603, #43259, #21073, #14064, #3735, #71326, #20701, #15162, #26633, #66146, #42152, #65408, #49170, #15524, #65044, #37699, #60221, #8531, #53598, #60590, #2624, #9999, #2992, #14798, #8904, #9634, #37341, #70590, #19965, #42518, #47686, #31435, #54341, #48434, #43624, #32168, #9268, #14434, #36969, #53227, #53975, #70959, #20332, #59864, #31803, #26260, #70222, #27001, #374, #10727, #45440, #27725, #43991, #38439, #10364, #56515, #67259, #11087, #17346, #11455, #32895, #49531, #4827, #62418, #16617, #5908, #61329, #5553, #5187, #72055, #33259, #66891, #44364, #55797, #62061, #28442, #21799, #21434, #28091, #67973, #39905, #32534, #33615, #72788, #61688, #24, #39172, #60965, #50263, #55070, #27361, #55435, #56159, #50619, #22530, #45077, #50977, #66512, #22882, #38814, #22171, #49892, #44724, #67613, #15893, #4471, #72417, #16259, #16979, #39536, #33976, #18783, #52065, #46161, #63858, #2188, #24702, #56868, #13248, #57950, #35070, #40259, #29887, #68338, #1832, #57596, #6272, #41348, #28800, #68701, #51705, #62780, #51341, #18061, #46523, #41700, #19146, #57229, #40622, #29530, #63141, #34700, #6644, #1108, #29171, #743, #35786, #12536, #11817, #34334, #45802, #23615, #69779, #23252, #18424, #17698, #6999, #1469, #52426, #58309, #23975, #69065, #12172, #40990, #63506, #7358, #47246, #12893, #35426, #24340, #46888, #69426, #7720, #30254, #52787, #8814, #20986, #59041, #64595, #20248, #65322, #42800, #70874, #60139, #25064, #54613, #14713, #30981, #30616, #65693, #70137, #59777, #36887, #47607, #54254, #32082, #19515, #37255, #9183, #31718, #3650, #15080, #4019, #53146, #3283, #37617, #26544 ),
 ( #13613, #71613, #42073, #25811, #19886, #26173, #48349, #13982, #36521, #2545, #36158, #70510, #48714, #59406, #9548, #71236, #20616, #8445, #58676, #8086, #53514, #2908, #25439, #42439, #47982, #53892, #43174, #49085, #14352, #64961, #64224, #31351, #27278, #43539, #23441, #49811, #12357, #10643, #4389, #38350, #34891, #60877, #33173, #933, #33527, #45987, #72336, #61605, #40445, #49443, #16535, #71977, #72703, #66060, #16178, #28996, #9910, #21350, #11006, #56077, #55711, #66806, #62961, #15438, #68524, #54983, #38729, #39088, #5105, #26918, #37982, #17885, #21716, #10282, #32812, #57420, #43907, #60504, #44275, #5468, #27639, #66430, #15808, #32448, #55350, #61249, #44644, #50175, #6824, #51533, #22086, #4744, #67174, #29358, #51891, #1289, #29713, #52613, #18612, #13429, #13810, #41890, #47074, #63686, #8637, #35615, #7541, #23799, #2735, #30075, #64782, #64049, #57775, #41177, #14173, #13076, #35979, #53337, #36350, #25252, #2019, #64417, #19706, #52251, #69964, #1654, #52974, #46350, #69609, #8274, #63330, #24163, #58864, #30804, #58498, #18970, #42259, #68884, #47801, #35254, #41530, #19335, #7907, #7185, #18241, #70330, #24530, #58135, #30445, #36707, #46715, #40814, #2370, #59229, #31166, #53708, #12718, #69250, #24888, #47433, #25630, #65887, #38169, #60693, #37446, #48536, #54443, #15268, #21173, #49271, #3478, #65519, #55176, #9736, #21540, #4209, #42987, #42623, #4572, #9009, #71804, #48902, #59597, #66249, #44095, #37073, #26737, #43726, #15627, #10106, #27102, #15999, #65147, #37806, #49634, #38548, #14905, #32636, #72161, #31541, #14537, #61071, #48167, #10468, #54081, #60326, #66622, #31906, #32998, #43364, #59966, #3101, #70692, #20067, #25997 ) ),
 .UNSPECIFIED., .F., .F., .F. ) 
 B_SPLINE_SURFACE_WITH_KNOTS ( ( 2, 2 ),
 ( 3, 2, 2, 2, 2, 2, 2, 2, 2, 2, 2, 2, 2, 2, 2, 2, 2, 2, 2, 2, 2, 2, 2, 2, 2, 2, 2, 2, 2, 2, 2, 2, 2, 2, 2, 2, 2, 2, 2, 2, 2, 2, 2, 2, 2, 2, 2, 2, 2, 2, 2, 2, 2, 2, 2, 2, 2, 2, 2, 2, 2, 2, 2, 2, 2, 2, 2, 2, 2, 2, 2, 2, 2, 2, 2, 2, 2, 2, 2, 2, 2, 2, 2, 2, 2, 2, 2, 2, 2, 2, 2, 2, 2, 2, 2, 2, 2, 2, 2, 2, 2, 2, 2, 2, 2, 2, 2, 3 ),
 ( 0.000000000000000000, 1.000000000000000000 ),
 ( 0.000000000000000000, 0.009259259259259258745, 0.01851851851851851749, 0.02777777777777777624, 0.03703703703703703498, 0.04629629629629629373, 0.05555555555555555247, 0.06481481481481481122, 0.07407407407407406996, 0.08333333333333332871, 0.09259259259259258745, 0.1018518518518518462, 0.1111111111111111049, 0.1203703703703703637, 0.1296296296296296224, 0.1388888888888888951, 0.1481481481481481399, 0.1574074074074074125, 0.1666666666666666574, 0.1759259259259259300, 0.1851851851851851749, 0.1944444444444444475, 0.2037037037037036924, 0.2129629629629629650, 0.2222222222222222099, 0.2314814814814814825, 0.2407407407407407274, 0.2500000000000000000, 0.2592592592592592449, 0.2685185185185185452, 0.2777777777777777901, 0.2870370370370370350, 0.2962962962962962798, 0.3055555555555555802, 0.3148148148148148251, 0.3240740740740740700, 0.3333333333333333148, 0.3425925925925926152, 0.3518518518518518601, 0.3611111111111111049, 0.3703703703703703498, 0.3796296296296296502, 0.3888888888888888951, 0.3981481481481481399, 0.4074074074074073848, 0.4166666666666666852, 0.4259259259259259300, 0.4351851851851851749, 0.4444444444444444198, 0.4537037037037037202, 0.4629629629629629650, 0.4722222222222222099, 0.4814814814814814548, 0.4907407407407407551, 0.5000000000000000000, 0.5092592592592593004, 0.5185185185185184897, 0.5277777777777777901, 0.5370370370370370905, 0.5462962962962962798, 0.5555555555555555802, 0.5648148148148147696, 0.5740740740740740700, 0.5833333333333333703, 0.5925925925925925597, 0.6018518518518518601, 0.6111111111111111605, 0.6203703703703703498, 0.6296296296296296502, 0.6388888888888888395, 0.6481481481481481399, 0.6574074074074074403, 0.6666666666666666297, 0.6759259259259259300, 0.6851851851851852304, 0.6944444444444444198, 0.7037037037037037202, 0.7129629629629629095, 0.7222222222222222099, 0.7314814814814815103, 0.7407407407407406996, 0.7500000000000000000, 0.7592592592592593004, 0.7685185185185184897, 0.7777777777777777901, 0.7870370370370370905, 0.7962962962962962798, 0.8055555555555555802, 0.8148148148148147696, 0.8240740740740740700, 0.8333333333333333703, 0.8425925925925925597, 0.8518518518518518601, 0.8611111111111111605, 0.8703703703703703498, 0.8796296296296296502, 0.8888888888888888395, 0.8981481481481481399, 0.9074074074074074403, 0.9166666666666666297, 0.9259259259259259300, 0.9351851851851852304, 0.9444444444444444198, 0.9537037037037037202, 0.9629629629629629095, 0.9722222222222222099, 0.9814814814814815103, 0.9876227413766924812 ),
 .UNSPECIFIED. ) 
 GEOMETRIC_REPRESENTATION_ITEM ( )  RATIONAL_B_SPLINE_SURFACE ( (
 ( 1.000000000000000000, 0.8660254037844387076, 1.000000000000000000, 0.8660254037844387076, 1.000000000000000000, 0.8660254037844387076, 1.000000000000000000, 0.8660254037844387076, 1.000000000000000000, 0.8660254037844387076, 1.000000000000000000, 0.8660254037844387076, 1.000000000000000000, 0.8660254037844387076, 1.000000000000000000, 0.8660254037844387076, 1.000000000000000000, 0.8660254037844387076, 1.000000000000000000, 0.8660254037844387076, 1.000000000000000000, 0.8660254037844387076, 1.000000000000000000, 0.8660254037844387076, 1.000000000000000000, 0.8660254037844387076, 1.000000000000000000, 0.8660254037844387076, 1.000000000000000000, 0.8660254037844387076, 1.000000000000000000, 0.8660254037844387076, 1.000000000000000000, 0.8660254037844387076, 1.000000000000000000, 0.8660254037844387076, 1.000000000000000000, 0.8660254037844387076, 1.000000000000000000, 0.8660254037844387076, 1.000000000000000000, 0.8660254037844387076, 1.000000000000000000, 0.8660254037844387076, 1.000000000000000000, 0.8660254037844387076, 1.000000000000000000, 0.8660254037844387076, 1.000000000000000000, 0.8660254037844387076, 1.000000000000000000, 0.8660254037844387076, 1.000000000000000000, 0.8660254037844387076, 1.000000000000000000, 0.8660254037844387076, 1.000000000000000000, 0.8660254037844387076, 1.000000000000000000, 0.8660254037844387076, 1.000000000000000000, 0.8660254037844387076, 1.000000000000000000, 0.8660254037844387076, 1.000000000000000000, 0.8660254037844387076, 1.000000000000000000, 0.8660254037844387076, 1.000000000000000000, 0.8660254037844387076, 1.000000000000000000, 0.8660254037844387076, 1.000000000000000000, 0.8660254037844387076, 1.000000000000000000, 0.8660254037844387076, 1.000000000000000000, 0.8660254037844387076, 1.000000000000000000, 0.8660254037844387076, 1.000000000000000000, 0.8660254037844387076, 1.000000000000000000, 0.8660254037844387076, 1.000000000000000000, 0.8660254037844387076, 1.000000000000000000, 0.8660254037844387076, 1.000000000000000000, 0.8660254037844387076, 1.000000000000000000, 0.8660254037844387076, 1.000000000000000000, 0.8660254037844387076, 1.000000000000000000, 0.8660254037844387076, 1.000000000000000000, 0.8660254037844387076, 1.000000000000000000, 0.8660254037844387076, 1.000000000000000000, 0.8660254037844387076, 1.000000000000000000, 0.8660254037844387076, 1.000000000000000000, 0.8660254037844387076, 1.000000000000000000, 0.8660254037844387076, 1.000000000000000000, 0.8660254037844387076, 1.000000000000000000, 0.8660254037844387076, 1.000000000000000000, 0.8660254037844387076, 1.000000000000000000, 0.8660254037844387076, 1.000000000000000000, 0.8660254037844387076, 1.000000000000000000, 0.8660254037844387076, 1.000000000000000000, 0.8660254037844387076, 1.000000000000000000, 0.8660254037844387076, 1.000000000000000000, 0.8660254037844387076, 1.000000000000000000, 0.8660254037844387076, 1.000000000000000000, 0.8660254037844387076, 1.000000000000000000, 0.8660254037844387076, 1.000000000000000000, 0.8660254037844387076, 1.000000000000000000, 0.8660254037844387076, 1.000000000000000000, 0.8660254037844387076, 1.000000000000000000, 0.8660254037844387076, 1.000000000000000000, 0.8660254037844387076, 1.000000000000000000, 0.8660254037844387076, 1.000000000000000000, 0.8660254037844387076, 1.000000000000000000, 0.8660254037844387076, 1.000000000000000000, 0.8660254037844387076, 1.000000000000000000, 0.8660254037844387076, 1.000000000000000000, 0.8660254037844387076, 1.000000000000000000, 0.8660254037844387076, 1.000000000000000000, 0.8660254037844387076, 1.000000000000000000, 0.8660254037844387076, 1.000000000000000000, 0.8660254037844387076, 1.000000000000000000, 0.8660254037844387076, 1.000000000000000000, 0.8660254037844387076, 1.000000000000000000, 0.8660254037844387076, 1.000000000000000000, 0.8660254037844387076, 1.000000000000000000, 0.8660254037844387076, 1.000000000000000000, 0.8660254037844387076, 1.000000000000000000, 0.8660254037844387076, 1.000000000000000000, 0.8660254037844387076, 1.000000000000000000, 0.8660254037844387076, 1.000000000000000000, 0.8660254037844387076, 1.000000000000000000, 0.8660254037844387076, 1.000000000000000000, 0.8660254037844387076, 1.000000000000000000, 0.8660254037844387076, 1.000000000000000000, 0.8660254037844387076, 1.000000000000000000, 0.8660254037844387076, 1.000000000000000000, 0.8660254037844387076, 1.000000000000000000, 0.8660254037844387076, 1.000000000000000000, 0.8660254037844387076, 1.000000000000000000, 0.8660254037844387076, 1.000000000000000000, 0.8660254037844387076, 1.000000000000000000, 0.8660254037844387076, 1.000000000000000000, 0.8660254037844387076, 1.000000000000000000, 0.8660254037844387076, 1.000000000000000000, 0.8660254037844387076, 1.000000000000000000, 0.8660254037844387076, 1.000000000000000000, 0.9111405360107026619, 0.9401542295230078672),
 ( 1.000000000000000000, 0.8660254037844387076, 1.000000000000000000, 0.8660254037844387076, 1.000000000000000000, 0.8660254037844387076, 1.000000000000000000, 0.8660254037844387076, 1.000000000000000000, 0.8660254037844387076, 1.000000000000000000, 0.8660254037844387076, 1.000000000000000000, 0.8660254037844387076, 1.000000000000000000, 0.8660254037844387076, 1.000000000000000000, 0.8660254037844387076, 1.000000000000000000, 0.8660254037844387076, 1.000000000000000000, 0.8660254037844387076, 1.000000000000000000, 0.8660254037844387076, 1.000000000000000000, 0.8660254037844387076, 1.000000000000000000, 0.8660254037844387076, 1.000000000000000000, 0.8660254037844387076, 1.000000000000000000, 0.8660254037844387076, 1.000000000000000000, 0.8660254037844387076, 1.000000000000000000, 0.8660254037844387076, 1.000000000000000000, 0.8660254037844387076, 1.000000000000000000, 0.8660254037844387076, 1.000000000000000000, 0.8660254037844387076, 1.000000000000000000, 0.8660254037844387076, 1.000000000000000000, 0.8660254037844387076, 1.000000000000000000, 0.8660254037844387076, 1.000000000000000000, 0.8660254037844387076, 1.000000000000000000, 0.8660254037844387076, 1.000000000000000000, 0.8660254037844387076, 1.000000000000000000, 0.8660254037844387076, 1.000000000000000000, 0.8660254037844387076, 1.000000000000000000, 0.8660254037844387076, 1.000000000000000000, 0.8660254037844387076, 1.000000000000000000, 0.8660254037844387076, 1.000000000000000000, 0.8660254037844387076, 1.000000000000000000, 0.8660254037844387076, 1.000000000000000000, 0.8660254037844387076, 1.000000000000000000, 0.8660254037844387076, 1.000000000000000000, 0.8660254037844387076, 1.000000000000000000, 0.8660254037844387076, 1.000000000000000000, 0.8660254037844387076, 1.000000000000000000, 0.8660254037844387076, 1.000000000000000000, 0.8660254037844387076, 1.000000000000000000, 0.8660254037844387076, 1.000000000000000000, 0.8660254037844387076, 1.000000000000000000, 0.8660254037844387076, 1.000000000000000000, 0.8660254037844387076, 1.000000000000000000, 0.8660254037844387076, 1.000000000000000000, 0.8660254037844387076, 1.000000000000000000, 0.8660254037844387076, 1.000000000000000000, 0.8660254037844387076, 1.000000000000000000, 0.8660254037844387076, 1.000000000000000000, 0.8660254037844387076, 1.000000000000000000, 0.8660254037844387076, 1.000000000000000000, 0.8660254037844387076, 1.000000000000000000, 0.8660254037844387076, 1.000000000000000000, 0.8660254037844387076, 1.000000000000000000, 0.8660254037844387076, 1.000000000000000000, 0.8660254037844387076, 1.000000000000000000, 0.8660254037844387076, 1.000000000000000000, 0.8660254037844387076, 1.000000000000000000, 0.8660254037844387076, 1.000000000000000000, 0.8660254037844387076, 1.000000000000000000, 0.8660254037844387076, 1.000000000000000000, 0.8660254037844387076, 1.000000000000000000, 0.8660254037844387076, 1.000000000000000000, 0.8660254037844387076, 1.000000000000000000, 0.8660254037844387076, 1.000000000000000000, 0.8660254037844387076, 1.000000000000000000, 0.8660254037844387076, 1.000000000000000000, 0.8660254037844387076, 1.000000000000000000, 0.8660254037844387076, 1.000000000000000000, 0.8660254037844387076, 1.000000000000000000, 0.8660254037844387076, 1.000000000000000000, 0.8660254037844387076, 1.000000000000000000, 0.8660254037844387076, 1.000000000000000000, 0.8660254037844387076, 1.000000000000000000, 0.8660254037844387076, 1.000000000000000000, 0.8660254037844387076, 1.000000000000000000, 0.8660254037844387076, 1.000000000000000000, 0.8660254037844387076, 1.000000000000000000, 0.8660254037844387076, 1.000000000000000000, 0.8660254037844387076, 1.000000000000000000, 0.8660254037844387076, 1.000000000000000000, 0.8660254037844387076, 1.000000000000000000, 0.8660254037844387076, 1.000000000000000000, 0.8660254037844387076, 1.000000000000000000, 0.8660254037844387076, 1.000000000000000000, 0.8660254037844387076, 1.000000000000000000, 0.8660254037844387076, 1.000000000000000000, 0.8660254037844387076, 1.000000000000000000, 0.8660254037844387076, 1.000000000000000000, 0.8660254037844387076, 1.000000000000000000, 0.8660254037844387076, 1.000000000000000000, 0.8660254037844387076, 1.000000000000000000, 0.8660254037844387076, 1.000000000000000000, 0.8660254037844387076, 1.000000000000000000, 0.8660254037844387076, 1.000000000000000000, 0.8660254037844387076, 1.000000000000000000, 0.8660254037844387076, 1.000000000000000000, 0.8660254037844387076, 1.000000000000000000, 0.8660254037844387076, 1.000000000000000000, 0.8660254037844387076, 1.000000000000000000, 0.8660254037844387076, 1.000000000000000000, 0.8660254037844387076, 1.000000000000000000, 0.8660254037844387076, 1.000000000000000000, 0.8660254037844387076, 1.000000000000000000, 0.8660254037844387076, 1.000000000000000000, 0.9111405360107026619, 0.9401542295230078672) ) ) 
 REPRESENTATION_ITEM ( '' )  SURFACE ( )  );
#17977 = EDGE_CURVE ( 'NONE', #14969, #18379, #16526, .T. ) ;
#17976 = CARTESIAN_POINT ( 'NONE',  ( 7.959375000614516971, -4.541064518000417216, -2.621784821875001281 ) ) ;
#17978 = CARTESIAN_POINT ( 'NONE',  ( 17.39999999999999858, 0.000000000000000000, 4.999999999999998224 ) ) ;
#17979 = CARTESIAN_POINT ( 'NONE',  ( 15.32812500061451644, 4.541064518000418104, 2.621784821874999949 ) ) ;
#17980 = CARTESIAN_POINT ( 'NONE',  ( -3.999999999999999556, 18.98749999999999716, 27.69059892324149175 ) ) ;
#17981 = DIRECTION ( 'NONE',  ( 1.000000000000000000, 0.000000000000000000, 0.000000000000000000 ) ) ;
#17982 = CARTESIAN_POINT ( 'NONE',  ( 20.22187500061451715, 2.746126346562645981, -4.756430356249997438 ) ) ;
#17983 = CARTESIAN_POINT ( 'NONE',  ( 9.890625000614516438, 6.054752690667223547, 3.707466751127219781E-16 ) ) ;
#17984 = CARTESIAN_POINT ( 'NONE',  ( 26.67187500061451644, 3.027376345333611329, 5.243569643749999010 ) ) ;
#17985 = CARTESIAN_POINT ( 'NONE',  ( 27.07500000122903216, -5.773502691896255534, -1.060575238724906372E-15 ) ) ;
#17986 = CARTESIAN_POINT ( 'NONE',  ( 25.77187500061451075, 3.027376345333611329, 5.243569643749999010 ) ) ;
#17987 = CARTESIAN_POINT ( 'NONE',  ( 7.537500000000002309, -2.886751345948129988, 4.999999999999997335 ) ) ;
#17988 = CARTESIAN_POINT ( 'NONE',  ( 2.000000000000001332, 13.06250000122903465, 33.46410161513774995 ) ) ;
#17989 = CARTESIAN_POINT ( 'NONE',  ( 15.02812500061451750, -4.541064518000419881, 2.621784821874995952 ) ) ;
#17990 = CARTESIAN_POINT ( 'NONE',  ( 6.900000001229035007, -2.886751345948125991, -5.000000000000000000 ) ) ;
#17991 = CARTESIAN_POINT ( 'NONE',  ( 17.55937500061451573, 4.541064518000418104, -2.621784821874998173 ) ) ;
#17992 = CARTESIAN_POINT ( 'NONE',  ( 11.85937500061451644, 0.000000000000000000, 5.243569643749999010 ) ) ;
#17993 = DIRECTION ( 'NONE',  ( -1.000000000000000000, -0.000000000000000000, -0.000000000000000000 ) ) ;
#17994 = ORIENTED_EDGE ( 'NONE', *, *, #7027, .F. ) ;
#17995 = CARTESIAN_POINT ( 'NONE',  ( 12.70312500061451821, 0.000000000000000000, 5.243569643749999010 ) ) ;
#17996 = CARTESIAN_POINT ( 'NONE',  ( 25.50000000122903288, 5.773502691896255534, 3.535250795749688894E-16 ) ) ;
#17997 = CARTESIAN_POINT ( 'NONE',  ( 13.80937500061451750, -4.541064518000417216, -2.621784821875001281 ) ) ;
#17998 = CARTESIAN_POINT ( 'NONE',  ( 45.00000000000000000, 6.123233995736764310E-16, -4.999999999999998224 ) ) ;
#17999 = CARTESIAN_POINT ( 'NONE',  ( 13.90312500061451750, 4.541064518000418104, -2.621784821874998173 ) ) ;
#18000 = CARTESIAN_POINT ( 'NONE',  ( 26.47500000122903430, 2.886751345948135317, 4.999999999999984013 ) ) ;
#18001 = EDGE_CURVE ( 'NONE', #18095, #46571, #58766, .T. ) ;
#18002 = CARTESIAN_POINT ( 'NONE',  ( 23.10937500061451644, 0.000000000000000000, 5.243569643749999010 ) ) ;
#18003 = CARTESIAN_POINT ( 'NONE',  ( -4.243569643749999898, 10.80312500061451786, 30.00000000000000000 ) ) ;
#18004 = CARTESIAN_POINT ( 'NONE',  ( 11.62500000122903465, 2.886751345948126879, 4.999999999999999112 ) ) ;
#18005 = CARTESIAN_POINT ( 'NONE',  ( 45.00000000000000000, 0.000000000000000000, 0.000000000000000000 ) ) ;
#18006 = CARTESIAN_POINT ( 'NONE',  ( 3.178125000614515638, 4.541064518000418104, 2.621784821874999949 ) ) ;
#18007 = CARTESIAN_POINT ( 'NONE',  ( -4.243569643749998122, 17.64687500061451786, -27.54997392385601174 ) ) ;
#18008 = CARTESIAN_POINT ( 'NONE',  ( 17.82187500061451502, -6.054752690667223547, -1.112240025338166033E-15 ) ) ;
#18009 = CARTESIAN_POINT ( 'NONE',  ( 19.08750000122903145, 6.123233995736764310E-16, -4.999999999999998224 ) ) ;
#18010 =( BOUNDED_CURVE ( )  B_SPLINE_CURVE ( 2, ( #2825, #53804, #54533, #3935, #29539, #3567, #43457, #26458, #48264 ),
 .UNSPECIFIED., .F., .F. ) 
 B_SPLINE_CURVE_WITH_KNOTS ( ( 3, 2, 2, 2, 3 ),
 ( 0.8472222222222222099, 0.8518518518518518601, 0.8611111111111111605, 0.8703703703703703498, 0.8750000000000000000 ),
 .UNSPECIFIED. ) 
 CURVE ( )  GEOMETRIC_REPRESENTATION_ITEM ( )  RATIONAL_B_SPLINE_CURVE ( ( 0.9330127018922194093, 0.9330127018922194093, 1.000000000000000000, 0.8660254037844387076, 1.000000000000000000, 0.8660254037844387076, 1.000000000000000000, 0.9330127018922194093, 0.9330127018922194093 ) ) 
 REPRESENTATION_ITEM ( '' )  );
#18011 = CARTESIAN_POINT ( 'NONE',  ( 13.88437500061451679, 6.421520780324663323E-16, -5.243569643749999010 ) ) ;
#18012 = DIRECTION ( 'NONE',  ( 0.000000000000000000, 0.000000000000000000, 1.000000000000000000 ) ) ;
#18013 = CARTESIAN_POINT ( 'NONE',  ( 20.02500000122903145, 2.886751345948129099, -4.999999999999998224 ) ) ;
#18014 = CARTESIAN_POINT ( 'NONE',  ( 15.47812500061451679, -4.541064518000419881, 2.621784821874995952 ) ) ;
#18015 = CARTESIAN_POINT ( 'NONE',  ( 29.35312500061451502, 0.000000000000000000, 5.243569643749999010 ) ) ;
#18016 = ORIENTED_EDGE ( 'NONE', *, *, #48583, .F. ) ;
#18017 = ORIENTED_EDGE ( 'NONE', *, *, #60732, .F. ) ;
#18018 = CARTESIAN_POINT ( 'NONE',  ( 18.67500000000000071, 4.330127018922191873, 2.499999999999999556 ) ) ;
#18019 = CARTESIAN_POINT ( 'NONE',  ( 19.31250000122903288, 0.000000000000000000, 4.999999999999998224 ) ) ;
#18020 = CARTESIAN_POINT ( 'NONE',  ( 4.153125000614515727, 0.000000000000000000, 5.243569643749999010 ) ) ;
#18021 = CARTESIAN_POINT ( 'NONE',  ( 15.30000000122903359, -2.886751345948129988, 4.999999999999997335 ) ) ;
#18022 = CARTESIAN_POINT ( 'NONE',  ( 26.37187500061451217, -6.054752690667223547, -1.112240025338166033E-15 ) ) ;
#18023 = CARTESIAN_POINT ( 'NONE',  ( 20.61562500061451431, 3.027376345333613106, -5.243569643749998122 ) ) ;
#18024 = CARTESIAN_POINT ( 'NONE',  ( 24.06562500061451715, -6.054752690667223547, -1.112240025338166033E-15 ) ) ;
#18025 = CARTESIAN_POINT ( 'NONE',  ( 4.115625000614516082, 3.027376345333611329, 5.243569643749999010 ) ) ;
#18026 = CARTESIAN_POINT ( 'NONE',  ( 27.67499999999999716, 4.330127018922191873, 2.499999999999999556 ) ) ;
#18027 = CARTESIAN_POINT ( 'NONE',  ( 4.602594079845841790, 1.953557899511747964, 4.866096033195304926 ) ) ;
#18028 =( BOUNDED_CURVE ( )  B_SPLINE_CURVE ( 2, ( #18936, #57385, #22056, #12686, #35223, #33495, #68487, #23408, #29681 ),
 .UNSPECIFIED., .F., .F. ) 
 B_SPLINE_CURVE_WITH_KNOTS ( ( 3, 2, 2, 2, 3 ),
 ( 0.6413043478260869179, 0.6449275362318840354, 0.6521739130434782705, 0.6594202898550725056, 0.6630434782608696231 ),
 .UNSPECIFIED. ) 
 CURVE ( )  GEOMETRIC_REPRESENTATION_ITEM ( )  RATIONAL_B_SPLINE_CURVE ( ( 0.9330127018922194093, 0.9330127018922194093, 1.000000000000000000, 0.8660254037844387076, 1.000000000000000000, 0.8660254037844387076, 1.000000000000000000, 0.9330127018922182991, 0.9330127018922192983 ) ) 
 REPRESENTATION_ITEM ( '' )  );
#18029 = CARTESIAN_POINT ( 'NONE',  ( 8.484375000614518214, 5.824947211148865298E-16, -4.756430356249998326 ) ) ;
#18030 = CARTESIAN_POINT ( 'NONE',  ( 1.999999999999997335, 17.82499999999999929, 33.46410161513775705 ) ) ;
#18031 = CARTESIAN_POINT ( 'NONE',  ( 28.76250000000000284, -5.773502691896255534, -1.060575238724906372E-15 ) ) ;
#18032 = CARTESIAN_POINT ( 'NONE',  ( 4.243569643749999898, 16.93437500061451573, -30.00000000000000000 ) ) ;
#18033 = CARTESIAN_POINT ( 'NONE',  ( 6.337500001229033231, -4.330127018922194537, 2.499999999999995559 ) ) ;
#18034 = CARTESIAN_POINT ( 'NONE',  ( 6.412500000000001421, 2.886751345948129099, -4.999999999999998224 ) ) ;
#18035 = CARTESIAN_POINT ( 'NONE',  ( 3.037500001229032964, 4.330127018922191873, 2.499999999999999556 ) ) ;
#18036 = CARTESIAN_POINT ( 'NONE',  ( 10.35937500061451644, 4.541064518000418104, -2.621784821874998173 ) ) ;
#18037 = CYLINDRICAL_SURFACE ( 'NONE', #65444, 1.500000000000000444 ) ;
#18038 = DIRECTION ( 'NONE',  ( 0.000000000000000000, 0.000000000000000000, 1.000000000000000000 ) ) ;
#18039 = CARTESIAN_POINT ( 'NONE',  ( -5.918438294331348715, 8.060677219855273634, -31.00586393815197894 ) ) ;
#18040 = CARTESIAN_POINT ( 'NONE',  ( 8.859375000614518214, -4.541064518000417216, -2.621784821875001281 ) ) ;
#18041 = CARTESIAN_POINT ( 'NONE',  ( 13.39687500061451608, -3.027376345333610441, -5.243569643749999898 ) ) ;
#18042 = CARTESIAN_POINT ( 'NONE',  ( 5.512499999999999289, 2.886751345948129099, -4.999999999999998224 ) ) ;
#18043 = CARTESIAN_POINT ( 'NONE',  ( -3.000416591977282496E-16, 16.09062500061459744, 25.09994784771203058 ) ) ;
#18044 = CARTESIAN_POINT ( 'NONE',  ( 20.55937500061451573, -4.541064518000417216, -2.621784821875001281 ) ) ;
#18045 = CARTESIAN_POINT ( 'NONE',  ( 9.637499999999999289, 5.773502691896255534, 3.535250795749688401E-16 ) ) ;
#18046 = CARTESIAN_POINT ( 'NONE',  ( 25.72500000122903074, -5.773502691896255534, -1.060575238724906372E-15 ) ) ;
#18047 = CARTESIAN_POINT ( 'NONE',  ( 18.45937500061451431, 2.746126346562643317, 4.756430356249998326 ) ) ;
#18048 = CARTESIAN_POINT ( 'NONE',  ( 23.76562500061451644, 3.027376345333613106, -5.243569643749998122 ) ) ;
#18049 = CARTESIAN_POINT ( 'NONE',  ( 14.12812500061451715, -4.541064518000419881, 2.621784821874995952 ) ) ;
#18050 = CARTESIAN_POINT ( 'NONE',  ( 25.73437500061451644, -2.746126346562646425, 4.756430356249996549 ) ) ;
#18051 = CARTESIAN_POINT ( 'NONE',  ( 11.03437500061451715, -4.541064518000419881, 2.621784821874995952 ) ) ;
#18052 = CARTESIAN_POINT ( 'NONE',  ( 29.28749999999999787, -2.886751345948125991, -5.000000000000000000 ) ) ;
#18053 = CARTESIAN_POINT ( 'NONE',  ( 23.43750000122902932, -4.330127018922194537, 2.499999999999995559 ) ) ;
#18054 = CYLINDRICAL_SURFACE ( 'NONE', #21357, 4.000000000000000000 ) ;
#18055 = CARTESIAN_POINT ( 'NONE',  ( 10.95937500061451964, 0.000000000000000000, 5.243569643749999010 ) ) ;
#18056 = CARTESIAN_POINT ( 'NONE',  ( 29.22187500061451715, 3.027376345333613106, -5.243569643749998122 ) ) ;
#18057 = CARTESIAN_POINT ( 'NONE',  ( 4.134375000614517681, 4.541064518000418104, 2.621784821874999949 ) ) ;
#18058 = DIRECTION ( 'NONE',  ( 1.000000000000000000, 0.000000000000000000, 0.000000000000000000 ) ) ;
#18059 = CARTESIAN_POINT ( 'NONE',  ( 21.49687500061451573, -3.027376345333610441, -5.243569643749999898 ) ) ;
#18060 = CARTESIAN_POINT ( 'NONE',  ( 14.59687500061452070, -3.027376345333614438, 5.243569643749998122 ) ) ;
#18061 = CARTESIAN_POINT ( 'NONE',  ( -7.967954043666661671E-16, 18.04062499938548214, 34.33755215474603517 ) ) ;
#18062 = CARTESIAN_POINT ( 'NONE',  ( 25.16249999999999432, -5.773502691896255534, -1.060575238724906372E-15 ) ) ;
#18063 = CARTESIAN_POINT ( 'NONE',  ( 3.756430356250000102, 20.29062499938548569, 30.00000000000000000 ) ) ;
#18064 = CARTESIAN_POINT ( 'NONE',  ( 26.40937500061451715, -4.119189519843965641, -2.378215178125001383 ) ) ;
#18065 = CARTESIAN_POINT ( 'NONE',  ( 16.90312500061451573, -4.541064518000417216, -2.621784821875001281 ) ) ;
#18066 = CARTESIAN_POINT ( 'NONE',  ( 8.175000000000002487, 6.123233995736764310E-16, -4.999999999999998224 ) ) ;
#18067 = CARTESIAN_POINT ( 'NONE',  ( -1.999999999999997113, 14.22500000000000142, 33.46410161513775705 ) ) ;
#18068 = CARTESIAN_POINT ( 'NONE',  ( 14.21249999999999858, 2.886751345948126879, 4.999999999999999112 ) ) ;
#18069 = CARTESIAN_POINT ( 'NONE',  ( -2.121784821874996840, 10.42812500061451786, 33.67503911421598417 ) ) ;
#18070 = CARTESIAN_POINT ( 'NONE',  ( 17.06250000122903288, 0.000000000000000000, 4.999999999999998224 ) ) ;
#18071 = CARTESIAN_POINT ( 'NONE',  ( 25.80937500061451928, 0.000000000000000000, 5.243569643749999010 ) ) ;
#18072 = ORIENTED_EDGE ( 'NONE', *, *, #40917, .T. ) ;
#18073 = CARTESIAN_POINT ( 'NONE',  ( 21.70312500061451644, 0.000000000000000000, 5.243569643749999010 ) ) ;
#18074 = CARTESIAN_POINT ( 'NONE',  ( 20.74687500061451573, 6.054752690667223547, 3.707466751127219781E-16 ) ) ;
#18075 = CARTESIAN_POINT ( 'NONE',  ( 4.612500000000002487, 2.886751345948129099, -4.999999999999998224 ) ) ;
#18076 = CARTESIAN_POINT ( 'NONE',  ( 7.153125000614518392, 4.541064518000418104, -2.621784821874998173 ) ) ;
#18077 = CARTESIAN_POINT ( 'NONE',  ( 21.96562500061451573, 3.027376345333613106, -5.243569643749998122 ) ) ;
#18078 = CARTESIAN_POINT ( 'NONE',  ( 13.28437500061451715, -4.541064518000419881, 2.621784821874995952 ) ) ;
#18079 = CARTESIAN_POINT ( 'NONE',  ( 16.32187500061451502, 3.027376345333611329, 5.243569643749999010 ) ) ;
#18080 = CARTESIAN_POINT ( 'NONE',  ( -4.243569643749997233, 16.69062500061451360, 32.45002607614398471 ) ) ;
#18081 = CARTESIAN_POINT ( 'NONE',  ( 18.97500000122903074, -5.773502691896255534, -1.060575238724906372E-15 ) ) ;
#18082 = CARTESIAN_POINT ( 'NONE',  ( 14.25937500061451679, -4.119189519843965641, -2.378215178125001383 ) ) ;
#18083 = CARTESIAN_POINT ( 'NONE',  ( 9.478125000614515017, 4.541064518000418104, 2.621784821874999949 ) ) ;
#18084 = CARTESIAN_POINT ( 'NONE',  ( 5.634375000614519458, -4.541064518000419881, 2.621784821874995952 ) ) ;
#18085 = CARTESIAN_POINT ( 'NONE',  ( 4.096875000614518925, 6.054752690667223547, 3.707466751127219781E-16 ) ) ;
#18086 = CARTESIAN_POINT ( 'NONE',  ( 25.35937500061451644, 0.000000000000000000, 5.243569643749999010 ) ) ;
#18087 = CARTESIAN_POINT ( 'NONE',  ( 17.72812500061451502, -4.541064518000419881, 2.621784821874995952 ) ) ;
#18088 = CARTESIAN_POINT ( 'NONE',  ( 28.23750000122903359, 4.330127018922191873, 2.499999999999999556 ) ) ;
#18089 = CARTESIAN_POINT ( 'NONE',  ( 24.21562500061451573, 3.027376345333613106, -5.243569643749998122 ) ) ;
#18090 = CARTESIAN_POINT ( 'NONE',  ( 21.27187500061451786, 3.027376345333611329, 5.243569643749999010 ) ) ;
#18091 = CARTESIAN_POINT ( 'NONE',  ( 18.17812500061451786, -4.541064518000419881, 2.621784821874995952 ) ) ;
#18092 = CARTESIAN_POINT ( 'NONE',  ( 2.121784821875001281, 17.75937500061451502, 33.67503911421598417 ) ) ;
#18093 = CARTESIAN_POINT ( 'NONE',  ( 21.25312500061451715, 0.000000000000000000, 5.243569643749999010 ) ) ;
#18094 = CARTESIAN_POINT ( 'NONE',  ( 5.810221930991193690E-16, 19.36250000000000071, 26.00000000000000000 ) ) ;
#18095 = VERTEX_POINT ( 'NONE', #56067 ) ;
#18096 = CARTESIAN_POINT ( 'NONE',  ( 25.19999999999999929, -4.330127018922190985, -2.500000000000001332 ) ) ;
#18097 = CARTESIAN_POINT ( 'NONE',  ( -3.999999999999997335, 12.83750000000000213, -27.69059892324149175 ) ) ;
#18098 = CARTESIAN_POINT ( 'NONE',  ( 3.756430356250000546, 20.44062499938547717, 27.83122392262697886 ) ) ;
#18099 = CARTESIAN_POINT ( 'NONE',  ( 28.49062500061451431, -3.027376345333614438, 5.243569643749998122 ) ) ;
#18100 = CARTESIAN_POINT ( 'NONE',  ( 10.26562500061451644, 3.027376345333613106, -5.243569643749998122 ) ) ;
#18101 = CARTESIAN_POINT ( 'NONE',  ( 22.95000000122903216, -2.886751345948129988, 4.999999999999997335 ) ) ;
#18102 = CARTESIAN_POINT ( 'NONE',  ( 27.40312500061451573, 4.541064518000418104, -2.621784821874998173 ) ) ;
#18103 = CARTESIAN_POINT ( 'NONE',  ( 27.22499999999999787, 4.330127018922191873, 2.499999999999999556 ) ) ;
#18104 = CARTESIAN_POINT ( 'NONE',  ( -3.999999999999999556, 15.57500000122903216, -32.30940107675850470 ) ) ;
#18105 = CARTESIAN_POINT ( 'NONE',  ( 29.54062500061451502, -3.027376345333610441, -5.243569643749999898 ) ) ;
#18106 = CARTESIAN_POINT ( 'NONE',  ( 11.46562500061451573, -6.054752690667223547, -1.112240025338166033E-15 ) ) ;
#18107 = ORIENTED_EDGE ( 'NONE', *, *, #63501, .F. ) ;
#18108 = CARTESIAN_POINT ( 'NONE',  ( 26.54062500061451146, 6.054752690667223547, 3.707466751127219781E-16 ) ) ;
#18109 = CARTESIAN_POINT ( 'NONE',  ( 7.228125000614517681, 4.541064518000418104, 2.621784821874999949 ) ) ;
#18110 = CARTESIAN_POINT ( 'NONE',  ( 6.665625000614515905, 3.027376345333613106, -5.243569643749998122 ) ) ;
#18111 = CARTESIAN_POINT ( 'NONE',  ( 15.90937500061451892, 0.000000000000000000, 4.756430356249998326 ) ) ;
#18112 = CARTESIAN_POINT ( 'NONE',  ( 17.73750000122903359, 6.123233995736764310E-16, -4.999999999999998224 ) ) ;
#18113 = CARTESIAN_POINT ( 'NONE',  ( 15.71250000000000213, -5.773502691896255534, -1.060575238724906372E-15 ) ) ;
#18114 = EDGE_CURVE ( 'NONE', #71973, #41056, #16293, .T. ) ;
#18115 = CARTESIAN_POINT ( 'NONE',  ( 16.80937500061451573, 0.000000000000000000, 5.243569643749999010 ) ) ;
#18116 = CARTESIAN_POINT ( 'NONE',  ( 11.13750000122903216, 4.330127018922191873, 2.499999999999999556 ) ) ;
#18117 = CARTESIAN_POINT ( 'NONE',  ( 16.35937500061451644, 0.000000000000000000, 5.243569643749999010 ) ) ;
#18118 = CARTESIAN_POINT ( 'NONE',  ( 17.17500000000000071, 6.123233995736764310E-16, -4.999999999999998224 ) ) ;
#18119 = CARTESIAN_POINT ( 'NONE',  ( 20.22187500061451715, 3.027376345333613106, -5.243569643749998122 ) ) ;
#18120 = CARTESIAN_POINT ( 'NONE',  ( 4.243569643749999898, 12.82812500061451821, -30.00000000000000000 ) ) ;
#18121 = DIRECTION ( 'NONE',  ( 0.000000000000000000, 1.000000000000000000, -0.000000000000000000 ) ) ;
#18122 = CARTESIAN_POINT ( 'NONE',  ( 23.37187500061451573, 4.119189519843966529, 2.378215178124999607 ) ) ;
#18123 = CARTESIAN_POINT ( 'NONE',  ( 1.071796769724485232, 15.23615380933862973, 25.99999999999999645 ) ) ;
#18124 = CARTESIAN_POINT ( 'NONE',  ( 25.22812500061451502, 4.541064518000418104, 2.621784821874999949 ) ) ;
#18125 = CARTESIAN_POINT ( 'NONE',  ( 28.24687500061451573, -3.027376345333610441, -5.243569643749999898 ) ) ;
#18126 = CARTESIAN_POINT ( 'NONE',  ( 23.92499999999999716, 6.123233995736764310E-16, -4.999999999999998224 ) ) ;
#18127 = CARTESIAN_POINT ( 'NONE',  ( 7.565625000614518036, 3.027376345333613106, -5.243569643749998122 ) ) ;
#18128 = CARTESIAN_POINT ( 'NONE',  ( 24.94687500061451502, -4.119189519843965641, -2.378215178125001383 ) ) ;
#18129 = CARTESIAN_POINT ( 'NONE',  ( 18.57187500061451857, 3.027376345333611329, 5.243569643749999010 ) ) ;
#18130 = CARTESIAN_POINT ( 'NONE',  ( 12.34687500061451537, -4.119189519843965641, -2.378215178125001383 ) ) ;
#18131 = CARTESIAN_POINT ( 'NONE',  ( 28.80000000122903003, -2.886751345948129988, 4.999999999999997335 ) ) ;
#18132 = CARTESIAN_POINT ( 'NONE',  ( 7.734375000614517326, 4.541064518000418104, 2.621784821874999949 ) ) ;
#18133 = ORIENTED_EDGE ( 'NONE', *, *, #26472, .T. ) ;
#18134 = CARTESIAN_POINT ( 'NONE',  ( 18.57187500061451857, 3.027376345333611329, 5.243569643749999010 ) ) ;
#18135 = CARTESIAN_POINT ( 'NONE',  ( 16.61250000000000071, -5.773502691896255534, -1.060575238724906372E-15 ) ) ;
#18136 = CARTESIAN_POINT ( 'NONE',  ( 27.26249999999999929, 2.886751345948126879, 4.999999999999999112 ) ) ;
#18137 = CARTESIAN_POINT ( 'NONE',  ( 28.88437500061451502, 4.541064518000418104, 2.621784821874999949 ) ) ;
#18138 = CARTESIAN_POINT ( 'NONE',  ( 26.38125000122903430, 4.330127018922191873, 2.499999999999999556 ) ) ;
#18139 = CARTESIAN_POINT ( 'NONE',  ( 20.83125000122903359, 6.123233995736764310E-16, -4.999999999999998224 ) ) ;
#18140 = ORIENTED_EDGE ( 'NONE', *, *, #47732, .T. ) ;
#18141 = CARTESIAN_POINT ( 'NONE',  ( 9.787499999999999645, -2.886751345948129988, 4.999999999999997335 ) ) ;
#18142 = CARTESIAN_POINT ( 'NONE',  ( 12.68437500061451750, -2.746126346562646425, 4.756430356249996549 ) ) ;
#18143 = CARTESIAN_POINT ( 'NONE',  ( 25.60312500061451502, 4.541064518000418104, -2.621784821874998173 ) ) ;
#18144 = CARTESIAN_POINT ( 'NONE',  ( 13.23750000000000071, 5.773502691896255534, 3.535250795749688894E-16 ) ) ;
#18145 =( BOUNDED_CURVE ( )  B_SPLINE_CURVE ( 2, ( #11348, #56408, #5799, #22775, #45326, #67862, #17233 ),
 .UNSPECIFIED., .F., .F. ) 
 B_SPLINE_CURVE_WITH_KNOTS ( ( 3, 2, 2, 3 ),
 ( 0.8499999999999999778, 0.8527777777777777457, 0.8555555555555555136, 0.8583333333333332815 ),
 .UNSPECIFIED. ) 
 CURVE ( )  GEOMETRIC_REPRESENTATION_ITEM ( )  RATIONAL_B_SPLINE_CURVE ( ( 1.000000000000000000, 0.8660254037844387076, 1.000000000000000000, 0.8660254037844387076, 1.000000000000000000, 0.8660254037844387076, 1.000000000000000000 ) ) 
 REPRESENTATION_ITEM ( '' )  );
#18146 = CARTESIAN_POINT ( 'NONE',  ( 9.787500001229036073, 4.330127018922191873, 2.499999999999999556 ) ) ;
#18147 = CARTESIAN_POINT ( 'NONE',  ( 9.215625000614515727, -6.054752690667223547, -1.112240025338166033E-15 ) ) ;
#18148 = CARTESIAN_POINT ( 'NONE',  ( 23.06250000000000355, 2.886751345948129099, -4.999999999999998224 ) ) ;
#18149 = CARTESIAN_POINT ( 'NONE',  ( 21.40312500061451573, -4.541064518000417216, -2.621784821875001281 ) ) ;
#18150 = CYLINDRICAL_SURFACE ( 'NONE', #50231, 4.999999999999998224 ) ;
#18151 = CARTESIAN_POINT ( 'NONE',  ( 25.87500000122903288, 2.886751345948129099, -4.999999999999998224 ) ) ;
#18152 = CARTESIAN_POINT ( 'NONE',  ( -3.756430356249999214, 15.97812499938548392, 27.83122392262697176 ) ) ;
#18153 = CARTESIAN_POINT ( 'NONE',  ( 8.137500000000002842, -2.886751345948125991, -5.000000000000000000 ) ) ;
#18154 = EDGE_LOOP ( 'NONE', ( #28839, #27904, #2593, #67778 ) ) ;
#18155 = CARTESIAN_POINT ( 'NONE',  ( 22.41562500061451502, 3.027376345333613106, -5.243569643749998122 ) ) ;
#18156 = CARTESIAN_POINT ( 'NONE',  ( 29.50312500061451360, -4.541064518000417216, -2.621784821875001281 ) ) ;
#18157 = CARTESIAN_POINT ( 'NONE',  ( 26.03437500061451715, 6.421520780324663323E-16, -5.243569643749999010 ) ) ;
#18158 = CARTESIAN_POINT ( 'NONE',  ( 17.85937500061451999, -4.541064518000417216, -2.621784821875001281 ) ) ;
#18159 = CARTESIAN_POINT ( 'NONE',  ( 13.19062500061451537, -3.027376345333614438, 5.243569643749998122 ) ) ;
#18160 = CARTESIAN_POINT ( 'NONE',  ( 12.20625000122903181, -4.330127018922190985, -2.500000000000001332 ) ) ;
#18161 = CARTESIAN_POINT ( 'NONE',  ( 26.88750000122903216, 4.330127018922191873, 2.499999999999999556 ) ) ;
#18162 = CARTESIAN_POINT ( 'NONE',  ( 21.87187500061451573, -5.492252693125287522, -1.008910452111647106E-15 ) ) ;
#18163 = CARTESIAN_POINT ( 'NONE',  ( 16.00312500061451715, -4.541064518000417216, -2.621784821875001281 ) ) ;
#18164 = CARTESIAN_POINT ( 'NONE',  ( 13.38750000000000107, -2.886751345948130876, 4.999999999999996447 ) ) ;
#18165 = CARTESIAN_POINT ( 'NONE',  ( 2.662500001229036073, 0.000000000000000000, 4.999999999999998224 ) ) ;
#18166 = CARTESIAN_POINT ( 'NONE',  ( 13.02187500061451608, 3.027376345333613106, -5.243569643749998122 ) ) ;
#18167 = CARTESIAN_POINT ( 'NONE',  ( 11.44687500061451857, -3.027376345333614438, 5.243569643749998122 ) ) ;
#18168 = CARTESIAN_POINT ( 'NONE',  ( 21.08437500061451786, 6.421520780324663323E-16, -5.243569643749999010 ) ) ;
#18169 = VERTEX_POINT ( 'NONE', #73056 ) ;
#18170 = CARTESIAN_POINT ( 'NONE',  ( 29.55000000000000071, 0.000000000000000000, 4.999999999999998224 ) ) ;
#18171 = CARTESIAN_POINT ( 'NONE',  ( 23.46562500061451573, 3.027376345333611329, 5.243569643749999010 ) ) ;
#18172 = CARTESIAN_POINT ( 'NONE',  ( 19.47187500061451360, 3.027376345333611329, 5.243569643749999010 ) ) ;
#18173 = CARTESIAN_POINT ( 'NONE',  ( 24.36562500061451786, 3.027376345333611329, 5.243569643749999010 ) ) ;
#18174 = CARTESIAN_POINT ( 'NONE',  ( 27.11250000000000071, 2.886751345948112668, -5.000000000000024869 ) ) ;
#18175 = CARTESIAN_POINT ( 'NONE',  ( -3.999999999999999556, 13.21250000000000213, 27.69059892324149530 ) ) ;
#18176 = AXIS2_PLACEMENT_3D ( 'NONE', #18390, #29496, #17312 ) ;
#18177 = CARTESIAN_POINT ( 'NONE',  ( 28.26562500061451289, 3.027376345333613106, -5.243569643749998122 ) ) ;
#18178 = CARTESIAN_POINT ( 'NONE',  ( 9.487500001229033586, -4.330127018922194537, 2.499999999999995559 ) ) ;
#18179 = CARTESIAN_POINT ( 'NONE',  ( 4.387500001229033053, 4.330127018922191873, 2.499999999999999556 ) ) ;
#18180 = CARTESIAN_POINT ( 'NONE',  ( 21.37499999999999645, 4.330127018922191873, 2.499999999999999556 ) ) ;
#18181 = CARTESIAN_POINT ( 'NONE',  ( 26.13750000122903216, -4.330127018922194537, 2.499999999999995559 ) ) ;
#18182 = CARTESIAN_POINT ( 'NONE',  ( 4.000000000000000000, 20.54374999877096641, 30.00000000000000000 ) ) ;
#18183 = CARTESIAN_POINT ( 'NONE',  ( 17.19375000122903430, -2.886751345948125991, -5.000000000000000000 ) ) ;
#18184 = CARTESIAN_POINT ( 'NONE',  ( 8.371875000614515727, -6.054752690667223547, -1.112240025338166033E-15 ) ) ;
#18185 = CARTESIAN_POINT ( 'NONE',  ( 17.72812500061451502, -4.541064518000419881, 2.621784821874995952 ) ) ;
#18186 = CARTESIAN_POINT ( 'NONE',  ( 10.20937500061451786, -4.541064518000417216, -2.621784821875001281 ) ) ;
#18187 = CARTESIAN_POINT ( 'NONE',  ( 29.17500000122903714, 2.886751345948126879, 4.999999999999999112 ) ) ;
#18188 = CARTESIAN_POINT ( 'NONE',  ( 19.17187500061451644, -6.054752690667223547, -1.112240025338166033E-15 ) ) ;
#18189 = CARTESIAN_POINT ( 'NONE',  ( 8.634375000614518569, 4.541064518000418104, 2.621784821874999949 ) ) ;
#18190 = CARTESIAN_POINT ( 'NONE',  ( 3.140625000614516882, 6.054752690667223547, 3.707466751127219781E-16 ) ) ;
#18191 = DIRECTION ( 'NONE',  ( -1.000000000000000000, 0.000000000000000000, -0.000000000000000000 ) ) ;
#18192 = CARTESIAN_POINT ( 'NONE',  ( 8.090625000614515727, 6.054752690667223547, 3.707466751127219781E-16 ) ) ;
#18193 = CARTESIAN_POINT ( 'NONE',  ( 17.91562500061451502, 3.027376345333613106, -5.243569643749998122 ) ) ;
#18194 = VERTEX_POINT ( 'NONE', #27999 ) ;
#18195 = CARTESIAN_POINT ( 'NONE',  ( 6.412500001229036073, -4.330127018922190985, -2.500000000000001332 ) ) ;
#18196 = CARTESIAN_POINT ( 'NONE',  ( 14.05312500061451431, 0.000000000000000000, 5.243569643749999010 ) ) ;
#18197 = CARTESIAN_POINT ( 'NONE',  ( 12.25312500061451537, 0.000000000000000000, 5.243569643749999010 ) ) ;
#18198 = CARTESIAN_POINT ( 'NONE',  ( 22.77187500061451786, -5.492252693125287522, -1.008910452111647106E-15 ) ) ;
#18199 = CARTESIAN_POINT ( 'NONE',  ( 12.86250000000000071, 2.886751345948126879, 4.999999999999999112 ) ) ;
#18200 = CARTESIAN_POINT ( 'NONE',  ( 5.662500001229035185, 4.330127018922192761, -2.499999999999997780 ) ) ;
#18201 = CARTESIAN_POINT ( 'NONE',  ( 4.378125000614518925, 6.421520780324663323E-16, -5.243569643749999010 ) ) ;
#18202 =( BOUNDED_CURVE ( )  B_SPLINE_CURVE ( 2, ( #31046, #69134, #24042, #31421, #53214, #2254, #58376 ),
 .UNSPECIFIED., .F., .F. ) 
 B_SPLINE_CURVE_WITH_KNOTS ( ( 3, 2, 2, 3 ),
 ( 0.1499999999999999944, 0.1533333333333333215, 0.1566666666666666485, 0.1599999999999999756 ),
 .UNSPECIFIED. ) 
 CURVE ( )  GEOMETRIC_REPRESENTATION_ITEM ( )  RATIONAL_B_SPLINE_CURVE ( ( 1.000000000000000000, 0.8660254037844387076, 1.000000000000000000, 0.8660254037844387076, 1.000000000000000000, 0.8660254037844398178, 0.9999999999999988898 ) ) 
 REPRESENTATION_ITEM ( '' )  );
#18203 = EDGE_CURVE ( 'NONE', #31631, #15981, #34201, .T. ) ;
#18204 = CARTESIAN_POINT ( 'NONE',  ( 19.57500000122903216, 2.886751345948129099, -4.999999999999998224 ) ) ;
#18205 = CARTESIAN_POINT ( 'NONE',  ( 25.01249999999999929, 2.886751345948126879, 4.999999999999999112 ) ) ;
#18206 = CARTESIAN_POINT ( 'NONE',  ( 9.001249775931846008E-16, 11.87187500061451750, -25.09994784771203058 ) ) ;
#18207 = CARTESIAN_POINT ( 'NONE',  ( 4.196151849995945149, -2.718880220196457476, -4.196151849995952254 ) ) ;
#18208 = CARTESIAN_POINT ( 'NONE',  ( 22.91250000122903430, 0.000000000000000000, 4.999999999999998224 ) ) ;
#18209 = DIRECTION ( 'NONE',  ( -1.000000000000000000, -0.000000000000000000, -0.000000000000000000 ) ) ;
#18210 = CARTESIAN_POINT ( 'NONE',  ( 17.59687500061451715, 6.054752690667223547, 3.707466751127219781E-16 ) ) ;
#18211 = LINE ( 'NONE', #23410, #46870 ) ;
#18212 = CARTESIAN_POINT ( 'NONE',  ( 14.80312500061451608, 4.541064518000418104, -2.621784821874998173 ) ) ;
#18213 = CARTESIAN_POINT ( 'NONE',  ( 10.36875000122903323, -5.773502691896255534, -1.060575238724906372E-15 ) ) ;
#18214 = CARTESIAN_POINT ( 'NONE',  ( 27.42187500061451644, 3.027376345333613106, -5.243569643749998122 ) ) ;
#18215 = CARTESIAN_POINT ( 'NONE',  ( 18.72187500061451360, 5.824947211148865298E-16, -4.756430356249998326 ) ) ;
#18216 = CARTESIAN_POINT ( 'NONE',  ( 11.80312500061451608, 0.000000000000000000, 5.243569643749999010 ) ) ;
#18217 = CARTESIAN_POINT ( 'NONE',  ( 16.05937500061451573, -4.541064518000417216, -2.621784821875001281 ) ) ;
#18218 = ORIENTED_EDGE ( 'NONE', *, *, #32403, .F. ) ;
#18219 = CARTESIAN_POINT ( 'NONE',  ( 26.69062500061451715, -3.027376345333614438, 5.243569643749998122 ) ) ;
#18220 = CARTESIAN_POINT ( 'NONE',  ( 19.86562500061451786, 3.027376345333611329, 5.243569643749999010 ) ) ;
#18221 = CARTESIAN_POINT ( 'NONE',  ( 29.16562500061451502, 3.027376345333613106, -5.243569643749998122 ) ) ;
#18222 = CARTESIAN_POINT ( 'NONE',  ( 20.36249999999999361, 2.886751345948073588, -5.000000000000094147 ) ) ;
#18223 = CARTESIAN_POINT ( 'NONE',  ( 9.712500000000002132, 2.886751345948126879, 4.999999999999999112 ) ) ;
#18224 = CARTESIAN_POINT ( 'NONE',  ( 20.32500000122903572, -5.773502691896255534, -1.060575238724906372E-15 ) ) ;
#18225 = CARTESIAN_POINT ( 'NONE',  ( 2.000000000000001332, 10.25000000000000000, 33.46410161513774995 ) ) ;
#18226 = CARTESIAN_POINT ( 'NONE',  ( 10.47187500061451715, -4.119189519843968306, 2.378215178124996054 ) ) ;
#18227 = ORIENTED_EDGE ( 'NONE', *, *, #38783, .T. ) ;
#18228 = CARTESIAN_POINT ( 'NONE',  ( 16.80000000000000071, 4.330127018922192761, -2.499999999999997780 ) ) ;
#18229 = CARTESIAN_POINT ( 'NONE',  ( 22.05000000000000071, -4.330127018922190985, -2.500000000000001332 ) ) ;
#18230 = CARTESIAN_POINT ( 'NONE',  ( 18.42187500061451644, 3.027376345333613106, -5.243569643749998122 ) ) ;
#18231 = CARTESIAN_POINT ( 'NONE',  ( 25.00312500061451715, -4.541064518000417216, -2.621784821875001281 ) ) ;
#18233 = VERTEX_POINT ( 'NONE', #43897 ) ;
#18232 = AXIS2_PLACEMENT_3D ( 'NONE', #49001, #59697, #53808 ) ;
#18234 = CARTESIAN_POINT ( 'NONE',  ( 8.737500001229033586, 6.123233995736764310E-16, -4.999999999999998224 ) ) ;
#18235 = CARTESIAN_POINT ( 'NONE',  ( 7.940625000614518036, -3.027376345333610441, -5.243569643749999898 ) ) ;
#18236 = CARTESIAN_POINT ( 'NONE',  ( 0.6945846161026939525, 20.50052346155192140, 33.93923243933046763 ) ) ;
#18237 = CARTESIAN_POINT ( 'NONE',  ( 14.43750000000000000, -2.886751345948125991, -5.000000000000000000 ) ) ;
#18238 = CARTESIAN_POINT ( 'NONE',  ( 2.121784821875001281, 17.25312500061451715, 33.67503911421598417 ) ) ;
#18239 = CARTESIAN_POINT ( 'NONE',  ( 28.41562500061451502, 3.027376345333611329, 5.243569643749999010 ) ) ;
#18240 = CARTESIAN_POINT ( 'NONE',  ( 9.487500000000000711, -2.886751345948125991, -5.000000000000000000 ) ) ;
#18241 = CARTESIAN_POINT ( 'NONE',  ( 3.756430356250000102, 18.04062499938548214, 30.00000000000000000 ) ) ;
#18242 = CARTESIAN_POINT ( 'NONE',  ( 26.22187500061451715, 3.027376345333611329, 5.243569643749999010 ) ) ;
#18243 = ORIENTED_EDGE ( 'NONE', *, *, #17583, .F. ) ;
#18244 = CARTESIAN_POINT ( 'NONE',  ( 21.81562500061451004, -6.054752690667223547, -1.112240025338166033E-15 ) ) ;
#18245 = CARTESIAN_POINT ( 'NONE',  ( 22.62187500061451573, 3.027376345333611329, 5.243569643749999010 ) ) ;
#18246 = CARTESIAN_POINT ( 'NONE',  ( 2.121784821874999061, 16.05312500061459247, -33.67503911421598417 ) ) ;
#18247 = CARTESIAN_POINT ( 'NONE',  ( 10.31250000000000355, -5.773502691896255534, -1.060575238724906372E-15 ) ) ;
#18248 = CARTESIAN_POINT ( 'NONE',  ( 6.928125000614516082, -4.541064518000419881, 2.621784821874995952 ) ) ;
#18249 = CARTESIAN_POINT ( 'NONE',  ( 29.29687500061450933, 5.492252693125287522, 3.363034840372157021E-16 ) ) ;
#18250 = CARTESIAN_POINT ( 'NONE',  ( 22.97812500061451857, 4.541064518000418104, 2.621784821874999949 ) ) ;
#18251 = CARTESIAN_POINT ( 'NONE',  ( 28.05937500061451217, -5.492252693125287522, -1.008910452111647106E-15 ) ) ;
#18252 = CARTESIAN_POINT ( 'NONE',  ( 12.23437500061451821, 4.119189519843966529, 2.378215178124999607 ) ) ;
#18253 = CARTESIAN_POINT ( 'NONE',  ( 16.35937500061451644, 0.000000000000000000, 5.243569643749999010 ) ) ;
#18254 = CARTESIAN_POINT ( 'NONE',  ( -4.243569643749997233, 12.69687500061451857, 32.45002607614398471 ) ) ;
#18255 = CARTESIAN_POINT ( 'NONE',  ( 18.04687500061451999, 6.054752690667223547, 3.707466751127219781E-16 ) ) ;
#18256 = CARTESIAN_POINT ( 'NONE',  ( 26.29687500061451644, -3.027376345333614438, 5.243569643749998122 ) ) ;
#18257 = CARTESIAN_POINT ( 'NONE',  ( -4.243569643749999898, 15.77187500061451608, 27.54997392385601529 ) ) ;
#18258 = CARTESIAN_POINT ( 'NONE',  ( 7.715625000614515727, 3.027376345333611329, 5.243569643749999010 ) ) ;
#18259 = CARTESIAN_POINT ( 'NONE',  ( 1.071796769724489895, 10.52990381179670010, -34.00000000000000000 ) ) ;
#18260 = CARTESIAN_POINT ( 'NONE',  ( 5.221875000614519813, -6.054752690667223547, -1.112240025338166033E-15 ) ) ;
#18261 = FACE_OUTER_BOUND ( 'NONE', #34074, .T. ) ;
#18262 = CARTESIAN_POINT ( 'NONE',  ( 4.453125000614517326, 4.541064518000418104, -2.621784821874998173 ) ) ;
#18263 = CARTESIAN_POINT ( 'NONE',  ( 8.784375000614518925, -4.541064518000419881, 2.621784821874995952 ) ) ;
#18264 = CARTESIAN_POINT ( 'NONE',  ( 0.000000000000000000, 0.000000000000000000, 0.000000000000000000 ) ) ;
#18265 = CARTESIAN_POINT ( 'NONE',  ( 17.10000000122903430, -2.886751345948129988, 4.999999999999997335 ) ) ;
#18266 = CARTESIAN_POINT ( 'NONE',  ( 5.109375000614518214, 0.000000000000000000, 5.243569643749999010 ) ) ;
#18267 = CARTESIAN_POINT ( 'NONE',  ( 8.015625000614518214, 3.027376345333613106, -5.243569643749998122 ) ) ;
#18268 = CARTESIAN_POINT ( 'NONE',  ( -4.000000000000000000, 13.56874999877096677, 30.00000000000000000 ) ) ;
#18269 = CARTESIAN_POINT ( 'NONE',  ( 23.41875000122903216, -5.773502691896255534, -1.060575238724906372E-15 ) ) ;
#18270 = CARTESIAN_POINT ( 'NONE',  ( 17.14687500061451786, 6.054752690667223547, 3.707466751127219781E-16 ) ) ;
#18271 = ORIENTED_EDGE ( 'NONE', *, *, #54489, .F. ) ;
#18272 = CARTESIAN_POINT ( 'NONE',  ( 24.59062500061451573, -3.027376345333610441, -5.243569643749999898 ) ) ;
#18273 = CARTESIAN_POINT ( 'NONE',  ( 9.515625000614518214, 3.027376345333611329, 5.243569643749999010 ) ) ;
#18274 = CARTESIAN_POINT ( 'NONE',  ( 28.09687500061451715, -3.027376345333614438, 5.243569643749998122 ) ) ;
#18275 = CARTESIAN_POINT ( 'NONE',  ( 11.16562500061451679, 3.027376345333613106, -5.243569643749998122 ) ) ;
#18276 = CARTESIAN_POINT ( 'NONE',  ( 25.44375000122903074, 5.773502691896255534, 3.535250795749688401E-16 ) ) ;
#18277 = CARTESIAN_POINT ( 'NONE',  ( 10.68750000122903288, 4.330127018922191873, 2.499999999999999556 ) ) ;
#18278 = CARTESIAN_POINT ( 'NONE',  ( 25.15312500061451217, 4.541064518000418104, -2.621784821874998173 ) ) ;
#18279 = CARTESIAN_POINT ( 'NONE',  ( -2.121784821874999949, 13.87812500061451715, -33.67503911421598417 ) ) ;
#18280 = CARTESIAN_POINT ( 'NONE',  ( 13.27500000122903323, 2.886751345948129099, -4.999999999999998224 ) ) ;
#18281 = CARTESIAN_POINT ( 'NONE',  ( 23.05312500061451431, 0.000000000000000000, 5.243569643749999010 ) ) ;
#18282 = VECTOR ( 'NONE', #35359, 1000.000000000000000 ) ;
#18283 = CARTESIAN_POINT ( 'NONE',  ( 11.40000000000000036, 4.330127018922192761, -2.499999999999997780 ) ) ;
#18284 = CARTESIAN_POINT ( 'NONE',  ( 19.41562500061451146, 3.027376345333611329, 5.243569643749999010 ) ) ;
#18285 = CARTESIAN_POINT ( 'NONE',  ( 5.559375000614517504, 0.000000000000000000, 5.243569643749999010 ) ) ;
#18286 = EDGE_CURVE ( 'NONE', #25347, #55385, #33884, .T. ) ;
#18287 = CARTESIAN_POINT ( 'NONE',  ( 21.71249999999999858, 2.886751345948129099, -4.999999999999998224 ) ) ;
#18288 = CARTESIAN_POINT ( 'NONE',  ( 7.387500001229032165, 6.123233995736764310E-16, -4.999999999999998224 ) ) ;
#18289 = CARTESIAN_POINT ( 'NONE',  ( 15.56250000122903465, 4.330127018922192761, -2.499999999999997780 ) ) ;
#18290 = CARTESIAN_POINT ( 'NONE',  ( 11.72812500061451857, 4.541064518000418104, 2.621784821874999949 ) ) ;
#18291 = CARTESIAN_POINT ( 'NONE',  ( 14.72812500061451679, 6.421520780324663323E-16, -5.243569643749999010 ) ) ;
#18292 = VECTOR ( 'NONE', #54507, 1000.000000000000000 ) ;
#18293 = CARTESIAN_POINT ( 'NONE',  ( 26.47500000122903074, 2.886751345948126879, 4.999999999999999112 ) ) ;
#18294 = CARTESIAN_POINT ( 'NONE',  ( 19.42499999999999716, 6.123233995736764310E-16, -4.999999999999998224 ) ) ;
#18295 = AXIS2_PLACEMENT_3D ( 'NONE', #25697, #46779, #69314 ) ;
#18296 = CARTESIAN_POINT ( 'NONE',  ( 22.65937500061451715, 0.000000000000000000, 5.243569643749999010 ) ) ;
#18297 = CARTESIAN_POINT ( 'NONE',  ( 22.40625000122903288, 0.000000000000000000, 4.999999999999998224 ) ) ;
#18298 = CARTESIAN_POINT ( 'NONE',  ( 10.87500000122903288, -5.773502691896255534, -1.060575238724906372E-15 ) ) ;
#18299 = CARTESIAN_POINT ( 'NONE',  ( 8.709375000614517859, 0.000000000000000000, 5.243569643749999010 ) ) ;
#18300 = CARTESIAN_POINT ( 'NONE',  ( 24.57187500061451502, -6.054752690667223547, -1.112240025338166033E-15 ) ) ;
#18301 = CARTESIAN_POINT ( 'NONE',  ( 3.496875000614518836, -3.027376345333610441, -5.243569643749999898 ) ) ;
#18302 = CARTESIAN_POINT ( 'NONE',  ( 21.06562500061451715, 3.027376345333613106, -5.243569643749998122 ) ) ;
#18303 = CARTESIAN_POINT ( 'NONE',  ( 26.93437500061451573, 6.421520780324663323E-16, -5.243569643749999010 ) ) ;
#18304 = CARTESIAN_POINT ( 'NONE',  ( -3.756430356250000102, 16.12812499938548427, 30.00000000000000000 ) ) ;
#18305 = CARTESIAN_POINT ( 'NONE',  ( 18.67500000000000071, 4.330127018922191873, 2.499999999999999556 ) ) ;
#18306 = CARTESIAN_POINT ( 'NONE',  ( 7.696875000614516793, 6.054752690667223547, 3.707466751127219781E-16 ) ) ;
#18307 = CARTESIAN_POINT ( 'NONE',  ( 20.31562500061451715, 3.027376345333611329, 5.243569643749999010 ) ) ;
#18308 = ORIENTED_EDGE ( 'NONE', *, *, #28846, .F. ) ;
#18309 = CARTESIAN_POINT ( 'NONE',  ( 25.05000000000000071, 0.000000000000000000, 4.999999999999998224 ) ) ;
#18310 = CARTESIAN_POINT ( 'NONE',  ( 27.21562500061451928, -6.054752690667223547, -1.112240025338166033E-15 ) ) ;
#18311 = CARTESIAN_POINT ( 'NONE',  ( 3.346875000614518036, -3.027376345333614438, 5.243569643749998122 ) ) ;
#18312 = CARTESIAN_POINT ( 'NONE',  ( 45.00000000000000000, 0.000000000000000000, 0.000000000000000000 ) ) ;
#18313 = CYLINDRICAL_SURFACE ( 'NONE', #1708, 3.999999999999996447 ) ;
#18314 = CARTESIAN_POINT ( 'NONE',  ( 16.57499999999999929, -4.330127018922194537, 2.499999999999995559 ) ) ;
#18315 = CARTESIAN_POINT ( 'NONE',  ( 22.04062500061451502, 6.054752690667223547, 3.707466751127219781E-16 ) ) ;
#18316 = VERTEX_POINT ( 'NONE', #61596 ) ;
#18317 = CARTESIAN_POINT ( 'NONE',  ( 25.94999999999999929, 0.000000000000000000, 4.999999999999998224 ) ) ;
#18318 = CARTESIAN_POINT ( 'NONE',  ( 25.95937500061451431, -4.541064518000417216, -2.621784821875001281 ) ) ;
#18319 = ORIENTED_EDGE ( 'NONE', *, *, #14004, .F. ) ;
#18320 = CARTESIAN_POINT ( 'NONE',  ( 16.37812500061451715, -4.541064518000419881, 2.621784821874995952 ) ) ;
#18321 = CARTESIAN_POINT ( 'NONE',  ( 5.165625000614518569, -6.054752690667223547, -1.112240025338166033E-15 ) ) ;
#18322 = CARTESIAN_POINT ( 'NONE',  ( 19.24687500061451573, 4.119189519843966529, -2.378215178124998275 ) ) ;
#18323 = CARTESIAN_POINT ( 'NONE',  ( 29.16562500061451502, 3.027376345333613106, -5.243569643749998122 ) ) ;
#18324 = CARTESIAN_POINT ( 'NONE',  ( 15.33750000122903323, -4.330127018922194537, 2.499999999999995559 ) ) ;
#18325 = VECTOR ( 'NONE', #51264, 1000.000000000000000 ) ;
#18326 = CARTESIAN_POINT ( 'NONE',  ( 22.87500000000000000, -4.330127018922194537, 2.499999999999995559 ) ) ;
#18327 = CARTESIAN_POINT ( 'NONE',  ( 28.94999999999999929, 4.330127018922192761, -2.499999999999997780 ) ) ;
#18328 = CARTESIAN_POINT ( 'NONE',  ( 4.771875000614516971, -6.054752690667223547, -1.112240025338166033E-15 ) ) ;
#18329 = CARTESIAN_POINT ( 'NONE',  ( 10.20937500061451786, -4.541064518000417216, -2.621784821875001281 ) ) ;
#18330 = CARTESIAN_POINT ( 'NONE',  ( 18.79687500061451644, -3.027376345333610441, -5.243569643749999898 ) ) ;
#18331 = CARTESIAN_POINT ( 'NONE',  ( 9.937500001229032875, -4.330127018922194537, 2.499999999999995559 ) ) ;
#18332 = ORIENTED_EDGE ( 'NONE', *, *, #67527, .T. ) ;
#18333 = CARTESIAN_POINT ( 'NONE',  ( 28.60312500061451502, -4.541064518000417216, -2.621784821875001281 ) ) ;
#18334 = CARTESIAN_POINT ( 'NONE',  ( 3.675000000000001155, 6.123233995736764310E-16, -4.999999999999998224 ) ) ;
#18335 = CARTESIAN_POINT ( 'NONE',  ( 4.921875000614518214, 3.027376345333613106, -5.243569643749998122 ) ) ;
#18336 = CARTESIAN_POINT ( 'NONE',  ( 18.22499999999999787, 4.330127018922191873, 2.499999999999999556 ) ) ;
#18337 = CARTESIAN_POINT ( 'NONE',  ( 17.12812500061451715, 4.541064518000418104, 2.621784821874999949 ) ) ;
#18338 = CARTESIAN_POINT ( 'NONE',  ( 2.000000000000000444, 19.77500000000000213, 26.53589838486224650 ) ) ;
#18339 = DIRECTION ( 'NONE',  ( 0.000000000000000000, 0.000000000000000000, -1.000000000000000000 ) ) ;
#18340 = CARTESIAN_POINT ( 'NONE',  ( 19.43437500061451928, 4.119189519843966529, 2.378215178124999607 ) ) ;
#18341 = CARTESIAN_POINT ( 'NONE',  ( 7.378125000614518036, -4.541064518000419881, 2.621784821874995952 ) ) ;
#18342 = CARTESIAN_POINT ( 'NONE',  ( 26.29687500061451644, -3.027376345333614438, 5.243569643749998122 ) ) ;
#18343 = CARTESIAN_POINT ( 'NONE',  ( 4.243569643749999010, 18.77187500061451786, 27.54997392385601174 ) ) ;
#18344 = CARTESIAN_POINT ( 'NONE',  ( 26.29687500061451644, -3.027376345333614438, 5.243569643749998122 ) ) ;
#18345 = CARTESIAN_POINT ( 'NONE',  ( 7.200000000000001954, -4.330127018922190985, -2.500000000000001332 ) ) ;
#18346 = CARTESIAN_POINT ( 'NONE',  ( -2.828200636599751609E-16, 13.70000000122903572, 25.38119784648299770 ) ) ;
#18347 = CARTESIAN_POINT ( 'NONE',  ( 15.21562500061451750, 3.027376345333613106, -5.243569643749998122 ) ) ;
#18348 = CARTESIAN_POINT ( 'NONE',  ( 6.600000001229032520, 5.773502691896255534, 3.535250795749688894E-16 ) ) ;
#18349 = EDGE_CURVE ( 'NONE', #47876, #19994, #10278, .T. ) ;
#18350 = VECTOR ( 'NONE', #65848, 1000.000000000000000 ) ;
#18351 = CARTESIAN_POINT ( 'NONE',  ( 18.12187500061451573, 3.027376345333611329, 5.243569643749999010 ) ) ;
#18352 = CARTESIAN_POINT ( 'NONE',  ( 12.23437500061451821, 4.541064518000418104, 2.621784821874999949 ) ) ;
#18353 = CARTESIAN_POINT ( 'NONE',  ( -3.999828644916963327, 3.000228472979579841, -29.85654714282670952 ) ) ;
#18354 = ORIENTED_EDGE ( 'NONE', *, *, #44062, .T. ) ;
#18355 = CARTESIAN_POINT ( 'NONE',  ( 12.06562500061451537, 3.027376345333613106, -5.243569643749998122 ) ) ;
#18356 = AXIS2_PLACEMENT_3D ( 'NONE', #61775, #51425, #38898 ) ;
#18357 = FACE_BOUND ( 'NONE', #36376, .T. ) ;
#18358 = CARTESIAN_POINT ( 'NONE',  ( 24.18750000122903288, 4.330127018922191873, 2.499999999999999556 ) ) ;
#18359 = CARTESIAN_POINT ( 'NONE',  ( 13.69687500061451679, -3.027376345333614438, 5.243569643749998122 ) ) ;
#18360 = CARTESIAN_POINT ( 'NONE',  ( 28.87499999999999645, 6.123233995736764310E-16, -4.999999999999998224 ) ) ;
#18361 = CARTESIAN_POINT ( 'NONE',  ( 14.24062500061451608, -3.027376345333610441, -5.243569643749999898 ) ) ;
#18362 = EDGE_CURVE ( 'NONE', #32246, #5287, #46062, .T. ) ;
#18363 = CARTESIAN_POINT ( 'NONE',  ( 3.999999999999998668, 18.91249999999999787, -32.30940107675850470 ) ) ;
#18364 = CARTESIAN_POINT ( 'NONE',  ( 23.55937500061451573, 0.000000000000000000, 5.243569643749999010 ) ) ;
#18365 = DIRECTION ( 'NONE',  ( -1.000000000000000000, -0.000000000000000000, -0.000000000000000000 ) ) ;
#18366 = CARTESIAN_POINT ( 'NONE',  ( 11.70000000122903216, -2.886751345948129988, 4.999999999999997335 ) ) ;
#18367 = CYLINDRICAL_SURFACE ( 'NONE', #35112, 4.999999999999998224 ) ;
#18368 = CARTESIAN_POINT ( 'NONE',  ( -3.999999999999999112, 19.51250000000000284, 27.69059892324149885 ) ) ;
#18369 = CARTESIAN_POINT ( 'NONE',  ( -4.243569643749999898, 17.60937500061451999, -30.00000000000000000 ) ) ;
#18370 =( BOUNDED_CURVE ( )  B_SPLINE_CURVE ( 2, ( #38662, #32377, #60438, #27211, #54917, #49746, #59711 ),
 .UNSPECIFIED., .F., .F. ) 
 B_SPLINE_CURVE_WITH_KNOTS ( ( 3, 2, 2, 3 ),
 ( 0.1900000000000000855, 0.1933333333333333848, 0.1966666666666667118, 0.2000000000000000389 ),
 .UNSPECIFIED. ) 
 CURVE ( )  GEOMETRIC_REPRESENTATION_ITEM ( )  RATIONAL_B_SPLINE_CURVE ( ( 0.9999999999999966693, 0.8660254037844420383, 1.000000000000000000, 0.8660254037844387076, 1.000000000000000000, 0.8660254037844375974, 1.000000000000001110 ) ) 
 REPRESENTATION_ITEM ( '' )  );
#18371 = EDGE_CURVE ( 'NONE', #38724, #1846, #55340, .T. ) ;
#18372 = CARTESIAN_POINT ( 'NONE',  ( 19.02187500061451786, 3.027376345333611329, 5.243569643749999010 ) ) ;
#18373 = CARTESIAN_POINT ( 'NONE',  ( 17.21250000122903145, -4.330127018922190985, -2.500000000000001332 ) ) ;
#18374 = CARTESIAN_POINT ( 'NONE',  ( 15.08437500061451786, -4.541064518000419881, 2.621784821874995952 ) ) ;
#18375 = CARTESIAN_POINT ( 'NONE',  ( -4.243569643749999898, 10.82187500061451857, 27.54997392385601529 ) ) ;
#18376 = CARTESIAN_POINT ( 'NONE',  ( 21.11250000122903359, 0.000000000000000000, 4.999999999999998224 ) ) ;
#18377 = CARTESIAN_POINT ( 'NONE',  ( 15.40312500061451573, 0.000000000000000000, 5.243569643749999010 ) ) ;
#18378 = VERTEX_POINT ( 'NONE', #28349 ) ;
#18379 = VERTEX_POINT ( 'NONE', #49802 ) ;
#18380 = CARTESIAN_POINT ( 'NONE',  ( 18.52499999999999858, 6.123233995736764310E-16, -4.999999999999998224 ) ) ;
#18381 = FACE_OUTER_BOUND ( 'NONE', #52604, .T. ) ;
#18382 = CARTESIAN_POINT ( 'NONE',  ( 22.34999999999999787, 0.000000000000000000, 4.999999999999998224 ) ) ;
#18383 = CARTESIAN_POINT ( 'NONE',  ( 13.95000000122903572, -2.886751345948129988, 4.999999999999997335 ) ) ;
#18384 = CARTESIAN_POINT ( 'NONE',  ( 27.45937500061451786, 4.541064518000418104, -2.621784821874998173 ) ) ;
#18385 = CARTESIAN_POINT ( 'NONE',  ( 19.34062500061451573, 6.054752690667223547, 3.707466751127219781E-16 ) ) ;
#18386 = CARTESIAN_POINT ( 'NONE',  ( 22.86562500061451431, 3.027376345333613106, -5.243569643749998122 ) ) ;
#18387 = CARTESIAN_POINT ( 'NONE',  ( 4.340625000614515727, -3.027376345333610441, -5.243569643749999898 ) ) ;
#18388 = CARTESIAN_POINT ( 'NONE',  ( 26.39999999999999858, 0.000000000000000000, 4.999999999999998224 ) ) ;
#18389 = CARTESIAN_POINT ( 'NONE',  ( 8.034375000614518925, 5.824947211148865298E-16, -4.756430356249998326 ) ) ;
#18390 = CARTESIAN_POINT ( 'NONE',  ( 0.000000000000000000, 20.00000000000000000, 30.00000000000000000 ) ) ;
#18391 = CARTESIAN_POINT ( 'NONE',  ( 20.15625000122903288, 0.000000000000000000, 4.999999999999998224 ) ) ;
#18392 = CARTESIAN_POINT ( 'NONE',  ( 2.121784821875001281, 15.95937500061451608, -26.32496088578401938 ) ) ;
#18393 = EDGE_CURVE ( 'NONE', #36225, #19466, #19078, .T. ) ;
#18394 = CARTESIAN_POINT ( 'NONE',  ( 5.362500001229033586, 0.000000000000000000, 4.999999999999998224 ) ) ;
#18395 = CARTESIAN_POINT ( 'NONE',  ( 6.787500000000001421, -2.886751345948125991, -5.000000000000000000 ) ) ;
#18396 = CARTESIAN_POINT ( 'NONE',  ( 16.31249999999999645, 2.886751345948062486, -5.000000000000113687 ) ) ;
#18397 = CARTESIAN_POINT ( 'NONE',  ( 9.459375000614517859, 4.541064518000418104, -2.621784821874998173 ) ) ;
#18398 = CARTESIAN_POINT ( 'NONE',  ( 28.11562500061451431, -6.054752690667223547, -1.112240025338166033E-15 ) ) ;
#18399 = CARTESIAN_POINT ( 'NONE',  ( 27.56250000122902932, -4.330127018922190985, -2.500000000000001332 ) ) ;
#18400 = CARTESIAN_POINT ( 'NONE',  ( 45.00000000000000000, 0.000000000000000000, 4.999999999999998224 ) ) ;
#18401 = CARTESIAN_POINT ( 'NONE',  ( 10.00000000000000000, 1.224646799147353256E-15, -50.00000000000000000 ) ) ;
#18402 = CARTESIAN_POINT ( 'NONE',  ( 8.371875000614515727, -6.054752690667223547, -1.112240025338166033E-15 ) ) ;
#18403 = CARTESIAN_POINT ( 'NONE',  ( 10.24687500061451750, -3.027376345333610441, -5.243569643749999898 ) ) ;
#18404 = CARTESIAN_POINT ( 'NONE',  ( 5.625000000000001776, 4.330127018922191873, 2.499999999999999556 ) ) ;
#18405 =( BOUNDED_CURVE ( )  B_SPLINE_CURVE ( 2, ( #23258, #34341, #16625, #39179, #50270, #55804, #67619 ),
 .UNSPECIFIED., .F., .F. ) 
 B_SPLINE_CURVE_WITH_KNOTS ( ( 3, 2, 2, 3 ),
 ( 0.5333333333333334370, 0.5361111111111112049, 0.5388888888888888618, 0.5416666666666666297 ),
 .UNSPECIFIED. ) 
 CURVE ( )  GEOMETRIC_REPRESENTATION_ITEM ( )  RATIONAL_B_SPLINE_CURVE ( ( 0.9999999999999946709, 0.8660254037844440367, 1.000000000000000000, 0.8660254037844387076, 1.000000000000000000, 0.8660254037844387076, 1.000000000000000000 ) ) 
 REPRESENTATION_ITEM ( '' )  );
#18406 = CARTESIAN_POINT ( 'NONE',  ( 2.121784821874999061, 15.60312500061459495, 26.32496088578401583 ) ) ;
#18407 = CARTESIAN_POINT ( 'NONE',  ( 4.949999999999999289, -4.330127018922190985, -2.500000000000001332 ) ) ;
#18408 = CARTESIAN_POINT ( 'NONE',  ( 6.675000000000000711, -4.330127018922194537, 2.499999999999995559 ) ) ;
#18409 = CARTESIAN_POINT ( 'NONE',  ( 26.85000000122903430, 5.773502691896255534, 3.535250795749688894E-16 ) ) ;
#18410 = CARTESIAN_POINT ( 'NONE',  ( 18.87187500061451573, 4.119189519843966529, 2.378215178124999607 ) ) ;
#18411 = CARTESIAN_POINT ( 'NONE',  ( 23.87812500061451715, 4.541064518000418104, 2.621784821874999949 ) ) ;
#18412 = CARTESIAN_POINT ( 'NONE',  ( 13.19062500061451537, -3.027376345333614438, 5.243569643749998122 ) ) ;
#18413 = CARTESIAN_POINT ( 'NONE',  ( 25.99687500061451573, 4.119189519843966529, -2.378215178124998275 ) ) ;
#18414 = CARTESIAN_POINT ( 'NONE',  ( 9.346875000614517148, -3.027376345333610441, -5.243569643749999898 ) ) ;
#18415 = CARTESIAN_POINT ( 'NONE',  ( 25.34999999999999787, 4.330127018922192761, -2.499999999999997780 ) ) ;
#18416 = CARTESIAN_POINT ( 'NONE',  ( 22.08750000122903501, -4.330127018922194537, 2.499999999999995559 ) ) ;
#18417 = CARTESIAN_POINT ( 'NONE',  ( 0.000000000000000000, 20.00000000000000000, 30.00000000000000000 ) ) ;
#18418 = CARTESIAN_POINT ( 'NONE',  ( 12.04687500061451821, -3.027376345333610441, -5.243569643749999898 ) ) ;
#18419 = CARTESIAN_POINT ( 'NONE',  ( 26.93437500061451573, 6.421520780324663323E-16, -5.243569643749999010 ) ) ;
#18420 = CARTESIAN_POINT ( 'NONE',  ( 3.459375000614519635, -4.541064518000417216, -2.621784821875001281 ) ) ;
#18421 = CARTESIAN_POINT ( 'NONE',  ( 2.000000000000001332, 13.51250000122903394, -26.53589838486224650 ) ) ;
#18422 = CARTESIAN_POINT ( 'NONE',  ( 21.42187500061451644, -6.054752690667223547, -1.112240025338166033E-15 ) ) ;
#18423 = CARTESIAN_POINT ( 'NONE',  ( 12.27187500061451786, 3.027376345333611329, 5.243569643749999010 ) ) ;
#18424 = CARTESIAN_POINT ( 'NONE',  ( -3.756430356250000102, 18.82812499938548356, 30.00000000000000000 ) ) ;
#18425 = CARTESIAN_POINT ( 'NONE',  ( 24.86250000000000071, 2.886751345948129099, -4.999999999999998224 ) ) ;
#18426 = CARTESIAN_POINT ( 'NONE',  ( -2.000000000000001776, 13.25000000000000178, 33.46410161513775705 ) ) ;
#18427 = CARTESIAN_POINT ( 'NONE',  ( 4.243569643749999898, 14.19687500061451857, -27.54997392385601529 ) ) ;
#18428 = CARTESIAN_POINT ( 'NONE',  ( 26.67187500061451644, 2.746126346562643317, 4.756430356249998326 ) ) ;
#18429 = CARTESIAN_POINT ( 'NONE',  ( 18.17812500061451786, -4.541064518000419881, 2.621784821874995952 ) ) ;
#18430 = CARTESIAN_POINT ( 'NONE',  ( 8.025000000000000355, -4.330127018922194537, 2.499999999999995559 ) ) ;
#18431 = CARTESIAN_POINT ( 'NONE',  ( 45.00000000000000000, -4.500000000000000000, -5.500000000000000000 ) ) ;
#18432 = CARTESIAN_POINT ( 'NONE',  ( 14.73749999999999893, -2.886751345948129988, 4.999999999999997335 ) ) ;
#18433 = CARTESIAN_POINT ( 'NONE',  ( 3.999999999999999112, 19.43750000122903288, 30.00000000000000000 ) ) ;
#18435 =( BOUNDED_CURVE ( )  B_SPLINE_CURVE ( 2, ( #56029, #66758, #66382, #54935, #50127, #44597, #49397 ),
 .UNSPECIFIED., .F., .F. ) 
 B_SPLINE_CURVE_WITH_KNOTS ( ( 3, 2, 2, 3 ),
 ( 0.7000000000000001776, 0.7033333333333335879, 0.7066666666666668872, 0.7100000000000001865 ),
 .UNSPECIFIED. ) 
 CURVE ( )  GEOMETRIC_REPRESENTATION_ITEM ( )  RATIONAL_B_SPLINE_CURVE ( ( 0.9999999999999911182, 0.8660254037844475894, 1.000000000000000000, 0.8660254037844387076, 1.000000000000000000, 0.8660254037844298258, 1.000000000000008882 ) ) 
 REPRESENTATION_ITEM ( '' )  );
#18434 = CARTESIAN_POINT ( 'NONE',  ( 14.10000000122903252, -2.886751345948125991, -5.000000000000000000 ) ) ;
#18436 = CARTESIAN_POINT ( 'NONE',  ( 25.73437500061451644, 4.541064518000418104, 2.621784821874999949 ) ) ;
#18437 = AXIS2_PLACEMENT_3D ( 'NONE', #21854, #67663, #62111 ) ;
#18438 = EDGE_LOOP ( 'NONE', ( #56265, #35247, #17959, #18604 ) ) ;
#18439 = CARTESIAN_POINT ( 'NONE',  ( 18.81562500061452070, 3.027376345333613106, -5.243569643749998122 ) ) ;
#18440 = CARTESIAN_POINT ( 'NONE',  ( 21.19687500061451502, 6.054752690667223547, 3.707466751127219781E-16 ) ) ;
#18441 = CARTESIAN_POINT ( 'NONE',  ( 3.037500000000002309, -2.886751345948129988, 4.999999999999997335 ) ) ;
#18442 = CARTESIAN_POINT ( 'NONE',  ( 7.790625000614518569, -3.027376345333614438, 5.243569643749998122 ) ) ;
#18443 = CARTESIAN_POINT ( 'NONE',  ( 21.25312500061451715, 0.000000000000000000, 5.243569643749999010 ) ) ;
#18444 = CARTESIAN_POINT ( 'NONE',  ( 12.60937500061451821, 4.541064518000418104, -2.621784821874998173 ) ) ;
#18445 = CARTESIAN_POINT ( 'NONE',  ( 16.54687500061451644, -3.027376345333610441, -5.243569643749999898 ) ) ;
#18446 = CARTESIAN_POINT ( 'NONE',  ( 4.243569643749999010, 14.21562500061451928, 27.54997392385601174 ) ) ;
#18447 = CARTESIAN_POINT ( 'NONE',  ( 18.75000000122903288, 5.773502691896255534, 3.535250795749688894E-16 ) ) ;
#18448 = CARTESIAN_POINT ( 'NONE',  ( 14.70937500061451786, -4.119189519843965641, -2.378215178125001383 ) ) ;
#18449 = CARTESIAN_POINT ( 'NONE',  ( 9.290625000614515017, -3.027376345333610441, -5.243569643749999898 ) ) ;
#18450 = CARTESIAN_POINT ( 'NONE',  ( 3.496875000614518836, -3.027376345333610441, -5.243569643749999898 ) ) ;
#18451 = CARTESIAN_POINT ( 'NONE',  ( 29.69062500061451715, 6.054752690667223547, 3.707466751127219781E-16 ) ) ;
#18452 = EDGE_CURVE ( 'NONE', #16648, #36225, #44636, .T. ) ;
#18453 = CARTESIAN_POINT ( 'NONE',  ( 24.90937500061451715, 0.000000000000000000, 5.243569643749999010 ) ) ;
#18454 = CARTESIAN_POINT ( 'NONE',  ( 17.16562500061451502, 3.027376345333611329, 5.243569643749999010 ) ) ;
#18455 = CARTESIAN_POINT ( 'NONE',  ( 24.18750000122903288, 4.330127018922191873, 2.499999999999999556 ) ) ;
#18456 = CARTESIAN_POINT ( 'NONE',  ( 25.30312500061451431, 0.000000000000000000, 5.243569643749999010 ) ) ;
#18457 = CARTESIAN_POINT ( 'NONE',  ( 22.28437500061451715, -4.541064518000419881, 2.621784821874995952 ) ) ;
#18458 = CARTESIAN_POINT ( 'NONE',  ( 16.67812500061451786, 4.541064518000418104, 2.621784821874999949 ) ) ;
#18459 = CARTESIAN_POINT ( 'NONE',  ( -3.000416591977282496E-16, 17.94687500061451502, 25.09994784771203058 ) ) ;
#18460 =( BOUNDED_SURFACE ( )  B_SPLINE_SURFACE ( 1, 2, ( 
 ( #36083, #63060, #57522, #69706, #64148, #41274, #1752, #70063, #23537, #19437, #12463, #46814, #58236, #19072, #13174, #69352, #68986, #13535, #30545, #46087, #64518, #34993, #1031, #18709, #58603, #8010, #13911, #36450, #29453, #18343, #63785, #51990, #7641, #1391, #23900, #12817, #46448, #29814, #40918, #63430, #57875, #7285, #19810, #26466, #37543, #49372, #32006, #70796, #42363, #60798, #71536, #2833, #64885, #30901, #9108, #31646, #3943, #71902, #54905, #14273, #71161, #20911, #3575, #20171, #37176, #36811, #25735, #20534, #54178, #49005, #8737, #60065, #26098, #43463, #53443, #15731, #47906, #43090, #48636, #65618, #43829, #15006, #59326, #31270, #53812, #4313, #9476, #54541, #38270, #9838, #3206, #70435, #48272, #25361, #65987, #42725, #15368, #37909, #65246, #60427, #14635, #59701, #21275, #32367, #26838, #66353, #72629, #72263, #5755, #45647, #68181, #17543, #61896, #50463, #39377, #50820, #67460, #16100, #27930, #40105, #5030, #10569, #11301, #38650, #56711, #33821, #34175, #22372, #10204, #4671, #5392, #28289, #72991, #55999, #32739, #55276, #50098, #21640, #67815, #17188, #23090, #223, #22728, #27201, #49736, #22013, #56365, #44924, #16823, #44198, #28643, #61174, #45281, #66729, #39748, #62264, #11660, #55636, #33097, #44569, #67099, #27567, #16457, #39015, #6112, #61530, #10928, #33455, #51181, #585, #46363, #47710, #8192, #20357, #25169, #51547, #65067, #68897, #62619, #64333, #70249, #948, #57434, #23456, #19621, #46001, #23812, #3016, #29372, #42177, #68538, #18254, #25546, #51904, #31084, #36267, #1302, #40827, #17899, #6837, #30719, #13726, #59148, #40459, #64703, #58782, #53624, #12015, #48458, #6475, #53252, #2650, #14087, #3397, #36627, #62975, #12371, #34906, #14458, #8557, #48089, #70982, #42541, #70614, #29010, #19988, #34538, #36992, #59514, #8928, #31458, #54000, #25918, #57068, #72812, #33281, #21095, #72440, #66914, #32192, #31826, #38463, #21458, #26657, #16282, #60244, #55094, #65432, #32557, #4850, #27384, #4128, #15185, #43646, #4494, #60989, #55820, #10388, #54364, #32920, #49555, #61353, #44013, #9658, #3759, #42908, #55457, #14822, #26283, #37365, #66170 ),
 ( #10021, #49916, #20725, #27023, #60612, #21824, #44389, #48820, #71350, #72076, #43283, #66535, #10749, #15915, #71723, #38838, #5208, #65804, #37724, #54725, #59887, #49192, #27749, #15546, #50288, #9293, #38089, #12555, #763, #16642, #67635, #17002, #28114, #50643, #28464, #68720, #17718, #40278, #62799, #45463, #62084, #7018, #12192, #51725, #40641, #39559, #44749, #57615, #11837, #5930, #67995, #68357, #39197, #61712, #34356, #397, #17368, #22904, #23635, #47, #67283, #56888, #22552, #51360, #22195, #39925, #6662, #11111, #45100, #34719, #57249, #6293, #62439, #63160, #33640, #46181, #56184, #28822, #23271, #29191, #45821, #1126, #11477, #18080, #35089, #5577, #29549, #34000, #56537, #52085, #50999, #8468, #53168, #58329, #48005, #18804, #13636, #23996, #64248, #36543, #59063, #35807, #46908, #52808, #36180, #19538, #14374, #70161, #63526, #42096, #8108, #19908, #2565, #41368, #12913, #31373, #64618, #46544, #35446, #1490, #2209, #24724, #47628, #42461, #25461, #57970, #41721, #31003, #2932, #58698, #14005, #52448, #30636, #19167, #53536, #70533, #7377, #29908, #25085, #1854, #64983, #36909, #59429, #30276, #8837, #69085, #24361, #69447, #63878, #18446, #7740, #41011, #47267, #13269, #69801, #43928, #44300, #32473, #48371, #26197, #48736, #59800, #9206, #60162, #27300, #49466, #70898, #49107, #71999, #71636, #26567, #10666, #16201, #20639, #42822, #38376, #60900, #66829, #66454, #21374, #20270, #25834, #65717, #26941, #43561, #21009, #61273, #72358, #31741, #15831, #37278, #10303, #55006, #15461, #71259, #65346, #15103, #43197, #54279, #14736, #9572, #38006, #53914, #3307, #37639, #32104, #66083, #54637, #60528, #9935, #3673, #4412, #4042, #55373, #32836, #4767, #49834, #21739, #38752, #28032, #44668, #39846, #67198, #67555, #45744, #73088, #683, #5850, #22469, #39473, #39111, #50561, #317, #11396, #28740, #11029, #62360, #56459, #23190, #63080, #18003, #50202, #22826, #33916, #28381, #46103, #50919, #16560, #61627, #33552, #57169, #67914, #11756, #40561, #12116, #56102, #72727, #5493, #33196, #17285, #45020, #51280, #68279, #16918, #45378, #61996, #55735, #23555, #34274, #62723, #6581 ) ),
 .UNSPECIFIED., .F., .F., .F. ) 
 B_SPLINE_SURFACE_WITH_KNOTS ( ( 2, 2 ),
 ( 3, 2, 2, 2, 2, 2, 2, 2, 2, 2, 2, 2, 2, 2, 2, 2, 2, 2, 2, 2, 2, 2, 2, 2, 2, 2, 2, 2, 2, 2, 2, 2, 2, 2, 2, 2, 2, 2, 2, 2, 2, 2, 2, 2, 2, 2, 2, 2, 2, 2, 2, 2, 2, 2, 2, 2, 2, 2, 2, 2, 2, 2, 2, 2, 2, 2, 2, 2, 2, 2, 2, 2, 2, 2, 2, 2, 2, 2, 2, 2, 2, 2, 2, 2, 2, 2, 2, 2, 2, 2, 2, 2, 2, 2, 2, 2, 2, 2, 2, 2, 2, 2, 2, 2, 2, 2, 2, 2, 2, 2, 2, 2, 2, 2, 2, 2, 2, 2, 2, 2, 2, 2, 2, 2, 2, 2, 2, 2, 2, 2, 2, 2, 2, 2, 2, 3 ),
 ( 0.000000000000000000, 1.000000000000000000 ),
 ( 0.000000000000000000, 0.007246376811594202987, 0.01449275362318840597, 0.02173913043478260809, 0.02898550724637681195, 0.03623188405797101580, 0.04347826086956521618, 0.05072463768115942351, 0.05797101449275362389, 0.06521739130434782428, 0.07246376811594203160, 0.07971014492753622505, 0.08695652173913043237, 0.09420289855072463969, 0.1014492753623188470, 0.1086956521739130405, 0.1159420289855072478, 0.1231884057971014551, 0.1304347826086956486, 0.1376811594202898559, 0.1449275362318840632, 0.1521739130434782705, 0.1594202898550724501, 0.1666666666666666574, 0.1739130434782608647, 0.1811594202898550721, 0.1884057971014492794, 0.1956521739130434867, 0.2028985507246376940, 0.2101449275362318736, 0.2173913043478260809, 0.2246376811594202882, 0.2318840579710144956, 0.2391304347826087029, 0.2463768115942029102, 0.2536231884057971175, 0.2608695652173912971, 0.2681159420289855322, 0.2753623188405797118, 0.2826086956521738913, 0.2898550724637681264, 0.2971014492753623060, 0.3043478260869565410, 0.3115942028985507206, 0.3188405797101449002, 0.3260869565217391353, 0.3333333333333333148, 0.3405797101449275499, 0.3478260869565217295, 0.3550724637681159646, 0.3623188405797101441, 0.3695652173913043237, 0.3768115942028985588, 0.3840579710144927383, 0.3913043478260869734, 0.3985507246376811530, 0.4057971014492753881, 0.4130434782608695676, 0.4202898550724637472, 0.4275362318840579823, 0.4347826086956521618, 0.4420289855072463969, 0.4492753623188405765, 0.4565217391304347561, 0.4637681159420289911, 0.4710144927536231707, 0.4782608695652174058, 0.4855072463768115854, 0.4927536231884058204, 0.5000000000000000000, 0.5072463768115942351, 0.5144927536231883591, 0.5217391304347825942, 0.5289855072463768293, 0.5362318840579710644, 0.5434782608695651884, 0.5507246376811594235, 0.5579710144927536586, 0.5652173913043477826, 0.5724637681159420177, 0.5797101449275362528, 0.5869565217391304879, 0.5942028985507246119, 0.6014492753623188470, 0.6086956521739130821, 0.6159420289855072062, 0.6231884057971014412, 0.6304347826086956763, 0.6376811594202898004, 0.6449275362318840354, 0.6521739130434782705, 0.6594202898550725056, 0.6666666666666666297, 0.6739130434782608647, 0.6811594202898550998, 0.6884057971014492239, 0.6956521739130434590, 0.7028985507246376940, 0.7101449275362319291, 0.7173913043478260532, 0.7246376811594202882, 0.7318840579710145233, 0.7391304347826086474, 0.7463768115942028825, 0.7536231884057971175, 0.7608695652173913526, 0.7681159420289854767, 0.7753623188405797118, 0.7826086956521739468, 0.7898550724637680709, 0.7971014492753623060, 0.8043478260869565410, 0.8115942028985507761, 0.8188405797101449002, 0.8260869565217391353, 0.8333333333333333703, 0.8405797101449274944, 0.8478260869565217295, 0.8550724637681159646, 0.8623188405797101996, 0.8695652173913043237, 0.8768115942028985588, 0.8840579710144927938, 0.8913043478260869179, 0.8985507246376811530, 0.9057971014492753881, 0.9130434782608695121, 0.9202898550724637472, 0.9275362318840579823, 0.9347826086956522174, 0.9420289855072463414, 0.9492753623188405765, 0.9565217391304348116, 0.9637681159420289356, 0.9662082893573751274, 0.9758703722509488587 ),
 .UNSPECIFIED. ) 
 GEOMETRIC_REPRESENTATION_ITEM ( )  RATIONAL_B_SPLINE_SURFACE ( (
 ( 1.000000000000000000, 0.8660254037844387076, 1.000000000000000000, 0.8660254037844387076, 1.000000000000000000, 0.8660254037844387076, 1.000000000000000000, 0.8660254037844387076, 1.000000000000000000, 0.8660254037844387076, 1.000000000000000000, 0.8660254037844387076, 1.000000000000000000, 0.8660254037844387076, 1.000000000000000000, 0.8660254037844387076, 1.000000000000000000, 0.8660254037844387076, 1.000000000000000000, 0.8660254037844387076, 1.000000000000000000, 0.8660254037844387076, 1.000000000000000000, 0.8660254037844387076, 1.000000000000000000, 0.8660254037844387076, 1.000000000000000000, 0.8660254037844387076, 1.000000000000000000, 0.8660254037844387076, 1.000000000000000000, 0.8660254037844387076, 1.000000000000000000, 0.8660254037844387076, 1.000000000000000000, 0.8660254037844387076, 1.000000000000000000, 0.8660254037844387076, 1.000000000000000000, 0.8660254037844387076, 1.000000000000000000, 0.8660254037844387076, 1.000000000000000000, 0.8660254037844387076, 1.000000000000000000, 0.8660254037844387076, 1.000000000000000000, 0.8660254037844387076, 1.000000000000000000, 0.8660254037844387076, 1.000000000000000000, 0.8660254037844387076, 1.000000000000000000, 0.8660254037844387076, 1.000000000000000000, 0.8660254037844387076, 1.000000000000000000, 0.8660254037844387076, 1.000000000000000000, 0.8660254037844387076, 1.000000000000000000, 0.8660254037844387076, 1.000000000000000000, 0.8660254037844387076, 1.000000000000000000, 0.8660254037844387076, 1.000000000000000000, 0.8660254037844387076, 1.000000000000000000, 0.8660254037844387076, 1.000000000000000000, 0.8660254037844387076, 1.000000000000000000, 0.8660254037844387076, 1.000000000000000000, 0.8660254037844387076, 1.000000000000000000, 0.8660254037844387076, 1.000000000000000000, 0.8660254037844387076, 1.000000000000000000, 0.8660254037844387076, 1.000000000000000000, 0.8660254037844387076, 1.000000000000000000, 0.8660254037844387076, 1.000000000000000000, 0.8660254037844387076, 1.000000000000000000, 0.8660254037844387076, 1.000000000000000000, 0.8660254037844387076, 1.000000000000000000, 0.8660254037844387076, 1.000000000000000000, 0.8660254037844387076, 1.000000000000000000, 0.8660254037844387076, 1.000000000000000000, 0.8660254037844387076, 1.000000000000000000, 0.8660254037844387076, 1.000000000000000000, 0.8660254037844387076, 1.000000000000000000, 0.8660254037844387076, 1.000000000000000000, 0.8660254037844387076, 1.000000000000000000, 0.8660254037844387076, 1.000000000000000000, 0.8660254037844387076, 1.000000000000000000, 0.8660254037844387076, 1.000000000000000000, 0.8660254037844387076, 1.000000000000000000, 0.8660254037844387076, 1.000000000000000000, 0.8660254037844387076, 1.000000000000000000, 0.8660254037844387076, 1.000000000000000000, 0.8660254037844387076, 1.000000000000000000, 0.8660254037844387076, 1.000000000000000000, 0.8660254037844387076, 1.000000000000000000, 0.8660254037844387076, 1.000000000000000000, 0.8660254037844387076, 1.000000000000000000, 0.8660254037844387076, 1.000000000000000000, 0.8660254037844387076, 1.000000000000000000, 0.8660254037844387076, 1.000000000000000000, 0.8660254037844387076, 1.000000000000000000, 0.8660254037844387076, 1.000000000000000000, 0.8660254037844387076, 1.000000000000000000, 0.8660254037844387076, 1.000000000000000000, 0.8660254037844387076, 1.000000000000000000, 0.8660254037844387076, 1.000000000000000000, 0.8660254037844387076, 1.000000000000000000, 0.8660254037844387076, 1.000000000000000000, 0.8660254037844387076, 1.000000000000000000, 0.8660254037844387076, 1.000000000000000000, 0.8660254037844387076, 1.000000000000000000, 0.8660254037844387076, 1.000000000000000000, 0.8660254037844387076, 1.000000000000000000, 0.8660254037844387076, 1.000000000000000000, 0.8660254037844387076, 1.000000000000000000, 0.8660254037844387076, 1.000000000000000000, 0.8660254037844387076, 1.000000000000000000, 0.8660254037844387076, 1.000000000000000000, 0.8660254037844387076, 1.000000000000000000, 0.8660254037844387076, 1.000000000000000000, 0.8660254037844387076, 1.000000000000000000, 0.8660254037844387076, 1.000000000000000000, 0.8660254037844387076, 1.000000000000000000, 0.8660254037844387076, 1.000000000000000000, 0.8660254037844387076, 1.000000000000000000, 0.8660254037844387076, 1.000000000000000000, 0.8660254037844387076, 1.000000000000000000, 0.8660254037844387076, 1.000000000000000000, 0.8660254037844387076, 1.000000000000000000, 0.8660254037844387076, 1.000000000000000000, 0.8660254037844387076, 1.000000000000000000, 0.8660254037844387076, 1.000000000000000000, 0.8660254037844387076, 1.000000000000000000, 0.8660254037844387076, 1.000000000000000000, 0.8660254037844387076, 1.000000000000000000, 0.8660254037844387076, 1.000000000000000000, 0.8660254037844387076, 1.000000000000000000, 0.8660254037844387076, 1.000000000000000000, 0.8660254037844387076, 1.000000000000000000, 0.8660254037844387076, 1.000000000000000000, 0.8660254037844387076, 1.000000000000000000, 0.8660254037844387076, 1.000000000000000000, 0.8660254037844387076, 1.000000000000000000, 0.8660254037844387076, 1.000000000000000000, 0.8660254037844387076, 1.000000000000000000, 0.8660254037844387076, 1.000000000000000000, 0.8660254037844387076, 1.000000000000000000, 0.8660254037844387076, 1.000000000000000000, 0.8660254037844387076, 1.000000000000000000, 0.8660254037844387076, 1.000000000000000000, 0.8660254037844387076, 1.000000000000000000, 0.8660254037844387076, 1.000000000000000000, 0.8660254037844387076, 1.000000000000000000, 0.8660254037844387076, 1.000000000000000000, 0.8660254037844387076, 1.000000000000000000, 0.8660254037844387076, 1.000000000000000000, 0.8660254037844387076, 1.000000000000000000, 0.8660254037844387076, 1.000000000000000000, 0.8660254037844387076, 1.000000000000000000, 0.8660254037844387076, 1.000000000000000000, 0.8660254037844387076, 1.000000000000000000, 0.8660254037844387076, 1.000000000000000000, 0.8660254037844387076, 1.000000000000000000, 0.8660254037844387076, 1.000000000000000000, 0.9548848677736607726, 0.9401542295229587953, 0.9401542295229587953, 0.9401542295229587953),
 ( 1.000000000000000000, 0.8660254037844387076, 1.000000000000000000, 0.8660254037844387076, 1.000000000000000000, 0.8660254037844387076, 1.000000000000000000, 0.8660254037844387076, 1.000000000000000000, 0.8660254037844387076, 1.000000000000000000, 0.8660254037844387076, 1.000000000000000000, 0.8660254037844387076, 1.000000000000000000, 0.8660254037844387076, 1.000000000000000000, 0.8660254037844387076, 1.000000000000000000, 0.8660254037844387076, 1.000000000000000000, 0.8660254037844387076, 1.000000000000000000, 0.8660254037844387076, 1.000000000000000000, 0.8660254037844387076, 1.000000000000000000, 0.8660254037844387076, 1.000000000000000000, 0.8660254037844387076, 1.000000000000000000, 0.8660254037844387076, 1.000000000000000000, 0.8660254037844387076, 1.000000000000000000, 0.8660254037844387076, 1.000000000000000000, 0.8660254037844387076, 1.000000000000000000, 0.8660254037844387076, 1.000000000000000000, 0.8660254037844387076, 1.000000000000000000, 0.8660254037844387076, 1.000000000000000000, 0.8660254037844387076, 1.000000000000000000, 0.8660254037844387076, 1.000000000000000000, 0.8660254037844387076, 1.000000000000000000, 0.8660254037844387076, 1.000000000000000000, 0.8660254037844387076, 1.000000000000000000, 0.8660254037844387076, 1.000000000000000000, 0.8660254037844387076, 1.000000000000000000, 0.8660254037844387076, 1.000000000000000000, 0.8660254037844387076, 1.000000000000000000, 0.8660254037844387076, 1.000000000000000000, 0.8660254037844387076, 1.000000000000000000, 0.8660254037844387076, 1.000000000000000000, 0.8660254037844387076, 1.000000000000000000, 0.8660254037844387076, 1.000000000000000000, 0.8660254037844387076, 1.000000000000000000, 0.8660254037844387076, 1.000000000000000000, 0.8660254037844387076, 1.000000000000000000, 0.8660254037844387076, 1.000000000000000000, 0.8660254037844387076, 1.000000000000000000, 0.8660254037844387076, 1.000000000000000000, 0.8660254037844387076, 1.000000000000000000, 0.8660254037844387076, 1.000000000000000000, 0.8660254037844387076, 1.000000000000000000, 0.8660254037844387076, 1.000000000000000000, 0.8660254037844387076, 1.000000000000000000, 0.8660254037844387076, 1.000000000000000000, 0.8660254037844387076, 1.000000000000000000, 0.8660254037844387076, 1.000000000000000000, 0.8660254037844387076, 1.000000000000000000, 0.8660254037844387076, 1.000000000000000000, 0.8660254037844387076, 1.000000000000000000, 0.8660254037844387076, 1.000000000000000000, 0.8660254037844387076, 1.000000000000000000, 0.8660254037844387076, 1.000000000000000000, 0.8660254037844387076, 1.000000000000000000, 0.8660254037844387076, 1.000000000000000000, 0.8660254037844387076, 1.000000000000000000, 0.8660254037844387076, 1.000000000000000000, 0.8660254037844387076, 1.000000000000000000, 0.8660254037844387076, 1.000000000000000000, 0.8660254037844387076, 1.000000000000000000, 0.8660254037844387076, 1.000000000000000000, 0.8660254037844387076, 1.000000000000000000, 0.8660254037844387076, 1.000000000000000000, 0.8660254037844387076, 1.000000000000000000, 0.8660254037844387076, 1.000000000000000000, 0.8660254037844387076, 1.000000000000000000, 0.8660254037844387076, 1.000000000000000000, 0.8660254037844387076, 1.000000000000000000, 0.8660254037844387076, 1.000000000000000000, 0.8660254037844387076, 1.000000000000000000, 0.8660254037844387076, 1.000000000000000000, 0.8660254037844387076, 1.000000000000000000, 0.8660254037844387076, 1.000000000000000000, 0.8660254037844387076, 1.000000000000000000, 0.8660254037844387076, 1.000000000000000000, 0.8660254037844387076, 1.000000000000000000, 0.8660254037844387076, 1.000000000000000000, 0.8660254037844387076, 1.000000000000000000, 0.8660254037844387076, 1.000000000000000000, 0.8660254037844387076, 1.000000000000000000, 0.8660254037844387076, 1.000000000000000000, 0.8660254037844387076, 1.000000000000000000, 0.8660254037844387076, 1.000000000000000000, 0.8660254037844387076, 1.000000000000000000, 0.8660254037844387076, 1.000000000000000000, 0.8660254037844387076, 1.000000000000000000, 0.8660254037844387076, 1.000000000000000000, 0.8660254037844387076, 1.000000000000000000, 0.8660254037844387076, 1.000000000000000000, 0.8660254037844387076, 1.000000000000000000, 0.8660254037844387076, 1.000000000000000000, 0.8660254037844387076, 1.000000000000000000, 0.8660254037844387076, 1.000000000000000000, 0.8660254037844387076, 1.000000000000000000, 0.8660254037844387076, 1.000000000000000000, 0.8660254037844387076, 1.000000000000000000, 0.8660254037844387076, 1.000000000000000000, 0.8660254037844387076, 1.000000000000000000, 0.8660254037844387076, 1.000000000000000000, 0.8660254037844387076, 1.000000000000000000, 0.8660254037844387076, 1.000000000000000000, 0.8660254037844387076, 1.000000000000000000, 0.8660254037844387076, 1.000000000000000000, 0.8660254037844387076, 1.000000000000000000, 0.8660254037844387076, 1.000000000000000000, 0.8660254037844387076, 1.000000000000000000, 0.8660254037844387076, 1.000000000000000000, 0.8660254037844387076, 1.000000000000000000, 0.8660254037844387076, 1.000000000000000000, 0.8660254037844387076, 1.000000000000000000, 0.8660254037844387076, 1.000000000000000000, 0.8660254037844387076, 1.000000000000000000, 0.8660254037844387076, 1.000000000000000000, 0.8660254037844387076, 1.000000000000000000, 0.8660254037844387076, 1.000000000000000000, 0.8660254037844387076, 1.000000000000000000, 0.8660254037844387076, 1.000000000000000000, 0.8660254037844387076, 1.000000000000000000, 0.8660254037844387076, 1.000000000000000000, 0.8660254037844387076, 1.000000000000000000, 0.8660254037844387076, 1.000000000000000000, 0.8660254037844387076, 1.000000000000000000, 0.8660254037844387076, 1.000000000000000000, 0.8660254037844387076, 1.000000000000000000, 0.8660254037844387076, 1.000000000000000000, 0.8660254037844387076, 1.000000000000000000, 0.8660254037844387076, 1.000000000000000000, 0.8660254037844387076, 1.000000000000000000, 0.8660254037844387076, 1.000000000000000000, 0.8660254037844387076, 1.000000000000000000, 0.9548848677736607726, 0.9401542295229587953, 0.9401542295229587953, 0.9401542295229587953) ) ) 
 REPRESENTATION_ITEM ( '' )  SURFACE ( )  );
#18461 = CARTESIAN_POINT ( 'NONE',  ( 22.97812500061451857, 4.541064518000418104, 2.621784821874999949 ) ) ;
#18462 = FACE_OUTER_BOUND ( 'NONE', #5811, .T. ) ;
#18463 = VERTEX_POINT ( 'NONE', #40528 ) ;
#18464 = CARTESIAN_POINT ( 'NONE',  ( 26.28749999999999432, 5.773502691896255534, 3.535250795749688894E-16 ) ) ;
#18465 = CARTESIAN_POINT ( 'NONE',  ( 1.999999999999998668, 12.65000000000000213, -33.46410161513775705 ) ) ;
#18466 = CARTESIAN_POINT ( 'NONE',  ( -1.878215178124999163, 18.75312499938548427, 26.74683588394047007 ) ) ;
#18467 = CARTESIAN_POINT ( 'NONE',  ( 3.159375000614518036, 4.541064518000418104, -2.621784821874998173 ) ) ;
#18468 = CARTESIAN_POINT ( 'NONE',  ( 9.403125000614517504, 4.541064518000418104, -2.621784821874998173 ) ) ;
#18469 = CARTESIAN_POINT ( 'NONE',  ( 21.60000000122903430, -2.886751345948129988, 4.999999999999997335 ) ) ;
#18470 = CARTESIAN_POINT ( 'NONE',  ( 26.42812500061451431, 6.421520780324663323E-16, -5.243569643749999010 ) ) ;
#18471 = CARTESIAN_POINT ( 'NONE',  ( 25.46249999999999858, 2.886751345948126879, 4.999999999999999112 ) ) ;
#18472 = CARTESIAN_POINT ( 'NONE',  ( 1.999999999999998668, 15.46250000122903501, -33.46410161513775705 ) ) ;
#18473 = CARTESIAN_POINT ( 'NONE',  ( 29.20312500061451644, 4.541064518000418104, -2.621784821874998173 ) ) ;
#18474 = CARTESIAN_POINT ( 'NONE',  ( 11.09062500061451573, -3.027376345333610441, -5.243569643749999898 ) ) ;
#18475 = ORIENTED_EDGE ( 'NONE', *, *, #14379, .F. ) ;
#18476 = CARTESIAN_POINT ( 'NONE',  ( 25.19062500061451715, 6.054752690667223547, 3.707466751127219781E-16 ) ) ;
#18477 = CARTESIAN_POINT ( 'NONE',  ( 7.078125000614516438, 6.421520780324663323E-16, -5.243569643749999010 ) ) ;
#18478 = CARTESIAN_POINT ( 'NONE',  ( 3.365625000614516082, -6.054752690667223547, -1.112240025338166033E-15 ) ) ;
#18479 = CARTESIAN_POINT ( 'NONE',  ( 17.25937500061451502, 0.000000000000000000, 4.756430356249998326 ) ) ;
#18480 = FACE_OUTER_BOUND ( 'NONE', #52325, .T. ) ;
#18481 = CARTESIAN_POINT ( 'NONE',  ( 14.06250000000000000, 2.886751345948129099, -4.999999999999998224 ) ) ;
#18482 = CARTESIAN_POINT ( 'NONE',  ( 13.39687500061451608, -3.027376345333610441, -5.243569643749999898 ) ) ;
#18483 = CARTESIAN_POINT ( 'NONE',  ( 11.10000000122903252, 5.773502691896255534, 3.535250795749688894E-16 ) ) ;
#18484 = CARTESIAN_POINT ( 'NONE',  ( 16.39687500061451786, -3.027376345333614438, 5.243569643749998122 ) ) ;
#18485 = CARTESIAN_POINT ( 'NONE',  ( 16.94999999999999929, 0.000000000000000000, 4.999999999999998224 ) ) ;
#18486 = CARTESIAN_POINT ( 'NONE',  ( 7.546875000614517326, -3.027376345333610441, -5.243569643749999898 ) ) ;
#18487 = CARTESIAN_POINT ( 'NONE',  ( 4.243569643749999898, 11.89062500061451644, -27.54997392385601529 ) ) ;
#18488 = DIRECTION ( 'NONE',  ( -1.000000000000000000, -0.000000000000000000, -0.000000000000000000 ) ) ;
#18489 = CARTESIAN_POINT ( 'NONE',  ( 22.77187500061451431, 5.824947211148865298E-16, -4.756430356249998326 ) ) ;
#18490 = ORIENTED_EDGE ( 'NONE', *, *, #62721, .F. ) ;
#18491 = EDGE_CURVE ( 'NONE', #10316, #70443, #62689, .T. ) ;
#18492 = CARTESIAN_POINT ( 'NONE',  ( 24.25312500061451715, 4.541064518000418104, -2.621784821874998173 ) ) ;
#18493 = CARTESIAN_POINT ( 'NONE',  ( -2.498395430326213790E-14, 20.65624999877097068, 26.00000000000000000 ) ) ;
#18494 = CARTESIAN_POINT ( 'NONE',  ( 28.02187500061451431, 3.027376345333611329, 5.243569643749999010 ) ) ;
#18495 = CARTESIAN_POINT ( 'NONE',  ( 23.58749999999999858, 5.773502691896255534, 3.535250795749688894E-16 ) ) ;
#18496 = CARTESIAN_POINT ( 'NONE',  ( 7.415625000614516793, -6.054752690667223547, -1.112240025338166033E-15 ) ) ;
#18497 = CARTESIAN_POINT ( 'NONE',  ( 24.83437500061451075, -2.746126346562646425, 4.756430356249996549 ) ) ;
#18498 = CARTESIAN_POINT ( 'NONE',  ( 20.25937500061451857, 4.541064518000418104, -2.621784821874998173 ) ) ;
#18499 = CARTESIAN_POINT ( 'NONE',  ( 10.13437500061451679, -2.746126346562641984, -4.756430356249999214 ) ) ;
#18500 = CARTESIAN_POINT ( 'NONE',  ( 29.36250000122903003, -4.330127018922190985, -2.500000000000001332 ) ) ;
#18501 = CARTESIAN_POINT ( 'NONE',  ( 8.634375000614518569, 4.541064518000418104, 2.621784821874999949 ) ) ;
#18502 = ORIENTED_EDGE ( 'NONE', *, *, #54530, .T. ) ;
#18503 = CARTESIAN_POINT ( 'NONE',  ( 20.07187500061451857, -6.054752690667223547, -1.112240025338166033E-15 ) ) ;
#18504 = CARTESIAN_POINT ( 'NONE',  ( -3.999999999999999112, 15.78124999877096535, 27.69059892324149530 ) ) ;
#18505 = CARTESIAN_POINT ( 'NONE',  ( 26.36249999999999716, 2.886751345948126879, 4.999999999999999112 ) ) ;
#18506 = CARTESIAN_POINT ( 'NONE',  ( 28.54687500061451644, -3.027376345333614438, 5.243569643749998122 ) ) ;
#18507 = CARTESIAN_POINT ( 'NONE',  ( 26.34375000122902577, 5.773502691896255534, 3.535250795749688401E-16 ) ) ;
#18508 = CARTESIAN_POINT ( 'NONE',  ( 10.65000000000000036, 0.000000000000000000, 4.999999999999998224 ) ) ;
#18509 = VERTEX_POINT ( 'NONE', #34241 ) ;
#18510 = CARTESIAN_POINT ( 'NONE',  ( 9.750000000000001776, 0.000000000000000000, 4.999999999999998224 ) ) ;
#18511 = CARTESIAN_POINT ( 'NONE',  ( 12.72187500061451537, -4.119189519843968306, 2.378215178124996054 ) ) ;
#18512 = CARTESIAN_POINT ( 'NONE',  ( 23.84062500061451928, 6.054752690667223547, 3.707466751127219781E-16 ) ) ;
#18513 = CARTESIAN_POINT ( 'NONE',  ( 13.01249999999999929, -5.773502691896255534, -1.060575238724906372E-15 ) ) ;
#18514 = CARTESIAN_POINT ( 'NONE',  ( 8.100000001229034297, -2.886751345948129988, 4.999999999999997335 ) ) ;
#18515 = CARTESIAN_POINT ( 'NONE',  ( 5.878125000614517148, 4.541064518000418104, 2.621784821874999949 ) ) ;
#18516 = CARTESIAN_POINT ( 'NONE',  ( 20.96250000000000213, 2.886751345948126879, 4.999999999999999112 ) ) ;
#18517 = B_SPLINE_CURVE_WITH_KNOTS ( 'NONE', 3,
 ( #21885, #50346, #27080, #10085, #4909, #49611, #72870, #32615, #55516, #4187, #16339, #19776, #49249, #71784, #9714, #26715, #32248, #55879, #43342, #25326, #33698, #10806, #65864, #32976, #55153, #44807, #21152, #27445, #47872, #15246, #37783, #72138, #2799, #4551, #21518, #43706, #44072, #66227 ),
 .UNSPECIFIED., .F., .F.,
 ( 4, 2, 2, 2, 2, 2, 2, 2, 2, 2, 2, 2, 2, 2, 2, 2, 2, 2, 4 ),
 ( 0.01305910913008847749, 0.01347211191627390239, 0.01388511470245932730, 0.01471112027483017712, 0.01553712584720102867, 0.01636313141957188022, 0.01801514256431357638, 0.01884114813668442273, 0.01925415092286984764, 0.01966715370905527255, 0.02008015649524069746, 0.02049315928142611890, 0.02131916485379695830, 0.02214517042616779424, 0.02297117599853863018, 0.02379718157090946959, 0.02462318714328030553, 0.02544919271565114494, 0.02627519828802198087 ),
 .UNSPECIFIED. ) ;
#18518 = CARTESIAN_POINT ( 'NONE',  ( 22.07812500061451644, 4.541064518000418104, 2.621784821874999949 ) ) ;
#18519 = CARTESIAN_POINT ( 'NONE',  ( 23.47499999999999787, 6.123233995736764310E-16, -4.999999999999998224 ) ) ;
#18520 = CARTESIAN_POINT ( 'NONE',  ( 24.90000000122903145, -2.886751345948125991, -5.000000000000000000 ) ) ;
#18521 = CARTESIAN_POINT ( 'NONE',  ( 3.756430356249998770, 16.65312499938548285, 32.16877607737301759 ) ) ;
#18522 = CARTESIAN_POINT ( 'NONE',  ( 4.537500000000000533, -2.886751345948125991, -5.000000000000000000 ) ) ;
#18523 = VERTEX_POINT ( 'NONE', #7267 ) ;
#18524 = CARTESIAN_POINT ( 'NONE',  ( 22.00312500061451360, 4.541064518000418104, -2.621784821874998173 ) ) ;
#18525 = CARTESIAN_POINT ( 'NONE',  ( 27.81562500061452070, 3.027376345333613106, -5.243569643749998122 ) ) ;
#18526 = CARTESIAN_POINT ( 'NONE',  ( 27.83437500061451786, 6.421520780324663323E-16, -5.243569643749999010 ) ) ;
#18527 = CARTESIAN_POINT ( 'NONE',  ( 13.64062500061451644, -3.027376345333614438, 5.243569643749998122 ) ) ;
#18528 = CARTESIAN_POINT ( 'NONE',  ( 29.96249999999999858, 2.886751345948126879, 4.999999999999998224 ) ) ;
#18529 = VECTOR ( 'NONE', #49464, 1000.000000000000000 ) ;
#18530 = CARTESIAN_POINT ( 'NONE',  ( 25.57500000122903216, 2.886751345948126879, 4.999999999999999112 ) ) ;
#18531 = CARTESIAN_POINT ( 'NONE',  ( 21.19687500061451502, 5.492252693125287522, 3.363034840372157021E-16 ) ) ;
#18532 = CARTESIAN_POINT ( 'NONE',  ( 16.49062500061451786, -3.027376345333610441, -5.243569643749999898 ) ) ;
#18533 = CARTESIAN_POINT ( 'NONE',  ( -1.071796769724483234, 16.75759618943233420, -34.00000000000000711 ) ) ;
#18534 = ADVANCED_FACE ( 'NONE', ( #18691 ), #71542, .T. ) ;
#18535 = CARTESIAN_POINT ( 'NONE',  ( 5.887500001229034829, -4.330127018922194537, 2.499999999999995559 ) ) ;
#18536 = CARTESIAN_POINT ( 'NONE',  ( 11.18437500061451928, 6.421520780324663323E-16, -5.243569643749999010 ) ) ;
#18537 = CARTESIAN_POINT ( 'NONE',  ( 12.23437500061451821, 4.541064518000418104, 2.621784821874999949 ) ) ;
#18538 = CARTESIAN_POINT ( 'NONE',  ( 20.44687500061451857, -3.027376345333614438, 5.243569643749998122 ) ) ;
#18539 = ORIENTED_EDGE ( 'NONE', *, *, #31941, .F. ) ;
#18540 = CARTESIAN_POINT ( 'NONE',  ( 24.07500000122903572, 2.886751345948162850, -4.999999999999940492 ) ) ;
#18541 = CARTESIAN_POINT ( 'NONE',  ( 23.16562500061451502, -6.054752690667223547, -1.112240025338166033E-15 ) ) ;
#18542 = CARTESIAN_POINT ( 'NONE',  ( 18.15937500061451715, 0.000000000000000000, 5.243569643749999010 ) ) ;
#18543 = CARTESIAN_POINT ( 'NONE',  ( 24.51562500061451289, -6.054752690667223547, -1.112240025338166033E-15 ) ) ;
#18544 = CARTESIAN_POINT ( 'NONE',  ( -3.999999999999997335, 15.08750000000000036, 32.30940107675850470 ) ) ;
#18545 = CARTESIAN_POINT ( 'NONE',  ( 29.72812500061451502, 4.541064518000418104, 2.621784821874999949 ) ) ;
#18546 = CARTESIAN_POINT ( 'NONE',  ( 8.475000001229034297, 2.886751345948126879, 4.999999999999999112 ) ) ;
#18547 = CARTESIAN_POINT ( 'NONE',  ( 5.737500001229033586, 4.330127018922191873, 2.499999999999999556 ) ) ;
#18548 = CARTESIAN_POINT ( 'NONE',  ( 28.42499999999999716, 6.123233995736764310E-16, -4.999999999999998224 ) ) ;
#18549 = CARTESIAN_POINT ( 'NONE',  ( 28.08750000122903145, 6.123233995736764310E-16, -4.999999999999998224 ) ) ;
#18550 = CARTESIAN_POINT ( 'NONE',  ( -3.999999999999999556, 20.73124999877096641, 27.69059892324149175 ) ) ;
#18551 = CARTESIAN_POINT ( 'NONE',  ( 10.39687500061451786, 6.054752690667223547, 3.707466751127219781E-16 ) ) ;
#18552 = CARTESIAN_POINT ( 'NONE',  ( 9.487499999999997158, -2.886751345948126435, -5.000000000000000000 ) ) ;
#18553 = CARTESIAN_POINT ( 'NONE',  ( 17.61562500061451786, 3.027376345333611329, 5.243569643749999010 ) ) ;
#18554 = CARTESIAN_POINT ( 'NONE',  ( 12.00937500061451857, -4.541064518000417216, -2.621784821875001281 ) ) ;
#18555 = CARTESIAN_POINT ( 'NONE',  ( 3.103125000614517237, 4.541064518000418104, -2.621784821874998173 ) ) ;
#18556 = CARTESIAN_POINT ( 'NONE',  ( 18.57187500061451857, 3.027376345333611329, 5.243569643749999010 ) ) ;
#18557 = CARTESIAN_POINT ( 'NONE',  ( 8.371875000614515727, -6.054752690667223547, -1.112240025338166033E-15 ) ) ;
#18558 = CARTESIAN_POINT ( 'NONE',  ( 3.703125000614516882, 0.000000000000000000, 5.243569643749999010 ) ) ;
#18559 = DIRECTION ( 'NONE',  ( -1.000000000000000000, -0.000000000000000000, -0.000000000000000000 ) ) ;
#18560 = CARTESIAN_POINT ( 'NONE',  ( 7.303125000614516082, 0.000000000000000000, 5.243569643749999010 ) ) ;
#18561 = CARTESIAN_POINT ( 'NONE',  ( 17.05312500061451786, 4.541064518000418104, -2.621784821874998173 ) ) ;
#18562 = VERTEX_POINT ( 'NONE', #40233 ) ;
#18563 = CARTESIAN_POINT ( 'NONE',  ( 6.300000001229033586, -2.886751345948129988, 4.999999999999997335 ) ) ;
#18564 = CARTESIAN_POINT ( 'NONE',  ( 14.31562500061451537, 3.027376345333613106, -5.243569643749998122 ) ) ;
#18565 = CARTESIAN_POINT ( 'NONE',  ( 13.56562500061451892, 3.027376345333611329, 5.243569643749999010 ) ) ;
#18566 = CARTESIAN_POINT ( 'NONE',  ( 24.45937500061451786, 0.000000000000000000, 4.756430356249998326 ) ) ;
#18567 = CARTESIAN_POINT ( 'NONE',  ( 14.28750000000000142, -2.886751345948129988, 4.999999999999997335 ) ) ;
#18568 = CARTESIAN_POINT ( 'NONE',  ( 7.087500001229034119, 4.330127018922191873, 2.499999999999999556 ) ) ;
#18569 = CARTESIAN_POINT ( 'NONE',  ( 29.13749999999999929, -2.886751345948095349, 5.000000000000058620 ) ) ;
#18570 = CARTESIAN_POINT ( 'NONE',  ( 15.64687500061451608, -3.027376345333610441, -5.243569643749999898 ) ) ;
#18571 = CARTESIAN_POINT ( 'NONE',  ( 17.85000000122903430, 5.773502691896255534, 3.535250795749688894E-16 ) ) ;
#18572 = CARTESIAN_POINT ( 'NONE',  ( 25.42500000000000071, 4.330127018922191873, 2.499999999999999556 ) ) ;
#18573 = CARTESIAN_POINT ( 'NONE',  ( -3.000416591977282496E-16, 18.34062500061451928, -34.90005215228797653 ) ) ;
#18574 = CARTESIAN_POINT ( 'NONE',  ( -3.999999999999999112, 13.13749999999999751, 27.69059892324149530 ) ) ;
#18575 = CARTESIAN_POINT ( 'NONE',  ( 6.825000000000001066, 6.123233995736764310E-16, -4.999999999999998224 ) ) ;
#18576 = VECTOR ( 'NONE', #68259, 1000.000000000000000 ) ;
#18577 = CARTESIAN_POINT ( 'NONE',  ( 9.637500001229033941, 6.123233995736764310E-16, -4.999999999999998224 ) ) ;
#18578 = CARTESIAN_POINT ( 'NONE',  ( 24.37500000000000000, 6.123233995736764310E-16, -4.999999999999998224 ) ) ;
#18579 = CARTESIAN_POINT ( 'NONE',  ( 17.48437500061451999, 6.421520780324663323E-16, -5.243569643749999010 ) ) ;
#18580 =( BOUNDED_CURVE ( )  B_SPLINE_CURVE ( 2, ( #11510, #45855, #51035, #44785, #5245, #27787, #432 ),
 .UNSPECIFIED., .F., .F. ) 
 B_SPLINE_CURVE_WITH_KNOTS ( ( 3, 2, 2, 3 ),
 ( 0.6600000000000000311, 0.6633333333333333304, 0.6666666666666666297, 0.6700000000000000400 ),
 .UNSPECIFIED. ) 
 CURVE ( )  GEOMETRIC_REPRESENTATION_ITEM ( )  RATIONAL_B_SPLINE_CURVE ( ( 1.000000000000000000, 0.8660254037844387076, 1.000000000000000000, 0.8660254037844387076, 1.000000000000000000, 0.8660254037844387076, 1.000000000000000000 ) ) 
 REPRESENTATION_ITEM ( '' )  );
#18581 = CARTESIAN_POINT ( 'NONE',  ( 15.22500000000000142, -4.330127018922194537, 2.499999999999995559 ) ) ;
#18582 = CARTESIAN_POINT ( 'NONE',  ( 14.39062500061451821, 6.054752690667223547, 3.707466751127219781E-16 ) ) ;
#18583 = CARTESIAN_POINT ( 'NONE',  ( 9.656250001229032875, 4.330127018922192761, -2.499999999999997780 ) ) ;
#18584 = CARTESIAN_POINT ( 'NONE',  ( 8.962500000000002132, -5.773502691896255534, -1.060575238724906372E-15 ) ) ;
#18585 = CARTESIAN_POINT ( 'NONE',  ( 26.14687500061451431, 6.054752690667223547, 3.707466751127219781E-16 ) ) ;
#18586 = CARTESIAN_POINT ( 'NONE',  ( 19.43437500061451573, -2.746126346562646425, 4.756430356249996549 ) ) ;
#18587 = CARTESIAN_POINT ( 'NONE',  ( 11.16562500061451679, 3.027376345333613106, -5.243569643749998122 ) ) ;
#18588 = CARTESIAN_POINT ( 'NONE',  ( 16.13437500061451502, 6.421520780324663323E-16, -5.243569643749999010 ) ) ;
#18589 = ORIENTED_EDGE ( 'NONE', *, *, #46820, .F. ) ;
#18590 = CARTESIAN_POINT ( 'NONE',  ( 26.65312500061451573, 0.000000000000000000, 5.243569643749999010 ) ) ;
#18591 = CARTESIAN_POINT ( 'NONE',  ( 21.14062500061451289, 6.054752690667223547, 3.707466751127219781E-16 ) ) ;
#18592 = CARTESIAN_POINT ( 'NONE',  ( 29.05312500061451431, -4.541064518000417216, -2.621784821875001281 ) ) ;
#18593 = AXIS2_PLACEMENT_3D ( 'NONE', #6340, #36955, #64296 ) ;
#18594 = CARTESIAN_POINT ( 'NONE',  ( -3.999999999999997335, 14.30000000122903359, -27.69059892324149530 ) ) ;
#18595 = CARTESIAN_POINT ( 'NONE',  ( 10.72500000000000142, -4.330127018922194537, 2.499999999999995559 ) ) ;
#18596 = CARTESIAN_POINT ( 'NONE',  ( 18.22500000122903430, 2.886751345948129099, -4.999999999999998224 ) ) ;
#18597 = CARTESIAN_POINT ( 'NONE',  ( 0.000000000000000000, 0.000000000000000000, 50.00000000000000000 ) ) ;
#18598 = CARTESIAN_POINT ( 'NONE',  ( 10.28437500061451892, 5.492252693125287522, 3.363034840372157021E-16 ) ) ;
#18599 = ORIENTED_EDGE ( 'NONE', *, *, #72525, .T. ) ;
#18600 = CARTESIAN_POINT ( 'NONE',  ( 16.57499999999999929, -4.330127018922194537, 2.499999999999995559 ) ) ;
#18601 = CARTESIAN_POINT ( 'NONE',  ( 22.34999999999999787, 0.000000000000000000, 4.999999999999998224 ) ) ;
#18602 = CARTESIAN_POINT ( 'NONE',  ( 18.04687500061451999, 6.054752690667223547, 3.707466751127219781E-16 ) ) ;
#18603 = CARTESIAN_POINT ( 'NONE',  ( 13.52812500061451750, 4.541064518000418104, 2.621784821874999949 ) ) ;
#18604 = ORIENTED_EDGE ( 'NONE', *, *, #53983, .F. ) ;
#18605 = CARTESIAN_POINT ( 'NONE',  ( 4.940625000614515372, 6.054752690667223547, 3.707466751127219781E-16 ) ) ;
#18606 = CARTESIAN_POINT ( 'NONE',  ( 2.417052323292336544E-14, 20.48749999999999716, 34.00000000000000000 ) ) ;
#18607 = CARTESIAN_POINT ( 'NONE',  ( 12.11250000000000249, -5.773502691896255534, -1.060575238724906372E-15 ) ) ;
#18608 = CARTESIAN_POINT ( 'NONE',  ( 28.20937500061451075, 2.746126346562645981, -4.756430356249997438 ) ) ;
#18609 = CARTESIAN_POINT ( 'NONE',  ( -4.243569643749999898, 17.96562500061451573, 27.54997392385601529 ) ) ;
#18610 = CARTESIAN_POINT ( 'NONE',  ( 29.27812500061451573, 4.541064518000418104, 2.621784821874999949 ) ) ;
#18611 = CARTESIAN_POINT ( 'NONE',  ( 9.825000000000001066, -4.330127018922194537, 2.499999999999995559 ) ) ;
#18612 = CARTESIAN_POINT ( 'NONE',  ( 1.878215178125000495, 16.31562499938548427, 26.74683588394047007 ) ) ;
#18613 = CARTESIAN_POINT ( 'NONE',  ( 26.59687500061451360, 6.054752690667223547, 3.707466751127219781E-16 ) ) ;
#18614 = ORIENTED_EDGE ( 'NONE', *, *, #53086, .T. ) ;
#18615 = CARTESIAN_POINT ( 'NONE',  ( 22.71562500061451573, -6.054752690667223547, -1.112240025338166033E-15 ) ) ;
#18616 = CARTESIAN_POINT ( 'NONE',  ( 23.44687500061451502, 6.054752690667223547, 3.707466751127219781E-16 ) ) ;
#18617 = CARTESIAN_POINT ( 'NONE',  ( 4.243569643749999010, 17.36562500061459602, -32.45002607614398471 ) ) ;
#18618 = CARTESIAN_POINT ( 'NONE',  ( 5.953125000614519102, 0.000000000000000000, 5.243569643749999010 ) ) ;
#18619 = CARTESIAN_POINT ( 'NONE',  ( 29.37187500061451928, 2.746126346562643317, 4.756430356249998326 ) ) ;
#18620 = CARTESIAN_POINT ( 'NONE',  ( 24.17812500061451786, 6.421520780324663323E-16, -5.243569643749999010 ) ) ;
#18621 = CARTESIAN_POINT ( 'NONE',  ( 28.77187500061451431, 4.119189519843966529, 2.378215178124999607 ) ) ;
#18622 = CARTESIAN_POINT ( 'NONE',  ( 10.47187500061451715, 2.746126346562643317, 4.756430356249998326 ) ) ;
#18623 = CARTESIAN_POINT ( 'NONE',  ( 16.17187500061451644, 3.027376345333613106, -5.243569643749998122 ) ) ;
#18624 = CARTESIAN_POINT ( 'NONE',  ( 18.64687500061451786, -3.027376345333614438, 5.243569643749998122 ) ) ;
#18625 = CARTESIAN_POINT ( 'NONE',  ( 26.22187500061451715, 3.027376345333611329, 5.243569643749999010 ) ) ;
#18626 = CARTESIAN_POINT ( 'NONE',  ( -2.121784821874999949, 17.53437500061451715, 26.32496088578401938 ) ) ;
#18627 = CARTESIAN_POINT ( 'NONE',  ( 7.003125000614518036, -4.541064518000417216, -2.621784821875001281 ) ) ;
#18628 = CARTESIAN_POINT ( 'NONE',  ( -3.999999999999997335, 19.13750000000000284, 32.30940107675850470 ) ) ;
#18629 = EDGE_CURVE ( 'NONE', #11388, #57032, #4002, .T. ) ;
#18630 = CARTESIAN_POINT ( 'NONE',  ( 4.996875000614516615, 6.054752690667223547, 3.707466751127219781E-16 ) ) ;
#18631 = CARTESIAN_POINT ( 'NONE',  ( 5.578125000614518214, -4.541064518000419881, 2.621784821874995952 ) ) ;
#18632 = CARTESIAN_POINT ( 'NONE',  ( 8.971875000614515372, 3.027376345333613106, -5.243569643749998122 ) ) ;
#18633 = SURFACE_STYLE_FILL_AREA ( #13450 ) ;
#18634 = CARTESIAN_POINT ( 'NONE',  ( 17.36250000122903359, 4.330127018922192761, -2.499999999999997780 ) ) ;
#18635 = CARTESIAN_POINT ( 'NONE',  ( 4.696875000614518569, -3.027376345333614438, 5.243569643749998122 ) ) ;
#18636 = CARTESIAN_POINT ( 'NONE',  ( 8.615625000614517859, 3.027376345333611329, 5.243569643749999010 ) ) ;
#18637 = CARTESIAN_POINT ( 'NONE',  ( 1.999999999999997335, 14.61874999877096570, 33.46410161513775705 ) ) ;
#18638 = CARTESIAN_POINT ( 'NONE',  ( 23.83125000122903359, -4.330127018922194537, 2.499999999999995559 ) ) ;
#18639 = CARTESIAN_POINT ( 'NONE',  ( 16.95937500061451786, -4.541064518000417216, -2.621784821875001281 ) ) ;
#18640 = CARTESIAN_POINT ( 'NONE',  ( 27.71250000000000568, 2.886751345948102454, 5.000000000000042633 ) ) ;
#18641 = VERTEX_POINT ( 'NONE', #29145 ) ;
#18642 = CARTESIAN_POINT ( 'NONE',  ( 24.92812500061451431, -4.541064518000419881, 2.621784821874995952 ) ) ;
#18643 = CARTESIAN_POINT ( 'NONE',  ( 8.578125000614518214, 4.541064518000418104, 2.621784821874999949 ) ) ;
#18644 = CARTESIAN_POINT ( 'NONE',  ( 26.14687500061451431, 6.054752690667223547, 3.707466751127219781E-16 ) ) ;
#18645 = CARTESIAN_POINT ( 'NONE',  ( 9.478125000614515017, 4.541064518000418104, 2.621784821874999949 ) ) ;
#18646 = CARTESIAN_POINT ( 'NONE',  ( -4.243569643749999898, 10.82187500061451857, -32.45002607614398471 ) ) ;
#18647 = EDGE_CURVE ( 'NONE', #61789, #8626, #44336, .T. ) ;
#18648 = CARTESIAN_POINT ( 'NONE',  ( 10.53750000122903252, 6.123233995736764310E-16, -4.999999999999998224 ) ) ;
#18649 =( BOUNDED_CURVE ( )  B_SPLINE_CURVE ( 3, ( #13042, #31508, #35580, #58462 ),
 .UNSPECIFIED., .F., .F. ) 
 B_SPLINE_CURVE_WITH_KNOTS ( ( 4, 4 ),
 ( 2.843340893843762540, 2.939989945538246996 ),
 .UNSPECIFIED. ) 
 CURVE ( )  GEOMETRIC_REPRESENTATION_ITEM ( )  RATIONAL_B_SPLINE_CURVE ( ( 1.000000000000000000, 0.9992217315398195243, 0.9992217315398195243, 1.000000000000000000 ) ) 
 REPRESENTATION_ITEM ( '' )  );
#18650 = CARTESIAN_POINT ( 'NONE',  ( 24.85312500061451502, 0.000000000000000000, 5.243569643749999010 ) ) ;
#18651 = CARTESIAN_POINT ( 'NONE',  ( -4.243569643749999898, 13.46562500061451928, -32.45002607614398471 ) ) ;
#18652 = CARTESIAN_POINT ( 'NONE',  ( 12.45000000122903394, 5.773502691896255534, 3.535250795749688894E-16 ) ) ;
#18653 = CARTESIAN_POINT ( 'NONE',  ( 21.66562500061451502, 3.027376345333611329, 5.243569643749999010 ) ) ;
#18654 = CARTESIAN_POINT ( 'NONE',  ( 10.20000000000000107, 0.000000000000000000, 4.999999999999998224 ) ) ;
#18655 = CARTESIAN_POINT ( 'NONE',  ( 20.24062500061451431, 6.054752690667223547, 3.707466751127219781E-16 ) ) ;
#18656 = CARTESIAN_POINT ( 'NONE',  ( 3.878215178125000051, 12.57031249969274178, 30.00000000000000000 ) ) ;
#18657 = CARTESIAN_POINT ( 'NONE',  ( 20.28750000000000142, -2.886751345948125991, -5.000000000000000000 ) ) ;
#18658 = CARTESIAN_POINT ( 'NONE',  ( 14.25000000122903465, 5.773502691896255534, 3.535250795749688894E-16 ) ) ;
#18659 = CARTESIAN_POINT ( 'NONE',  ( 10.19062500061451892, -3.027376345333610441, -5.243569643749999898 ) ) ;
#18660 = CARTESIAN_POINT ( 'NONE',  ( 15.02812500061451750, -4.541064518000419881, 2.621784821874995952 ) ) ;
#18661 = CARTESIAN_POINT ( 'NONE',  ( 25.87500000122903288, 2.886751345948129099, -4.999999999999998224 ) ) ;
#18662 = CARTESIAN_POINT ( 'NONE',  ( 22.32187500061451502, -6.054752690667223547, -1.112240025338166033E-15 ) ) ;
#18663 = LINE ( 'NONE', #57474, #12330 ) ;
#18664 = CARTESIAN_POINT ( 'NONE',  ( 8.100000001229034297, -2.886751345948129988, 4.999999999999997335 ) ) ;
#18665 = CARTESIAN_POINT ( 'NONE',  ( 9.421875000614519990, 3.027376345333613106, -5.243569643749998122 ) ) ;
#18666 = CARTESIAN_POINT ( 'NONE',  ( 25.58437500061451431, 6.421520780324663323E-16, -5.243569643749999010 ) ) ;
#18667 = CARTESIAN_POINT ( 'NONE',  ( 23.88749999999999929, -2.886751345948153968, -4.999999999999952038 ) ) ;
#18668 = CARTESIAN_POINT ( 'NONE',  ( 20.09062500061451573, -3.027376345333610441, -5.243569643749999898 ) ) ;
#18669 = CARTESIAN_POINT ( 'NONE',  ( 25.50937500061451502, -4.541064518000417216, -2.621784821875001281 ) ) ;
#18670 = CARTESIAN_POINT ( 'NONE',  ( -3.756430356250000102, 17.02812499938548285, 30.00000000000000000 ) ) ;
#18671 = CARTESIAN_POINT ( 'NONE',  ( 3.255427375287384351, -3.795065400537469102, 3.471954933061189852 ) ) ;
#18672 = CARTESIAN_POINT ( 'NONE',  ( 8.821875000614518569, -6.054752690667223547, -1.112240025338166033E-15 ) ) ;
#18673 = CARTESIAN_POINT ( 'NONE',  ( 16.19062500061451715, 6.054752690667223547, 3.707466751127219781E-16 ) ) ;
#18674 = ORIENTED_EDGE ( 'NONE', *, *, #48506, .F. ) ;
#18675 = CARTESIAN_POINT ( 'NONE',  ( -1.999999999999997113, 12.87500000000000178, -26.53589838486224295 ) ) ;
#18676 = CARTESIAN_POINT ( 'NONE',  ( 27.92812500061451431, 4.541064518000418104, 2.621784821874999949 ) ) ;
#18677 = CARTESIAN_POINT ( 'NONE',  ( 3.121875000614518836, 3.027376345333613106, -5.243569643749998122 ) ) ;
#18678 = CARTESIAN_POINT ( 'NONE',  ( 27.07499999999999929, 6.123233995736764310E-16, -4.999999999999998224 ) ) ;
#18679 = CARTESIAN_POINT ( 'NONE',  ( 16.76249999999999929, 2.886751345948129099, -4.999999999999998224 ) ) ;
#18680 = CARTESIAN_POINT ( 'NONE',  ( 20.99062500061451431, -3.027376345333610441, -5.243569643749999898 ) ) ;
#18681 = ORIENTED_EDGE ( 'NONE', *, *, #59515, .F. ) ;
#18682 = CARTESIAN_POINT ( 'NONE',  ( 25.19999999999999929, -4.330127018922190985, -2.500000000000001332 ) ) ;
#18683 = CARTESIAN_POINT ( 'NONE',  ( 26.29687500061451644, -3.027376345333614438, 5.243569643749998122 ) ) ;
#18684 = ORIENTED_EDGE ( 'NONE', *, *, #66354, .F. ) ;
#18685 = CARTESIAN_POINT ( 'NONE',  ( 11.91562500061451857, -6.054752690667223547, -1.112240025338166033E-15 ) ) ;
#18686 = CARTESIAN_POINT ( 'NONE',  ( 6.778125000614518392, 4.541064518000418104, 2.621784821874999949 ) ) ;
#18687 = CARTESIAN_POINT ( 'NONE',  ( 15.57187500061451679, 5.824947211148865298E-16, -4.756430356249998326 ) ) ;
#18688 = CARTESIAN_POINT ( 'NONE',  ( 3.309375000614518836, 0.000000000000000000, 5.243569643749999010 ) ) ;
#18689 = CARTESIAN_POINT ( 'NONE',  ( 15.52500000122903323, 2.886751345948129099, -4.999999999999998224 ) ) ;
#18690 = CARTESIAN_POINT ( 'NONE',  ( 22.72499999999999787, 4.330127018922191873, 2.499999999999999556 ) ) ;
#18691 = FACE_OUTER_BOUND ( 'NONE', #6185, .T. ) ;
#18692 = CARTESIAN_POINT ( 'NONE',  ( 4.359375000614517326, -4.541064518000417216, -2.621784821875001281 ) ) ;
#18693 = CARTESIAN_POINT ( 'NONE',  ( 9.234375000614518214, -4.541064518000419881, 2.621784821874995952 ) ) ;
#18694 = CARTESIAN_POINT ( 'NONE',  ( 19.92187500061451644, 3.027376345333611329, 5.243569643749999010 ) ) ;
#18695 = CARTESIAN_POINT ( 'NONE',  ( -1.999999999999997113, 15.23750000122903536, -26.53589838486224295 ) ) ;
#18696 = ORIENTED_EDGE ( 'NONE', *, *, #64237, .T. ) ;
#18697 = CARTESIAN_POINT ( 'NONE',  ( 29.12812500061451715, 6.421520780324663323E-16, -5.243569643749999010 ) ) ;
#18698 = CARTESIAN_POINT ( 'NONE',  ( 29.63437500061451502, 6.421520780324663323E-16, -5.243569643749999010 ) ) ;
#18699 = CARTESIAN_POINT ( 'NONE',  ( 3.871875000614519280, -6.054752690667223547, -1.112240025338166033E-15 ) ) ;
#18700 = CARTESIAN_POINT ( 'NONE',  ( 15.59999999999999964, 0.000000000000000000, 4.999999999999998224 ) ) ;
#18701 = CARTESIAN_POINT ( 'NONE',  ( 13.64062500061451644, -3.027376345333614438, 5.243569643749998122 ) ) ;
#18702 = CARTESIAN_POINT ( 'NONE',  ( 4.000000000000000000, 14.00000000122903465, 32.30940107675849760 ) ) ;
#18703 = CARTESIAN_POINT ( 'NONE',  ( 27.13125000122903430, 6.123233995736764310E-16, -4.999999999999998224 ) ) ;
#18704 = CARTESIAN_POINT ( 'NONE',  ( 20.70000000122903216, -2.886751345948129988, 4.999999999999997335 ) ) ;
#18705 = CARTESIAN_POINT ( 'NONE',  ( 16.72500000000000142, 6.123233995736764310E-16, -4.999999999999998224 ) ) ;
#18706 = CARTESIAN_POINT ( 'NONE',  ( 20.63437500061451857, 5.824947211148865298E-16, -4.756430356249998326 ) ) ;
#18707 = CARTESIAN_POINT ( 'NONE',  ( 7.003125000614518036, -4.541064518000417216, -2.621784821875001281 ) ) ;
#18708 = CARTESIAN_POINT ( 'NONE',  ( 25.28437500061451715, 4.541064518000418104, 2.621784821874999949 ) ) ;
#18709 = CARTESIAN_POINT ( 'NONE',  ( -4.243569643749997233, 18.99687500061451928, 32.45002607614398471 ) ) ;
#18710 = CARTESIAN_POINT ( 'NONE',  ( 27.27187500061451431, -6.054752690667223547, -1.112240025338166033E-15 ) ) ;
#18711 = CARTESIAN_POINT ( 'NONE',  ( 7.987500000000000711, -2.886751345948129988, 4.999999999999997335 ) ) ;
#18712 = CARTESIAN_POINT ( 'NONE',  ( -2.000000000000000000, 13.28750000122903430, 26.53589838486224650 ) ) ;
#18713 = CARTESIAN_POINT ( 'NONE',  ( 14.05312500061451431, 0.000000000000000000, 5.243569643749999010 ) ) ;
#18714 = CARTESIAN_POINT ( 'NONE',  ( 6.412500001229036073, -4.330127018922190985, -2.500000000000001332 ) ) ;
#18715 = EDGE_CURVE ( 'NONE', #58973, #24462, #28593, .T. ) ;
#18716 = CARTESIAN_POINT ( 'NONE',  ( 16.84687500061451715, -3.027376345333614438, 5.243569643749998122 ) ) ;
#18717 = CARTESIAN_POINT ( 'NONE',  ( 11.07187500061451679, -6.054752690667223547, -1.112240025338166033E-15 ) ) ;
#18718 = DIRECTION ( 'NONE',  ( -1.000000000000000000, -0.000000000000000000, -0.000000000000000000 ) ) ;
#18719 = ORIENTED_EDGE ( 'NONE', *, *, #45399, .T. ) ;
#18720 = CARTESIAN_POINT ( 'NONE',  ( 13.04062500061451502, 6.054752690667223547, 3.707466751127219781E-16 ) ) ;
#18721 = DIRECTION ( 'NONE',  ( 0.000000000000000000, 0.000000000000000000, 1.000000000000000000 ) ) ;
#18722 = CARTESIAN_POINT ( 'NONE',  ( 23.51250000122903216, -4.330127018922190985, -2.500000000000001332 ) ) ;
#18723 = CARTESIAN_POINT ( 'NONE',  ( 13.88437500061451679, 6.421520780324663323E-16, -5.243569643749999010 ) ) ;
#18724 = CARTESIAN_POINT ( 'NONE',  ( 13.60312500061451679, 0.000000000000000000, 5.243569643749999010 ) ) ;
#18725 = CARTESIAN_POINT ( 'NONE',  ( 45.00000000000000000, 0.000000000000000000, 4.999999999999998224 ) ) ;
#18726 = CARTESIAN_POINT ( 'NONE',  ( 24.45937500061451786, 0.000000000000000000, 5.243569643749999010 ) ) ;
#18727 = CARTESIAN_POINT ( 'NONE',  ( 8.437500000000000000, -2.886751345948130876, 4.999999999999996447 ) ) ;
#18728 = CARTESIAN_POINT ( 'NONE',  ( 45.00000000000000000, 6.123233995736764310E-16, -4.999999999999998224 ) ) ;
#18729 = CARTESIAN_POINT ( 'NONE',  ( 3.096623204930365691, 4.278619418581859790, -3.076353068265403667 ) ) ;
#18730 = CARTESIAN_POINT ( 'NONE',  ( -4.243569643749998122, 15.84687500061451892, -27.54997392385601174 ) ) ;
#18731 = CARTESIAN_POINT ( 'NONE',  ( 14.74687500061451573, -3.027376345333610441, -5.243569643749999898 ) ) ;
#18732 = CARTESIAN_POINT ( 'NONE',  ( 18.71250000122903145, 4.330127018922192761, -2.499999999999997780 ) ) ;
#18733 = CARTESIAN_POINT ( 'NONE',  ( 11.40937500061451892, 0.000000000000000000, 5.243569643749999010 ) ) ;
#18734 = CARTESIAN_POINT ( 'NONE',  ( -2.121784821874999949, 19.27812500061451573, -33.67503911421598417 ) ) ;
#18735 = CARTESIAN_POINT ( 'NONE',  ( 21.00000000122903288, 5.773502691896255534, 3.535250795749688894E-16 ) ) ;
#18736 = CARTESIAN_POINT ( 'NONE',  ( 13.04062500061451502, 6.054752690667223547, 3.707466751127219781E-16 ) ) ;
#18737 = ORIENTED_EDGE ( 'NONE', *, *, #23644, .F. ) ;
#18738 = VERTEX_POINT ( 'NONE', #70113 ) ;
#18739 = CARTESIAN_POINT ( 'NONE',  ( 17.47499999999999787, -4.330127018922194537, 2.499999999999995559 ) ) ;
#18740 = CARTESIAN_POINT ( 'NONE',  ( 1.071796769724488785, 18.20134618820329919, 34.00000000000000000 ) ) ;
#18741 = CARTESIAN_POINT ( 'NONE',  ( 12.19687500061451857, 6.054752690667223547, 3.707466751127219781E-16 ) ) ;
#18742 = PLANE ( 'NONE',  #30308 ) ;
#18743 = CARTESIAN_POINT ( 'NONE',  ( 13.08750000122903323, -4.330127018922194537, 2.499999999999995559 ) ) ;
#18744 = CARTESIAN_POINT ( 'NONE',  ( 20.70000000122903216, -2.886751345948129988, 4.999999999999997335 ) ) ;
#18745 = CARTESIAN_POINT ( 'NONE',  ( 17.57812500061451644, 4.541064518000418104, 2.621784821874999949 ) ) ;
#18746 = CARTESIAN_POINT ( 'NONE',  ( 22.64062500061451644, -3.027376345333614438, 5.243569643749998122 ) ) ;
#18747 = CARTESIAN_POINT ( 'NONE',  ( 29.25000000122903288, -2.886751345948129988, 4.999999999999997335 ) ) ;
#18748 = CARTESIAN_POINT ( 'NONE',  ( 27.33750000000000213, -2.886751345948129988, 4.999999999999997335 ) ) ;
#18749 = CARTESIAN_POINT ( 'NONE',  ( 1.071796769724491893, 11.69509619066136885, 33.99999999999999289 ) ) ;
#18750 = CARTESIAN_POINT ( 'NONE',  ( 29.73750000000000071, -2.886751345948125991, -5.000000000000000000 ) ) ;
#18751 = FACE_OUTER_BOUND ( 'NONE', #6654, .T. ) ;
#18752 = DIRECTION ( 'NONE',  ( -1.000000000000000000, -0.000000000000000000, -0.000000000000000000 ) ) ;
#18753 = CARTESIAN_POINT ( 'NONE',  ( 9.001249775931846008E-16, 15.47187500061451892, -25.09994784771203058 ) ) ;
#18754 = CARTESIAN_POINT ( 'NONE',  ( 3.825000001229032609, 2.886751345948129099, -4.999999999999998224 ) ) ;
#18755 = CARTESIAN_POINT ( 'NONE',  ( 6.600000000000001421, 0.000000000000000000, 4.999999999999998224 ) ) ;
#18756 = ADVANCED_FACE ( 'NONE', ( #46865 ), #46499, .F. ) ;
#18757 = CARTESIAN_POINT ( 'NONE',  ( 3.684375000614518836, 4.541064518000418104, 2.621784821874999949 ) ) ;
#18758 = CARTESIAN_POINT ( 'NONE',  ( 10.92187500061451644, 3.027376345333611329, 5.243569643749999010 ) ) ;
#18759 = CARTESIAN_POINT ( 'NONE',  ( 27.44062500061451715, 6.054752690667223547, 3.707466751127219781E-16 ) ) ;
#18760 = CARTESIAN_POINT ( 'NONE',  ( -5.798826918071315895, 8.147596131390992369, -31.59132108569609443 ) ) ;
#18761 = CARTESIAN_POINT ( 'NONE',  ( 8.400000000000000355, 0.000000000000000000, 4.999999999999998224 ) ) ;
#18762 = CARTESIAN_POINT ( 'NONE',  ( 7.059375000614518392, -4.541064518000417216, -2.621784821875001281 ) ) ;
#18763 = CARTESIAN_POINT ( 'NONE',  ( 12.12187500061451573, 3.027376345333613106, -5.243569643749998122 ) ) ;
#18764 = CARTESIAN_POINT ( 'NONE',  ( 6.562500000000001776, 2.886751345948126879, 4.999999999999999112 ) ) ;
#18765 = CARTESIAN_POINT ( 'NONE',  ( -4.243569643749998122, 15.79062500061459495, 32.45002607614398471 ) ) ;
#18766 = CARTESIAN_POINT ( 'NONE',  ( 4.848412143738765501, -3.306759954282229685, 4.272523750749039451 ) ) ;
#18767 = CARTESIAN_POINT ( 'NONE',  ( 7.724999999999999645, 6.123233995736764310E-16, -4.999999999999998224 ) ) ;
#18768 = CARTESIAN_POINT ( 'NONE',  ( 14.85937500061451999, 2.746126346562643317, 4.756430356249998326 ) ) ;
#18769 = CARTESIAN_POINT ( 'NONE',  ( 19.97812500061451502, -4.541064518000419881, 2.621784821874995952 ) ) ;
#18770 = CARTESIAN_POINT ( 'NONE',  ( 13.15312500061451750, 0.000000000000000000, 5.243569643749999010 ) ) ;
#18771 = CARTESIAN_POINT ( 'NONE',  ( 26.59687500061451360, 0.000000000000000000, 4.756430356249998326 ) ) ;
#18772 = CARTESIAN_POINT ( 'NONE',  ( 8.409375000614518925, -4.541064518000417216, -2.621784821875001281 ) ) ;
#18773 = CARTESIAN_POINT ( 'NONE',  ( 27.15000000000000213, 4.330127018922192761, -2.499999999999997780 ) ) ;
#18774 = CARTESIAN_POINT ( 'NONE',  ( 23.25000000122903288, 5.773502691896255534, 3.535250795749688894E-16 ) ) ;
#18775 = CARTESIAN_POINT ( 'NONE',  ( 11.21250000122903501, 0.000000000000000000, 4.999999999999998224 ) ) ;
#18776 = CARTESIAN_POINT ( 'NONE',  ( 12.27187500061451786, 3.027376345333611329, 5.243569643749999010 ) ) ;
#18777 = CARTESIAN_POINT ( 'NONE',  ( 27.30937500061451573, -4.541064518000417216, -2.621784821875001281 ) ) ;
#18778 = ADVANCED_FACE ( 'NONE', ( #40594 ), #2165, .T. ) ;
#18779 = CARTESIAN_POINT ( 'NONE',  ( 21.95625000122903003, 0.000000000000000000, 4.999999999999998224 ) ) ;
#18780 = DIRECTION ( 'NONE',  ( -0.000000000000000000, -1.000000000000000000, -0.000000000000000000 ) ) ;
#18781 = CARTESIAN_POINT ( 'NONE',  ( 18.90937500061451360, 4.541064518000418104, -2.621784821874998173 ) ) ;
#18782 = CARTESIAN_POINT ( 'NONE',  ( 12.42187500061451821, -6.054752690667223547, -1.112240025338166033E-15 ) ) ;
#18783 = CARTESIAN_POINT ( 'NONE',  ( 3.756430356249998770, 17.21562499938548285, 32.16877607737302469 ) ) ;
#18784 = CARTESIAN_POINT ( 'NONE',  ( 26.88749999999999574, -2.886751345948129988, 4.999999999999997335 ) ) ;
#18785 = CARTESIAN_POINT ( 'NONE',  ( 3.756430356249998770, 19.80312499938548498, 32.16877607737302469 ) ) ;
#18786 = CARTESIAN_POINT ( 'NONE',  ( -4.243569643749999898, 11.27187500061451608, -32.45002607614398471 ) ) ;
#18787 = CARTESIAN_POINT ( 'NONE',  ( 28.17187500061451644, -5.492252693125287522, -1.008910452111647106E-15 ) ) ;
#18788 = CARTESIAN_POINT ( 'NONE',  ( 15.55312500061451608, -4.541064518000417216, -2.621784821875001281 ) ) ;
#18789 = CARTESIAN_POINT ( 'NONE',  ( 4.837500000000001243, -2.886751345948129988, 4.999999999999997335 ) ) ;
#18790 =( BOUNDED_SURFACE ( )  B_SPLINE_SURFACE ( 1, 2, ( 
 ( #38492, #54752, #66942, #3786, #60639, #48484, #61380, #48848, #43675, #4154, #71378, #43311, #15213, #49219, #16310, #60271, #9685, #21122, #66198, #15576, #61017, #21489, #10052, #27412, #32946, #4876, #49943, #44415, #72839, #56914, #5957, #39586, #12580, #46205, #11503, #51386, #11139, #51027, #50316, #62110, #63184, #28490, #28141, #788, #62824, #12216, #22221, #23297, #34383, #44775, #55847, #50669, #56212, #11862, #40665, #61738, #68021, #33668, #45128, #1151, #67310, #45847, #73, #68382, #17743, #51750, #5605, #40302, #16668, #34745, #17394, #45490, #423, #22579, #18103, #6319, #5235, #68745, #39951, #22931, #27777, #23660, #67662, #57277, #39226, #6686, #34025, #56562, #28848, #17028, #29214, #62464, #19562, #24018, #70184, #30301, #47291, #64643, #53193, #19191, #47652, #52834, #1514, #2234, #19931, #42485, #46933, #42118, #25108, #35114, #2589, #52471, #14028, #25484, #46567, #41744, #65008, #36568, #58353, #1879, #57637, #18471, #48030, #69111, #24385, #41035, #63550, #12936, #13661, #69471, #8493, #64272, #59088, #69826, #24748, #7043, #29573, #31025, #35472, #52110, #36203, #58721, #57994, #7403, #8134, #53559, #29931, #30660, #2956, #70556, #18828, #41391, #63904, #13293, #35830, #7764, #70923, #21394, #53937, #48760, #55028, #31767, #32493, #66473, #8861, #4432, #38027, #21031, #38396, #72018, #71284, #71658, #3696, #65740, #43584, #14758, #49852, #66105, #59825, #26221, #54304, #9231, #15125, #4063, #26960, #32126, #15484, #48395, #15850, #20663, #21758, #20293, #43950, #14396, #60550, #3333, #25858, #60920, #44319, #10323, #31397, #49487, #32856, #55392, #4786, #9957, #27320, #26589, #9594, #72378, #65370, #36934, #54660, #59454, #42848, #37302, #43220, #37662, #60185, #49130, #52295, #18287, #977, #67217, #35298, #72746, #16578, #41219, #16219, #2060, #5147, #50220, #6508, #34939, #6871, #30119, #66849, #57465, #1696, #24207, #46760, #12762, #39130, #69294, #7584, #29403, #63008, #24571, #13118, #22131, #57819, #44686, #7229, #51578, #68570, #40861, #62650, #29758, #12047, #18657, #55753, #63727, #12404, #51937, #35659, #58179, #1334, #52653, #23846, #33214, #46394, #38772, #61292, #29043, #10684, #27682, #34571, #57099, #23487, #46034, #17929, #40492, #68929, #63378, #8316, #64826, #8679, #2410, #30845, #70006, #54484, #26039, #9418, #3885, #48578, #9052, #2775, #37487, #47474, #31211, #47116, #31948, #64090, #14216, #47845, #69648, #64459, #13472, #25298, #60008, #36021, #19010, #41572, #13850, #41933, #37113, #42666, #30488, #71105, #36392, #24931, #3148, #14949, #58538, #48211, #70373, #53379, #7950, #53016, #19751, #65190, #19376, #42300, #58906, #36751, #59271, #53751, #25674, #14580, #54122, #3518, #70733, #59640, #20111, #31583, #20478, #43031, #65560, #55581, #11242, #32312, #38591, #54846, #15674, #44869, #20853, #16404, #43770, #67044, #38958, #22316, #49312, #61476, #37848, #10871, #61117, #16043, #72208, #26780, #61837, #27508, #33765, #33404, #55941, #50041, #5337, #10514, #21585, #21953, #4255, #33041, #44139, #27877, #50410, #60369, #9778, #4974, #38211, #71846, #72934, #72567, #32681, #21217, #67405, #66294, #60739, #16766, #48948, #56309, #10149, #55220, #4615, #66666, #44510, #26405, #71477, #39324, #43405, #65930, #15310, #27145, #49679, #7141, #63643, #23754, #28951, #45590, #13032, #62208, #18567, #67757, #68124, #17129, #11604, #39690, #57376, #23035, #52207, #62919, #46303, #40400, #45946, #35571, #5698, #29671, #34121, #28234, #68477, #29315, #56661, #51127, #12314, #68842, #6055, #34849, #35213, #23397, #45224, #28590, #57735, #50764, #69209, #1608, #524, #12676, #17489, #40051, #18199, #62563, #40770, #24119, #169, #63284, #51846, #6783, #46668, #41133, #11959, #1249, #34484, #57014, #22673, #6419, #51490, #890, #17839, #47389, #2326, #30400, #36305, #47752, #3054, #2688, #59183, #18925, #37027, #52929, #65469, #41485, #65104, #58090, #8592, #47029, #69564, #31497, #14860, #42576, #1976, #70647, #8963, #48492, #58452, #19659, #7498, #42943, #24485, #25204, #58819, #30026, #24842, #64005, #13763, #71016, #13385, #52569, #35930, #69919, #19289, #48124, #53662, #7864, #54037, #41843, #64372, #14126, #25952, #8230, #31122, #30758, #53289, #70287, #20394, #42214, #25585, #64738, #36664, #20022, #14493, #59552, #3432, #15222, #21496, #10423, #32954, #31862, #44049, #27058, #54397, #61388, #60279, #65839, #4529, #16318, #20761, #10061, #71388, #32225, #72476, #9329, #15952, #9692, #66573, #38500, #49951, #37761, #61026, #26318, #55491, #32593, #60646, #43682, #54759, #38871, #49588, #66950, #37399, #55131, #15583, #59923, #3796, #4163, #4885, #26693, #27420, #38125, #72112, #21862, #49226, #44423, #71760, #48857, #21129, #43319, #66205, #28780, #23954, #52767, #56847, #51321, #57209, #12517, #57576, #7698, #45419, #35048, #52405, #1813, #24321, #63486, #17679, #46869, #30235, #12874, #68681, #12153, #2170, #725, #58292, #34314, #34680, #6253, #23232, #45784, #46504, #62761, #18764, #29510, #63121, #6624, #35406, #52045, #57932, #40599, #11797, #6979, #67955, #17327, #29152, #7339, #29868, #39886, #69409, #51685, #41330, #35769, #68319, #1449, #40238, #1089, #69042, #18404, #23596, #46142, #18042, #62399, #63839, #40971, #13230, #26150, #59754, #53495, #15059, #25046, #59383, #54594, #9528, #41682, #64939, #25417, #24681, #42053, #64205, #2887, #37597, #13593, #47228, #69760, #64575, #19495, #14689, #20225, #8065, #48690, #13964, #2525, #53870, #65670, #36139, #25790, #47961, #8423, #19128, #60118, #70489, #42779, #53126, #19866, #58658, #30959, #32060, #42419, #70118, #65299, #31696, #54231, #30599, #37231, #3261, #47589, #36501, #59022, #14330, #48327, #36865, #8794, #31327, #70852, #9161, #43148, #3628, #71214 ),
 ( #20591, #60481, #67153, #60855, #4722, #50153, #9889, #22065, #26895, #61580, #66040, #32424, #26523, #15418, #49061, #3996, #43883, #71954, #16513, #72683, #54961, #27985, #21330, #4366, #33151, #44972, #20962, #5084, #27256, #10259, #33871, #67510, #32791, #44623, #49421, #72314, #71589, #55328, #11353, #49789, #66409, #39066, #10983, #33504, #43517, #56053, #55688, #37961, #15785, #38327, #21695, #27619, #61949, #44252, #16155, #66783, #38707, #22425, #61227, #5445, #10621, #50515, #73042, #16874, #39429, #24864, #67868, #41864, #18947, #47051, #30050, #56761, #19682, #58474, #42235, #70309, #69585, #52590, #64760, #2711, #11711, #2347, #39800, #47411, #40156, #57121, #30422, #62316, #69941, #6166, #64394, #45333, #34228, #5805, #1996, #17597, #19311, #41506, #13784, #24507, #22781, #64026, #14150, #56414, #68233, #36326, #58841, #28335, #8251, #638, #30781, #47773, #17240, #13405, #28695, #62676, #35953, #7886, #51234, #12070, #23146, #50873, #53312, #271, #45700, #25227, #34593, #7519, #52950, #37049, #71410, #66598, #21517, #53684, #3820, #37422, #36685, #54060, #3079, #65493, #49610, #31143, #42964, #44071, #9352, #8987, #32247, #43705, #66226, #25607, #54780, #15245, #48145, #59206, #31519, #59574, #65863, #8614, #42600, #48880, #65126, #25973, #55152, #70669, #26714, #59945, #43341, #60302, #20416, #3455, #4186, #20045, #21151, #20785, #26341, #31885, #48514, #72137, #37782, #14516, #71041, #9713, #54419, #14883, #4550, #49248, #71783, #15605, #38146, #60670, #10084, #32614, #27079, #34054, #38893, #455, #4908, #72499, #38524, #33697, #50345, #56594, #101, #28520, #11173, #55515, #56244, #822, #23330, #27811, #51060, #5990, #15974, #22964, #33340, #45525, #6350, #27444, #22607, #49974, #72869, #5635, #50699, #44444, #22252, #61411, #45880, #68055, #51421, #61047, #17424, #39983, #44806, #28881, #16338, #45159, #10445, #32975, #21884, #28172, #16699, #66973, #55878, #10805, #67339, #5265, #39257, #61769, #67691, #17062, #39622, #62495, #11534, #62140, #11893, #34418, #56946, #24418, #36239, #12249, #69503, #18503, #52142, #25141, #58753, #24055, #63940, #23690, #63582, #18863, #1545, #68778, #35864, #68412, #57313, #51782, #46967, #2620, #6717, #1182, #7077, #35507, #7436, #30692, #17774, #58026, #2265, #24779, #47323, #13325, #40701, #69856, #53223, #58387, #41068, #35148, #40334, #46238, #8163, #29250, #57671, #18134, #63219, #12614, #41424, #29606, #41777, #52503, #7800, #29962, #1914, #62855, #34780, #19223, #46602, #69144, #30337, #52865, #12969, #64306, #13696, #15156, #53593, #31798, #4099, #65403, #14060, #2988, #26627, #47682, #38060, #43618, #31056, #54695, #36599, #8898, #37693, #65038, #65774, #49164, #42148, #60216, #71320, #54336, #71695, #32162, #31430, #3730, #36964, #25889, #26255, #48061, #9994, #48792, #19962, #59486, #14429, #42514, #48429, #37336, #9629, #14794, #20695, #8527, #21067, #53970, #55065, #25516, #66140, #70955, #20326, #15518, #3368, #60585, #4466, #32528, #64675, #70218, #19592, #59120, #70586, #43254, #42880, #59859, #9263, #22524, #4821, #11081, #44717, #67608, #62055, #60957, #38433, #33609, #16252, #10359, #11450, #44359, #368, #56153, #45071, #61682, #67253, #11811, #34328, #28435, #55429, #49525, #16611, #50613, #27355, #72411, #5547, #16973, #32889, #28085, #56509, #39167, #66506, #49886, #5902, #26996, #17340, #22876, #21793, #33970, #15887, #61323, #39530, #66885, #50972, #45434, #21428, #67967, #17, #39899, #62412, #56860, #10721, #72050, #38808, #5181, #43985, #33253, #55791, #27719, #50258, #72782, #22165, #51698, #57590, #69057, #24333, #23969, #7352, #40253, #58304, #1102, #13607, #62774, #13243, #6993, #52059, #69421, #23610, #52780, #36152, #63852, #23246, #18776, #30247, #41342, #46882, #29881, #7714, #18418, #1463, #1825, #57223, #63499, #46517, #35780, #2182, #12165, #17692, #12887, #68695, #34694, #24695, #52419, #12530, #6637, #29166, #28794, #40984, #40614, #47239, #35420, #69772, #57945, #45797, #19140, #64218, #6266, #18055, #41694, #51335, #737, #68332, #46155, #63135, #35063, #29524, #65314, #19509, #19879, #3276, #20241, #13976, #42432, #8437, #66052, #37610, #20978, #15430, #65685, #15073, #3643, #30973, #60132, #43531, #26166, #8807, #25432, #58671, #42065, #71603, #47601, #47974, #70131, #64588, #36514, #37248, #2901, #32075, #42793, #48706, #14704, #25804, #8079, #30610, #9541, #59035, #53139, #48342, #9176, #53508, #70502, #59769, #71229, #64953, #31711, #54607, #70867, #25058, #14345, #4012, #2538, #49076, #26536, #36879, #59397, #31344, #53884, #20608, #54246, #43166, #16889, #32439, #28000, #61597, #44637, #61964, #22438, #21708, #22078, #27270, #16169, #67166, #38341, #287, #16527, #10272, #49803, #55341, #32804, #38720, #27633, #56068, #55703, #39079, #71969, #39443, #4736, #45348, #21343, #44987, #61241, #10634, #50529, #72328, #11367, #67882, #67524, #54975, #73057, #33885, #56429, #5460, #10998, #5819, #50167, #33165, #33518, #15800, #28350, #5097, #50887, #22795, #43898, #49435, #37975, #44266, #66422, #60496, #4380, #72696, #9902, #66798, #26909, #60869, #652, #68971, #24610, #28710, #23160, #29080, #57506, #29439, #52693, #17254, #6908, #24249, #34607, #35336, #69334, #11726, #7268, #40901, #23885, #41256, #1735, #1016, #1375, #6546, #68607, #46432, #17611, #2099, #18328, #62690, #51615, #57137, #12086, #17968, #51976, #57859, #34977, #63414, #51249, #18692, #23522, #47157, #45714, #46797, #40529, #63045, #29797, #46072, #63768, #39814, #13156, #34242, #52333, #35698, #58218, #7623, #12800, #30160, #62330, #12446, #56775, #68248, #6181, #40171, #37157, #31627, #30528, #7992, #53794, #58946, #53055, #54161, #36065, #19793, #3557, #25343, #69689, #58585, #2449, #48254 ) ),
 .UNSPECIFIED., .F., .F., .F. ) 
 B_SPLINE_SURFACE_WITH_KNOTS ( ( 2, 2 ),
 ( 3, 2, 2, 2, 2, 2, 2, 2, 2, 2, 2, 2, 2, 2, 2, 2, 2, 2, 2, 2, 2, 2, 2, 2, 2, 2, 2, 2, 2, 2, 2, 2, 2, 2, 2, 2, 2, 2, 2, 2, 2, 2, 2, 2, 2, 2, 2, 2, 2, 2, 2, 2, 2, 2, 2, 2, 2, 2, 2, 2, 2, 2, 2, 2, 2, 2, 2, 2, 2, 2, 2, 2, 2, 2, 2, 2, 2, 2, 2, 2, 2, 2, 2, 2, 2, 2, 2, 2, 2, 2, 2, 2, 2, 2, 2, 2, 2, 2, 2, 2, 2, 2, 2, 2, 2, 2, 2, 2, 2, 2, 2, 2, 2, 2, 2, 2, 2, 2, 2, 2, 2, 2, 2, 2, 2, 2, 2, 2, 2, 2, 2, 2, 2, 2, 2, 2, 2, 2, 2, 2, 2, 2, 2, 2, 2, 2, 2, 2, 2, 2, 2, 2, 2, 2, 2, 2, 2, 2, 2, 2, 2, 2, 2, 2, 2, 2, 2, 2, 2, 2, 2, 2, 2, 2, 2, 2, 2, 2, 2, 2, 2, 2, 2, 2, 2, 2, 2, 2, 2, 2, 2, 2, 2, 2, 2, 2, 2, 2, 2, 2, 2, 2, 2, 2, 2, 2, 2, 2, 2, 2, 2, 2, 2, 2, 2, 2, 2, 2, 2, 2, 2, 2, 2, 2, 2, 2, 2, 2, 2, 2, 2, 2, 2, 2, 2, 2, 2, 2, 2, 2, 2, 2, 2, 2, 2, 2, 2, 2, 2, 2, 2, 2, 2, 2, 2, 2, 2, 2, 2, 2, 2, 2, 2, 2, 2, 2, 2, 2, 2, 2, 2, 2, 2, 2, 2, 2, 2, 2, 2, 2, 2, 2, 2, 2, 2, 2, 2, 2, 2, 2, 2, 2, 2, 2, 2, 2, 2, 2, 2, 2, 2, 2, 2, 2, 2, 2, 2, 2, 2, 2, 2, 2, 2, 2, 2, 2, 2, 2, 2, 2, 2, 2, 2, 2, 2, 2, 2, 2, 2, 2, 2, 2, 2, 2, 2, 2, 2, 2, 2, 2, 2, 2, 2, 2, 2, 2, 2, 2, 2, 2, 2, 2, 2, 2, 2, 2, 2, 2, 2, 2, 3 ),
 ( 0.000000000000000000, 1.000000000000000000 ),
 ( 0.000000000000000000, 0.002777777777777777884, 0.005555555555555555768, 0.008333333333333333218, 0.01111111111111111154, 0.01388888888888888812, 0.01666666666666666644, 0.01944444444444444475, 0.02222222222222222307, 0.02500000000000000139, 0.02777777777777777624, 0.03055555555555555455, 0.03333333333333333287, 0.03611111111111110772, 0.03888888888888888951, 0.04166666666666666435, 0.04444444444444444614, 0.04722222222222222099, 0.05000000000000000278, 0.05277777777777777762, 0.05555555555555555247, 0.05833333333333333426, 0.06111111111111110911, 0.06388888888888888395, 0.06666666666666666574, 0.06944444444444444753, 0.07222222222222221544, 0.07499999999999999722, 0.07777777777777777901, 0.08055555555555556080, 0.08333333333333332871, 0.08611111111111111049, 0.08888888888888889228, 0.09166666666666666019, 0.09444444444444444198, 0.09722222222222222376, 0.1000000000000000056, 0.1027777777777777735, 0.1055555555555555552, 0.1083333333333333370, 0.1111111111111111049, 0.1138888888888888867, 0.1166666666666666685, 0.1194444444444444503, 0.1222222222222222182, 0.1250000000000000000, 0.1277777777777777679, 0.1305555555555555636, 0.1333333333333333315, 0.1361111111111110994, 0.1388888888888888951, 0.1416666666666666630, 0.1444444444444444309, 0.1472222222222222265, 0.1499999999999999944, 0.1527777777777777901, 0.1555555555555555580, 0.1583333333333333259, 0.1611111111111111216, 0.1638888888888888895, 0.1666666666666666574, 0.1694444444444444531, 0.1722222222222222210, 0.1749999999999999889, 0.1777777777777777846, 0.1805555555555555525, 0.1833333333333333204, 0.1861111111111111160, 0.1888888888888888840, 0.1916666666666666796, 0.1944444444444444475, 0.1972222222222222154, 0.2000000000000000111, 0.2027777777777777790, 0.2055555555555555469, 0.2083333333333333426, 0.2111111111111111105, 0.2138888888888888784, 0.2166666666666666741, 0.2194444444444444420, 0.2222222222222222099, 0.2250000000000000056, 0.2277777777777777735, 0.2305555555555555691, 0.2333333333333333370, 0.2361111111111111049, 0.2388888888888889006, 0.2416666666666666685, 0.2444444444444444364, 0.2472222222222222321, 0.2500000000000000000, 0.2527777777777777679, 0.2555555555555555358, 0.2583333333333333592, 0.2611111111111111271, 0.2638888888888888951, 0.2666666666666666630, 0.2694444444444444309, 0.2722222222222221988, 0.2750000000000000222, 0.2777777777777777901, 0.2805555555555555580, 0.2833333333333333259, 0.2861111111111110938, 0.2888888888888888618, 0.2916666666666666852, 0.2944444444444444531, 0.2972222222222222210, 0.2999999999999999889, 0.3027777777777777568, 0.3055555555555555802, 0.3083333333333333481, 0.3111111111111111160, 0.3138888888888888840, 0.3166666666666666519, 0.3194444444444444198, 0.3222222222222222432, 0.3250000000000000111, 0.3277777777777777790, 0.3305555555555555469, 0.3333333333333333148, 0.3361111111111111382, 0.3388888888888889062, 0.3416666666666666741, 0.3444444444444444420, 0.3472222222222222099, 0.3499999999999999778, 0.3527777777777778012, 0.3555555555555555691, 0.3583333333333333370, 0.3611111111111111049, 0.3638888888888888729, 0.3666666666666666408, 0.3694444444444444642, 0.3722222222222222321, 0.3750000000000000000, 0.3777777777777777679, 0.3805555555555555358, 0.3833333333333333592, 0.3861111111111111271, 0.3888888888888888951, 0.3916666666666666630, 0.3944444444444444309, 0.3972222222222221988, 0.4000000000000000222, 0.4027777777777777901, 0.4055555555555555580, 0.4083333333333333259, 0.4111111111111110938, 0.4138888888888888618, 0.4166666666666666852, 0.4194444444444444531, 0.4222222222222222210, 0.4249999999999999889, 0.4277777777777777568, 0.4305555555555555802, 0.4333333333333333481, 0.4361111111111111160, 0.4388888888888888840, 0.4416666666666666519, 0.4444444444444444198, 0.4472222222222222432, 0.4500000000000000111, 0.4527777777777777790, 0.4555555555555555469, 0.4583333333333333148, 0.4611111111111111382, 0.4638888888888889062, 0.4666666666666666741, 0.4694444444444444420, 0.4722222222222222099, 0.4749999999999999778, 0.4777777777777778012, 0.4805555555555555691, 0.4833333333333333370, 0.4861111111111111049, 0.4888888888888888729, 0.4916666666666666408, 0.4944444444444444642, 0.4972222222222222321, 0.5000000000000000000, 0.5027777777777777679, 0.5055555555555555358, 0.5083333333333333037, 0.5111111111111110716, 0.5138888888888888395, 0.5166666666666667185, 0.5194444444444444864, 0.5222222222222222543, 0.5250000000000000222, 0.5277777777777777901, 0.5305555555555555580, 0.5333333333333333259, 0.5361111111111110938, 0.5388888888888888618, 0.5416666666666666297, 0.5444444444444443976, 0.5472222222222222765, 0.5500000000000000444, 0.5527777777777778123, 0.5555555555555555802, 0.5583333333333333481, 0.5611111111111111160, 0.5638888888888888840, 0.5666666666666666519, 0.5694444444444444198, 0.5722222222222221877, 0.5749999999999999556, 0.5777777777777777235, 0.5805555555555556024, 0.5833333333333333703, 0.5861111111111111382, 0.5888888888888889062, 0.5916666666666666741, 0.5944444444444444420, 0.5972222222222222099, 0.5999999999999999778, 0.6027777777777777457, 0.6055555555555555136, 0.6083333333333332815, 0.6111111111111111605, 0.6138888888888889284, 0.6166666666666666963, 0.6194444444444444642, 0.6222222222222222321, 0.6250000000000000000, 0.6277777777777777679, 0.6305555555555555358, 0.6333333333333333037, 0.6361111111111110716, 0.6388888888888888395, 0.6416666666666667185, 0.6444444444444444864, 0.6472222222222222543, 0.6500000000000000222, 0.6527777777777777901, 0.6555555555555555580, 0.6583333333333333259, 0.6611111111111110938, 0.6638888888888888618, 0.6666666666666666297, 0.6694444444444443976, 0.6722222222222222765, 0.6750000000000000444, 0.6777777777777778123, 0.6805555555555555802, 0.6833333333333333481, 0.6861111111111111160, 0.6888888888888888840, 0.6916666666666666519, 0.6944444444444444198, 0.6972222222222221877, 0.6999999999999999556, 0.7027777777777777235, 0.7055555555555556024, 0.7083333333333333703, 0.7111111111111111382, 0.7138888888888889062, 0.7166666666666666741, 0.7194444444444444420, 0.7222222222222222099, 0.7249999999999999778, 0.7277777777777777457, 0.7305555555555555136, 0.7333333333333332815, 0.7361111111111111605, 0.7388888888888889284, 0.7416666666666666963, 0.7444444444444444642, 0.7472222222222222321, 0.7500000000000000000, 0.7527777777777777679, 0.7555555555555555358, 0.7583333333333333037, 0.7611111111111110716, 0.7638888888888888395, 0.7666666666666667185, 0.7694444444444444864, 0.7722222222222222543, 0.7750000000000000222, 0.7777777777777777901, 0.7805555555555555580, 0.7833333333333333259, 0.7861111111111110938, 0.7888888888888888618, 0.7916666666666666297, 0.7944444444444443976, 0.7972222222222222765, 0.8000000000000000444, 0.8027777777777778123, 0.8055555555555555802, 0.8083333333333333481, 0.8111111111111111160, 0.8138888888888888840, 0.8166666666666666519, 0.8194444444444444198, 0.8222222222222221877, 0.8249999999999999556, 0.8277777777777777235, 0.8305555555555556024, 0.8333333333333333703, 0.8361111111111111382, 0.8388888888888889062, 0.8416666666666666741, 0.8444444444444444420, 0.8472222222222222099, 0.8499999999999999778, 0.8527777777777777457, 0.8555555555555555136, 0.8583333333333332815, 0.8611111111111111605, 0.8638888888888889284, 0.8666666666666666963, 0.8694444444444444642, 0.8722222222222222321, 0.8750000000000000000, 0.8777777777777777679, 0.8805555555555555358, 0.8833333333333333037, 0.8861111111111110716, 0.8888888888888888395, 0.8916666666666667185, 0.8944444444444444864, 0.8972222222222222543, 0.9000000000000000222, 0.9027777777777777901, 0.9055555555555555580, 0.9083333333333333259, 0.9111111111111110938, 0.9138888888888888618, 0.9166666666666666297, 0.9194444444444443976, 0.9222222222222222765, 0.9250000000000000444, 0.9277777777777778123, 0.9305555555555555802, 0.9333333333333333481, 0.9361111111111111160, 0.9388888888888888840, 0.9416666666666666519, 0.9444444444444444198, 0.9472222222222221877, 0.9499999999999999556, 0.9527777777777777235, 0.9555555555555556024, 0.9583333333333333703, 0.9611111111111111382, 0.9638888888888889062, 0.9666666666666666741, 0.9694444444444444420, 0.9722222222222222099, 0.9749999999999999778, 0.9777777777777777457, 0.9805555555555555136, 0.9833333333333332815, 0.9861111111111111605, 0.9888888888888889284, 0.9916666666666666963, 0.9944444444444444642, 0.9972222222222222321, 1.000000000000000000 ),
 .UNSPECIFIED. ) 
 GEOMETRIC_REPRESENTATION_ITEM ( )  RATIONAL_B_SPLINE_SURFACE ( (
 ( 1.000000000000000000, 0.8660254037844387076, 1.000000000000000000, 0.8660254037844387076, 1.000000000000000000, 0.8660254037844387076, 1.000000000000000000, 0.8660254037844387076, 1.000000000000000000, 0.8660254037844387076, 1.000000000000000000, 0.8660254037844387076, 1.000000000000000000, 0.8660254037844387076, 1.000000000000000000, 0.8660254037844387076, 1.000000000000000000, 0.8660254037844387076, 1.000000000000000000, 0.8660254037844387076, 1.000000000000000000, 0.8660254037844387076, 1.000000000000000000, 0.8660254037844387076, 1.000000000000000000, 0.8660254037844387076, 1.000000000000000000, 0.8660254037844387076, 1.000000000000000000, 0.8660254037844387076, 1.000000000000000000, 0.8660254037844387076, 1.000000000000000000, 0.8660254037844387076, 1.000000000000000000, 0.8660254037844387076, 1.000000000000000000, 0.8660254037844387076, 1.000000000000000000, 0.8660254037844387076, 1.000000000000000000, 0.8660254037844387076, 1.000000000000000000, 0.8660254037844387076, 1.000000000000000000, 0.8660254037844387076, 1.000000000000000000, 0.8660254037844387076, 1.000000000000000000, 0.8660254037844387076, 1.000000000000000000, 0.8660254037844387076, 1.000000000000000000, 0.8660254037844387076, 1.000000000000000000, 0.8660254037844387076, 1.000000000000000000, 0.8660254037844387076, 1.000000000000000000, 0.8660254037844387076, 1.000000000000000000, 0.8660254037844387076, 1.000000000000000000, 0.8660254037844387076, 1.000000000000000000, 0.8660254037844387076, 1.000000000000000000, 0.8660254037844387076, 1.000000000000000000, 0.8660254037844387076, 1.000000000000000000, 0.8660254037844387076, 1.000000000000000000, 0.8660254037844387076, 1.000000000000000000, 0.8660254037844387076, 1.000000000000000000, 0.8660254037844387076, 1.000000000000000000, 0.8660254037844387076, 1.000000000000000000, 0.8660254037844387076, 1.000000000000000000, 0.8660254037844387076, 1.000000000000000000, 0.8660254037844387076, 1.000000000000000000, 0.8660254037844387076, 1.000000000000000000, 0.8660254037844387076, 1.000000000000000000, 0.8660254037844387076, 1.000000000000000000, 0.8660254037844387076, 1.000000000000000000, 0.8660254037844387076, 1.000000000000000000, 0.8660254037844387076, 1.000000000000000000, 0.8660254037844387076, 1.000000000000000000, 0.8660254037844387076, 1.000000000000000000, 0.8660254037844387076, 1.000000000000000000, 0.8660254037844387076, 1.000000000000000000, 0.8660254037844387076, 1.000000000000000000, 0.8660254037844387076, 1.000000000000000000, 0.8660254037844387076, 1.000000000000000000, 0.8660254037844387076, 1.000000000000000000, 0.8660254037844387076, 1.000000000000000000, 0.8660254037844387076, 1.000000000000000000, 0.8660254037844387076, 1.000000000000000000, 0.8660254037844387076, 1.000000000000000000, 0.8660254037844387076, 1.000000000000000000, 0.8660254037844387076, 1.000000000000000000, 0.8660254037844387076, 1.000000000000000000, 0.8660254037844387076, 1.000000000000000000, 0.8660254037844387076, 1.000000000000000000, 0.8660254037844387076, 1.000000000000000000, 0.8660254037844387076, 1.000000000000000000, 0.8660254037844387076, 1.000000000000000000, 0.8660254037844387076, 1.000000000000000000, 0.8660254037844387076, 1.000000000000000000, 0.8660254037844387076, 1.000000000000000000, 0.8660254037844387076, 1.000000000000000000, 0.8660254037844387076, 1.000000000000000000, 0.8660254037844387076, 1.000000000000000000, 0.8660254037844387076, 1.000000000000000000, 0.8660254037844387076, 1.000000000000000000, 0.8660254037844387076, 1.000000000000000000, 0.8660254037844387076, 1.000000000000000000, 0.8660254037844387076, 1.000000000000000000, 0.8660254037844387076, 1.000000000000000000, 0.8660254037844387076, 1.000000000000000000, 0.8660254037844387076, 1.000000000000000000, 0.8660254037844387076, 1.000000000000000000, 0.8660254037844387076, 1.000000000000000000, 0.8660254037844387076, 1.000000000000000000, 0.8660254037844387076, 1.000000000000000000, 0.8660254037844387076, 1.000000000000000000, 0.8660254037844387076, 1.000000000000000000, 0.8660254037844387076, 1.000000000000000000, 0.8660254037844387076, 1.000000000000000000, 0.8660254037844387076, 1.000000000000000000, 0.8660254037844387076, 1.000000000000000000, 0.8660254037844387076, 1.000000000000000000, 0.8660254037844387076, 1.000000000000000000, 0.8660254037844387076, 1.000000000000000000, 0.8660254037844387076, 1.000000000000000000, 0.8660254037844387076, 1.000000000000000000, 0.8660254037844387076, 1.000000000000000000, 0.8660254037844387076, 1.000000000000000000, 0.8660254037844387076, 1.000000000000000000, 0.8660254037844387076, 1.000000000000000000, 0.8660254037844387076, 1.000000000000000000, 0.8660254037844387076, 1.000000000000000000, 0.8660254037844387076, 1.000000000000000000, 0.8660254037844387076, 1.000000000000000000, 0.8660254037844387076, 1.000000000000000000, 0.8660254037844387076, 1.000000000000000000, 0.8660254037844387076, 1.000000000000000000, 0.8660254037844387076, 1.000000000000000000, 0.8660254037844387076, 1.000000000000000000, 0.8660254037844387076, 1.000000000000000000, 0.8660254037844387076, 1.000000000000000000, 0.8660254037844387076, 1.000000000000000000, 0.8660254037844387076, 1.000000000000000000, 0.8660254037844387076, 1.000000000000000000, 0.8660254037844387076, 1.000000000000000000, 0.8660254037844387076, 1.000000000000000000, 0.8660254037844387076, 1.000000000000000000, 0.8660254037844387076, 1.000000000000000000, 0.8660254037844387076, 1.000000000000000000, 0.8660254037844387076, 1.000000000000000000, 0.8660254037844387076, 1.000000000000000000, 0.8660254037844387076, 1.000000000000000000, 0.8660254037844387076, 1.000000000000000000, 0.8660254037844387076, 1.000000000000000000, 0.8660254037844387076, 1.000000000000000000, 0.8660254037844387076, 1.000000000000000000, 0.8660254037844387076, 1.000000000000000000, 0.8660254037844387076, 1.000000000000000000, 0.8660254037844387076, 1.000000000000000000, 0.8660254037844387076, 1.000000000000000000, 0.8660254037844387076, 1.000000000000000000, 0.8660254037844387076, 1.000000000000000000, 0.8660254037844387076, 1.000000000000000000, 0.8660254037844387076, 1.000000000000000000, 0.8660254037844387076, 1.000000000000000000, 0.8660254037844387076, 1.000000000000000000, 0.8660254037844387076, 1.000000000000000000, 0.8660254037844387076, 1.000000000000000000, 0.8660254037844387076, 1.000000000000000000, 0.8660254037844387076, 1.000000000000000000, 0.8660254037844387076, 1.000000000000000000, 0.8660254037844387076, 1.000000000000000000, 0.8660254037844387076, 1.000000000000000000, 0.8660254037844387076, 1.000000000000000000, 0.8660254037844387076, 1.000000000000000000, 0.8660254037844387076, 1.000000000000000000, 0.8660254037844387076, 1.000000000000000000, 0.8660254037844387076, 1.000000000000000000, 0.8660254037844387076, 1.000000000000000000, 0.8660254037844387076, 1.000000000000000000, 0.8660254037844387076, 1.000000000000000000, 0.8660254037844387076, 1.000000000000000000, 0.8660254037844387076, 1.000000000000000000, 0.8660254037844387076, 1.000000000000000000, 0.8660254037844387076, 1.000000000000000000, 0.8660254037844387076, 1.000000000000000000, 0.8660254037844387076, 1.000000000000000000, 0.8660254037844387076, 1.000000000000000000, 0.8660254037844387076, 1.000000000000000000, 0.8660254037844387076, 1.000000000000000000, 0.8660254037844387076, 1.000000000000000000, 0.8660254037844387076, 1.000000000000000000, 0.8660254037844387076, 1.000000000000000000, 0.8660254037844387076, 1.000000000000000000, 0.8660254037844387076, 1.000000000000000000, 0.8660254037844387076, 1.000000000000000000, 0.8660254037844387076, 1.000000000000000000, 0.8660254037844387076, 1.000000000000000000, 0.8660254037844387076, 1.000000000000000000, 0.8660254037844387076, 1.000000000000000000, 0.8660254037844387076, 1.000000000000000000, 0.8660254037844387076, 1.000000000000000000, 0.8660254037844387076, 1.000000000000000000, 0.8660254037844387076, 1.000000000000000000, 0.8660254037844387076, 1.000000000000000000, 0.8660254037844387076, 1.000000000000000000, 0.8660254037844387076, 1.000000000000000000, 0.8660254037844387076, 1.000000000000000000, 0.8660254037844387076, 1.000000000000000000, 0.8660254037844387076, 1.000000000000000000, 0.8660254037844387076, 1.000000000000000000, 0.8660254037844387076, 1.000000000000000000, 0.8660254037844387076, 1.000000000000000000, 0.8660254037844387076, 1.000000000000000000, 0.8660254037844387076, 1.000000000000000000, 0.8660254037844387076, 1.000000000000000000, 0.8660254037844387076, 1.000000000000000000, 0.8660254037844387076, 1.000000000000000000, 0.8660254037844387076, 1.000000000000000000, 0.8660254037844387076, 1.000000000000000000, 0.8660254037844387076, 1.000000000000000000, 0.8660254037844387076, 1.000000000000000000, 0.8660254037844387076, 1.000000000000000000, 0.8660254037844387076, 1.000000000000000000, 0.8660254037844387076, 1.000000000000000000, 0.8660254037844387076, 1.000000000000000000, 0.8660254037844387076, 1.000000000000000000, 0.8660254037844387076, 1.000000000000000000, 0.8660254037844387076, 1.000000000000000000, 0.8660254037844387076, 1.000000000000000000, 0.8660254037844387076, 1.000000000000000000, 0.8660254037844387076, 1.000000000000000000, 0.8660254037844387076, 1.000000000000000000, 0.8660254037844387076, 1.000000000000000000, 0.8660254037844387076, 1.000000000000000000, 0.8660254037844387076, 1.000000000000000000, 0.8660254037844387076, 1.000000000000000000, 0.8660254037844387076, 1.000000000000000000, 0.8660254037844387076, 1.000000000000000000, 0.8660254037844387076, 1.000000000000000000, 0.8660254037844387076, 1.000000000000000000, 0.8660254037844387076, 1.000000000000000000, 0.8660254037844387076, 1.000000000000000000, 0.8660254037844387076, 1.000000000000000000, 0.8660254037844387076, 1.000000000000000000, 0.8660254037844387076, 1.000000000000000000, 0.8660254037844387076, 1.000000000000000000, 0.8660254037844387076, 1.000000000000000000, 0.8660254037844387076, 1.000000000000000000, 0.8660254037844387076, 1.000000000000000000, 0.8660254037844387076, 1.000000000000000000, 0.8660254037844387076, 1.000000000000000000, 0.8660254037844387076, 1.000000000000000000, 0.8660254037844387076, 1.000000000000000000, 0.8660254037844387076, 1.000000000000000000, 0.8660254037844387076, 1.000000000000000000, 0.8660254037844387076, 1.000000000000000000, 0.8660254037844387076, 1.000000000000000000, 0.8660254037844387076, 1.000000000000000000, 0.8660254037844387076, 1.000000000000000000, 0.8660254037844387076, 1.000000000000000000, 0.8660254037844387076, 1.000000000000000000, 0.8660254037844387076, 1.000000000000000000, 0.8660254037844387076, 1.000000000000000000, 0.8660254037844387076, 1.000000000000000000, 0.8660254037844387076, 1.000000000000000000, 0.8660254037844387076, 1.000000000000000000, 0.8660254037844387076, 1.000000000000000000, 0.8660254037844387076, 1.000000000000000000, 0.8660254037844387076, 1.000000000000000000, 0.8660254037844387076, 1.000000000000000000, 0.8660254037844387076, 1.000000000000000000, 0.8660254037844387076, 1.000000000000000000, 0.8660254037844387076, 1.000000000000000000, 0.8660254037844387076, 1.000000000000000000, 0.8660254037844387076, 1.000000000000000000, 0.8660254037844387076, 1.000000000000000000, 0.8660254037844387076, 1.000000000000000000, 0.8660254037844387076, 1.000000000000000000, 0.8660254037844387076, 1.000000000000000000, 0.8660254037844387076, 1.000000000000000000, 0.8660254037844387076, 1.000000000000000000, 0.8660254037844387076, 1.000000000000000000, 0.8660254037844387076, 1.000000000000000000, 0.8660254037844387076, 1.000000000000000000, 0.8660254037844387076, 1.000000000000000000, 0.8660254037844387076, 1.000000000000000000, 0.8660254037844387076, 1.000000000000000000, 0.8660254037844387076, 1.000000000000000000, 0.8660254037844387076, 1.000000000000000000, 0.8660254037844387076, 1.000000000000000000, 0.8660254037844387076, 1.000000000000000000, 0.8660254037844387076, 1.000000000000000000, 0.8660254037844387076, 1.000000000000000000, 0.8660254037844387076, 1.000000000000000000, 0.8660254037844387076, 1.000000000000000000, 0.8660254037844387076, 1.000000000000000000, 0.8660254037844387076, 1.000000000000000000, 0.8660254037844387076, 1.000000000000000000, 0.8660254037844387076, 1.000000000000000000, 0.8660254037844387076, 1.000000000000000000, 0.8660254037844387076, 1.000000000000000000, 0.8660254037844387076, 1.000000000000000000, 0.8660254037844387076, 1.000000000000000000, 0.8660254037844387076, 1.000000000000000000, 0.8660254037844387076, 1.000000000000000000, 0.8660254037844387076, 1.000000000000000000, 0.8660254037844387076, 1.000000000000000000, 0.8660254037844387076, 1.000000000000000000, 0.8660254037844387076, 1.000000000000000000, 0.8660254037844387076, 1.000000000000000000, 0.8660254037844387076, 1.000000000000000000, 0.8660254037844387076, 1.000000000000000000, 0.8660254037844387076, 1.000000000000000000, 0.8660254037844387076, 1.000000000000000000, 0.8660254037844387076, 1.000000000000000000, 0.8660254037844387076, 1.000000000000000000, 0.8660254037844387076, 1.000000000000000000, 0.8660254037844387076, 1.000000000000000000, 0.8660254037844387076, 1.000000000000000000, 0.8660254037844387076, 1.000000000000000000, 0.8660254037844387076, 1.000000000000000000, 0.8660254037844387076, 1.000000000000000000, 0.8660254037844387076, 1.000000000000000000, 0.8660254037844387076, 1.000000000000000000, 0.8660254037844387076, 1.000000000000000000, 0.8660254037844387076, 1.000000000000000000, 0.8660254037844387076, 1.000000000000000000, 0.8660254037844387076, 1.000000000000000000, 0.8660254037844387076, 1.000000000000000000, 0.8660254037844387076, 1.000000000000000000, 0.8660254037844387076, 1.000000000000000000, 0.8660254037844387076, 1.000000000000000000, 0.8660254037844387076, 1.000000000000000000, 0.8660254037844387076, 1.000000000000000000, 0.8660254037844387076, 1.000000000000000000, 0.8660254037844387076, 1.000000000000000000, 0.8660254037844387076, 1.000000000000000000, 0.8660254037844387076, 1.000000000000000000, 0.8660254037844387076, 1.000000000000000000, 0.8660254037844387076, 1.000000000000000000, 0.8660254037844387076, 1.000000000000000000, 0.8660254037844387076, 1.000000000000000000, 0.8660254037844387076, 1.000000000000000000, 0.8660254037844387076, 1.000000000000000000, 0.8660254037844387076, 1.000000000000000000, 0.8660254037844387076, 1.000000000000000000, 0.8660254037844387076, 1.000000000000000000, 0.8660254037844387076, 1.000000000000000000, 0.8660254037844387076, 1.000000000000000000, 0.8660254037844387076, 1.000000000000000000, 0.8660254037844387076, 1.000000000000000000, 0.8660254037844387076, 1.000000000000000000, 0.8660254037844387076, 1.000000000000000000, 0.8660254037844387076, 1.000000000000000000, 0.8660254037844387076, 1.000000000000000000, 0.8660254037844387076, 1.000000000000000000, 0.8660254037844387076, 1.000000000000000000, 0.8660254037844387076, 1.000000000000000000, 0.8660254037844387076, 1.000000000000000000, 0.8660254037844387076, 1.000000000000000000, 0.8660254037844387076, 1.000000000000000000, 0.8660254037844387076, 1.000000000000000000, 0.8660254037844387076, 1.000000000000000000, 0.8660254037844387076, 1.000000000000000000, 0.8660254037844387076, 1.000000000000000000, 0.8660254037844387076, 1.000000000000000000, 0.8660254037844387076, 1.000000000000000000, 0.8660254037844387076, 1.000000000000000000, 0.8660254037844387076, 1.000000000000000000, 0.8660254037844387076, 1.000000000000000000, 0.8660254037844387076, 1.000000000000000000, 0.8660254037844387076, 1.000000000000000000, 0.8660254037844387076, 1.000000000000000000, 0.8660254037844387076, 1.000000000000000000, 0.8660254037844387076, 1.000000000000000000, 0.8660254037844387076, 1.000000000000000000, 0.8660254037844387076, 1.000000000000000000, 0.8660254037844387076, 1.000000000000000000, 0.8660254037844387076, 1.000000000000000000, 0.8660254037844387076, 1.000000000000000000, 0.8660254037844387076, 1.000000000000000000, 0.8660254037844387076, 1.000000000000000000, 0.8660254037844387076, 1.000000000000000000, 0.8660254037844387076, 1.000000000000000000, 0.8660254037844387076, 1.000000000000000000, 0.8660254037844387076, 1.000000000000000000, 0.8660254037844387076, 1.000000000000000000),
 ( 1.000000000000000000, 0.8660254037844387076, 1.000000000000000000, 0.8660254037844387076, 1.000000000000000000, 0.8660254037844387076, 1.000000000000000000, 0.8660254037844387076, 1.000000000000000000, 0.8660254037844387076, 1.000000000000000000, 0.8660254037844387076, 1.000000000000000000, 0.8660254037844387076, 1.000000000000000000, 0.8660254037844387076, 1.000000000000000000, 0.8660254037844387076, 1.000000000000000000, 0.8660254037844387076, 1.000000000000000000, 0.8660254037844387076, 1.000000000000000000, 0.8660254037844387076, 1.000000000000000000, 0.8660254037844387076, 1.000000000000000000, 0.8660254037844387076, 1.000000000000000000, 0.8660254037844387076, 1.000000000000000000, 0.8660254037844387076, 1.000000000000000000, 0.8660254037844387076, 1.000000000000000000, 0.8660254037844387076, 1.000000000000000000, 0.8660254037844387076, 1.000000000000000000, 0.8660254037844387076, 1.000000000000000000, 0.8660254037844387076, 1.000000000000000000, 0.8660254037844387076, 1.000000000000000000, 0.8660254037844387076, 1.000000000000000000, 0.8660254037844387076, 1.000000000000000000, 0.8660254037844387076, 1.000000000000000000, 0.8660254037844387076, 1.000000000000000000, 0.8660254037844387076, 1.000000000000000000, 0.8660254037844387076, 1.000000000000000000, 0.8660254037844387076, 1.000000000000000000, 0.8660254037844387076, 1.000000000000000000, 0.8660254037844387076, 1.000000000000000000, 0.8660254037844387076, 1.000000000000000000, 0.8660254037844387076, 1.000000000000000000, 0.8660254037844387076, 1.000000000000000000, 0.8660254037844387076, 1.000000000000000000, 0.8660254037844387076, 1.000000000000000000, 0.8660254037844387076, 1.000000000000000000, 0.8660254037844387076, 1.000000000000000000, 0.8660254037844387076, 1.000000000000000000, 0.8660254037844387076, 1.000000000000000000, 0.8660254037844387076, 1.000000000000000000, 0.8660254037844387076, 1.000000000000000000, 0.8660254037844387076, 1.000000000000000000, 0.8660254037844387076, 1.000000000000000000, 0.8660254037844387076, 1.000000000000000000, 0.8660254037844387076, 1.000000000000000000, 0.8660254037844387076, 1.000000000000000000, 0.8660254037844387076, 1.000000000000000000, 0.8660254037844387076, 1.000000000000000000, 0.8660254037844387076, 1.000000000000000000, 0.8660254037844387076, 1.000000000000000000, 0.8660254037844387076, 1.000000000000000000, 0.8660254037844387076, 1.000000000000000000, 0.8660254037844387076, 1.000000000000000000, 0.8660254037844387076, 1.000000000000000000, 0.8660254037844387076, 1.000000000000000000, 0.8660254037844387076, 1.000000000000000000, 0.8660254037844387076, 1.000000000000000000, 0.8660254037844387076, 1.000000000000000000, 0.8660254037844387076, 1.000000000000000000, 0.8660254037844387076, 1.000000000000000000, 0.8660254037844387076, 1.000000000000000000, 0.8660254037844387076, 1.000000000000000000, 0.8660254037844387076, 1.000000000000000000, 0.8660254037844387076, 1.000000000000000000, 0.8660254037844387076, 1.000000000000000000, 0.8660254037844387076, 1.000000000000000000, 0.8660254037844387076, 1.000000000000000000, 0.8660254037844387076, 1.000000000000000000, 0.8660254037844387076, 1.000000000000000000, 0.8660254037844387076, 1.000000000000000000, 0.8660254037844387076, 1.000000000000000000, 0.8660254037844387076, 1.000000000000000000, 0.8660254037844387076, 1.000000000000000000, 0.8660254037844387076, 1.000000000000000000, 0.8660254037844387076, 1.000000000000000000, 0.8660254037844387076, 1.000000000000000000, 0.8660254037844387076, 1.000000000000000000, 0.8660254037844387076, 1.000000000000000000, 0.8660254037844387076, 1.000000000000000000, 0.8660254037844387076, 1.000000000000000000, 0.8660254037844387076, 1.000000000000000000, 0.8660254037844387076, 1.000000000000000000, 0.8660254037844387076, 1.000000000000000000, 0.8660254037844387076, 1.000000000000000000, 0.8660254037844387076, 1.000000000000000000, 0.8660254037844387076, 1.000000000000000000, 0.8660254037844387076, 1.000000000000000000, 0.8660254037844387076, 1.000000000000000000, 0.8660254037844387076, 1.000000000000000000, 0.8660254037844387076, 1.000000000000000000, 0.8660254037844387076, 1.000000000000000000, 0.8660254037844387076, 1.000000000000000000, 0.8660254037844387076, 1.000000000000000000, 0.8660254037844387076, 1.000000000000000000, 0.8660254037844387076, 1.000000000000000000, 0.8660254037844387076, 1.000000000000000000, 0.8660254037844387076, 1.000000000000000000, 0.8660254037844387076, 1.000000000000000000, 0.8660254037844387076, 1.000000000000000000, 0.8660254037844387076, 1.000000000000000000, 0.8660254037844387076, 1.000000000000000000, 0.8660254037844387076, 1.000000000000000000, 0.8660254037844387076, 1.000000000000000000, 0.8660254037844387076, 1.000000000000000000, 0.8660254037844387076, 1.000000000000000000, 0.8660254037844387076, 1.000000000000000000, 0.8660254037844387076, 1.000000000000000000, 0.8660254037844387076, 1.000000000000000000, 0.8660254037844387076, 1.000000000000000000, 0.8660254037844387076, 1.000000000000000000, 0.8660254037844387076, 1.000000000000000000, 0.8660254037844387076, 1.000000000000000000, 0.8660254037844387076, 1.000000000000000000, 0.8660254037844387076, 1.000000000000000000, 0.8660254037844387076, 1.000000000000000000, 0.8660254037844387076, 1.000000000000000000, 0.8660254037844387076, 1.000000000000000000, 0.8660254037844387076, 1.000000000000000000, 0.8660254037844387076, 1.000000000000000000, 0.8660254037844387076, 1.000000000000000000, 0.8660254037844387076, 1.000000000000000000, 0.8660254037844387076, 1.000000000000000000, 0.8660254037844387076, 1.000000000000000000, 0.8660254037844387076, 1.000000000000000000, 0.8660254037844387076, 1.000000000000000000, 0.8660254037844387076, 1.000000000000000000, 0.8660254037844387076, 1.000000000000000000, 0.8660254037844387076, 1.000000000000000000, 0.8660254037844387076, 1.000000000000000000, 0.8660254037844387076, 1.000000000000000000, 0.8660254037844387076, 1.000000000000000000, 0.8660254037844387076, 1.000000000000000000, 0.8660254037844387076, 1.000000000000000000, 0.8660254037844387076, 1.000000000000000000, 0.8660254037844387076, 1.000000000000000000, 0.8660254037844387076, 1.000000000000000000, 0.8660254037844387076, 1.000000000000000000, 0.8660254037844387076, 1.000000000000000000, 0.8660254037844387076, 1.000000000000000000, 0.8660254037844387076, 1.000000000000000000, 0.8660254037844387076, 1.000000000000000000, 0.8660254037844387076, 1.000000000000000000, 0.8660254037844387076, 1.000000000000000000, 0.8660254037844387076, 1.000000000000000000, 0.8660254037844387076, 1.000000000000000000, 0.8660254037844387076, 1.000000000000000000, 0.8660254037844387076, 1.000000000000000000, 0.8660254037844387076, 1.000000000000000000, 0.8660254037844387076, 1.000000000000000000, 0.8660254037844387076, 1.000000000000000000, 0.8660254037844387076, 1.000000000000000000, 0.8660254037844387076, 1.000000000000000000, 0.8660254037844387076, 1.000000000000000000, 0.8660254037844387076, 1.000000000000000000, 0.8660254037844387076, 1.000000000000000000, 0.8660254037844387076, 1.000000000000000000, 0.8660254037844387076, 1.000000000000000000, 0.8660254037844387076, 1.000000000000000000, 0.8660254037844387076, 1.000000000000000000, 0.8660254037844387076, 1.000000000000000000, 0.8660254037844387076, 1.000000000000000000, 0.8660254037844387076, 1.000000000000000000, 0.8660254037844387076, 1.000000000000000000, 0.8660254037844387076, 1.000000000000000000, 0.8660254037844387076, 1.000000000000000000, 0.8660254037844387076, 1.000000000000000000, 0.8660254037844387076, 1.000000000000000000, 0.8660254037844387076, 1.000000000000000000, 0.8660254037844387076, 1.000000000000000000, 0.8660254037844387076, 1.000000000000000000, 0.8660254037844387076, 1.000000000000000000, 0.8660254037844387076, 1.000000000000000000, 0.8660254037844387076, 1.000000000000000000, 0.8660254037844387076, 1.000000000000000000, 0.8660254037844387076, 1.000000000000000000, 0.8660254037844387076, 1.000000000000000000, 0.8660254037844387076, 1.000000000000000000, 0.8660254037844387076, 1.000000000000000000, 0.8660254037844387076, 1.000000000000000000, 0.8660254037844387076, 1.000000000000000000, 0.8660254037844387076, 1.000000000000000000, 0.8660254037844387076, 1.000000000000000000, 0.8660254037844387076, 1.000000000000000000, 0.8660254037844387076, 1.000000000000000000, 0.8660254037844387076, 1.000000000000000000, 0.8660254037844387076, 1.000000000000000000, 0.8660254037844387076, 1.000000000000000000, 0.8660254037844387076, 1.000000000000000000, 0.8660254037844387076, 1.000000000000000000, 0.8660254037844387076, 1.000000000000000000, 0.8660254037844387076, 1.000000000000000000, 0.8660254037844387076, 1.000000000000000000, 0.8660254037844387076, 1.000000000000000000, 0.8660254037844387076, 1.000000000000000000, 0.8660254037844387076, 1.000000000000000000, 0.8660254037844387076, 1.000000000000000000, 0.8660254037844387076, 1.000000000000000000, 0.8660254037844387076, 1.000000000000000000, 0.8660254037844387076, 1.000000000000000000, 0.8660254037844387076, 1.000000000000000000, 0.8660254037844387076, 1.000000000000000000, 0.8660254037844387076, 1.000000000000000000, 0.8660254037844387076, 1.000000000000000000, 0.8660254037844387076, 1.000000000000000000, 0.8660254037844387076, 1.000000000000000000, 0.8660254037844387076, 1.000000000000000000, 0.8660254037844387076, 1.000000000000000000, 0.8660254037844387076, 1.000000000000000000, 0.8660254037844387076, 1.000000000000000000, 0.8660254037844387076, 1.000000000000000000, 0.8660254037844387076, 1.000000000000000000, 0.8660254037844387076, 1.000000000000000000, 0.8660254037844387076, 1.000000000000000000, 0.8660254037844387076, 1.000000000000000000, 0.8660254037844387076, 1.000000000000000000, 0.8660254037844387076, 1.000000000000000000, 0.8660254037844387076, 1.000000000000000000, 0.8660254037844387076, 1.000000000000000000, 0.8660254037844387076, 1.000000000000000000, 0.8660254037844387076, 1.000000000000000000, 0.8660254037844387076, 1.000000000000000000, 0.8660254037844387076, 1.000000000000000000, 0.8660254037844387076, 1.000000000000000000, 0.8660254037844387076, 1.000000000000000000, 0.8660254037844387076, 1.000000000000000000, 0.8660254037844387076, 1.000000000000000000, 0.8660254037844387076, 1.000000000000000000, 0.8660254037844387076, 1.000000000000000000, 0.8660254037844387076, 1.000000000000000000, 0.8660254037844387076, 1.000000000000000000, 0.8660254037844387076, 1.000000000000000000, 0.8660254037844387076, 1.000000000000000000, 0.8660254037844387076, 1.000000000000000000, 0.8660254037844387076, 1.000000000000000000, 0.8660254037844387076, 1.000000000000000000, 0.8660254037844387076, 1.000000000000000000, 0.8660254037844387076, 1.000000000000000000, 0.8660254037844387076, 1.000000000000000000, 0.8660254037844387076, 1.000000000000000000, 0.8660254037844387076, 1.000000000000000000, 0.8660254037844387076, 1.000000000000000000, 0.8660254037844387076, 1.000000000000000000, 0.8660254037844387076, 1.000000000000000000, 0.8660254037844387076, 1.000000000000000000, 0.8660254037844387076, 1.000000000000000000, 0.8660254037844387076, 1.000000000000000000, 0.8660254037844387076, 1.000000000000000000, 0.8660254037844387076, 1.000000000000000000, 0.8660254037844387076, 1.000000000000000000, 0.8660254037844387076, 1.000000000000000000, 0.8660254037844387076, 1.000000000000000000, 0.8660254037844387076, 1.000000000000000000, 0.8660254037844387076, 1.000000000000000000, 0.8660254037844387076, 1.000000000000000000, 0.8660254037844387076, 1.000000000000000000, 0.8660254037844387076, 1.000000000000000000, 0.8660254037844387076, 1.000000000000000000, 0.8660254037844387076, 1.000000000000000000, 0.8660254037844387076, 1.000000000000000000, 0.8660254037844387076, 1.000000000000000000, 0.8660254037844387076, 1.000000000000000000, 0.8660254037844387076, 1.000000000000000000, 0.8660254037844387076, 1.000000000000000000, 0.8660254037844387076, 1.000000000000000000, 0.8660254037844387076, 1.000000000000000000, 0.8660254037844387076, 1.000000000000000000, 0.8660254037844387076, 1.000000000000000000, 0.8660254037844387076, 1.000000000000000000, 0.8660254037844387076, 1.000000000000000000, 0.8660254037844387076, 1.000000000000000000, 0.8660254037844387076, 1.000000000000000000, 0.8660254037844387076, 1.000000000000000000, 0.8660254037844387076, 1.000000000000000000, 0.8660254037844387076, 1.000000000000000000, 0.8660254037844387076, 1.000000000000000000, 0.8660254037844387076, 1.000000000000000000, 0.8660254037844387076, 1.000000000000000000, 0.8660254037844387076, 1.000000000000000000, 0.8660254037844387076, 1.000000000000000000, 0.8660254037844387076, 1.000000000000000000, 0.8660254037844387076, 1.000000000000000000, 0.8660254037844387076, 1.000000000000000000, 0.8660254037844387076, 1.000000000000000000, 0.8660254037844387076, 1.000000000000000000, 0.8660254037844387076, 1.000000000000000000, 0.8660254037844387076, 1.000000000000000000, 0.8660254037844387076, 1.000000000000000000, 0.8660254037844387076, 1.000000000000000000, 0.8660254037844387076, 1.000000000000000000, 0.8660254037844387076, 1.000000000000000000, 0.8660254037844387076, 1.000000000000000000, 0.8660254037844387076, 1.000000000000000000, 0.8660254037844387076, 1.000000000000000000, 0.8660254037844387076, 1.000000000000000000, 0.8660254037844387076, 1.000000000000000000, 0.8660254037844387076, 1.000000000000000000, 0.8660254037844387076, 1.000000000000000000, 0.8660254037844387076, 1.000000000000000000, 0.8660254037844387076, 1.000000000000000000, 0.8660254037844387076, 1.000000000000000000, 0.8660254037844387076, 1.000000000000000000, 0.8660254037844387076, 1.000000000000000000, 0.8660254037844387076, 1.000000000000000000, 0.8660254037844387076, 1.000000000000000000, 0.8660254037844387076, 1.000000000000000000, 0.8660254037844387076, 1.000000000000000000, 0.8660254037844387076, 1.000000000000000000, 0.8660254037844387076, 1.000000000000000000, 0.8660254037844387076, 1.000000000000000000, 0.8660254037844387076, 1.000000000000000000, 0.8660254037844387076, 1.000000000000000000, 0.8660254037844387076, 1.000000000000000000, 0.8660254037844387076, 1.000000000000000000, 0.8660254037844387076, 1.000000000000000000, 0.8660254037844387076, 1.000000000000000000, 0.8660254037844387076, 1.000000000000000000, 0.8660254037844387076, 1.000000000000000000, 0.8660254037844387076, 1.000000000000000000, 0.8660254037844387076, 1.000000000000000000, 0.8660254037844387076, 1.000000000000000000, 0.8660254037844387076, 1.000000000000000000, 0.8660254037844387076, 1.000000000000000000, 0.8660254037844387076, 1.000000000000000000, 0.8660254037844387076, 1.000000000000000000, 0.8660254037844387076, 1.000000000000000000, 0.8660254037844387076, 1.000000000000000000, 0.8660254037844387076, 1.000000000000000000, 0.8660254037844387076, 1.000000000000000000, 0.8660254037844387076, 1.000000000000000000, 0.8660254037844387076, 1.000000000000000000, 0.8660254037844387076, 1.000000000000000000, 0.8660254037844387076, 1.000000000000000000, 0.8660254037844387076, 1.000000000000000000, 0.8660254037844387076, 1.000000000000000000, 0.8660254037844387076, 1.000000000000000000, 0.8660254037844387076, 1.000000000000000000, 0.8660254037844387076, 1.000000000000000000, 0.8660254037844387076, 1.000000000000000000, 0.8660254037844387076, 1.000000000000000000, 0.8660254037844387076, 1.000000000000000000, 0.8660254037844387076, 1.000000000000000000, 0.8660254037844387076, 1.000000000000000000, 0.8660254037844387076, 1.000000000000000000, 0.8660254037844387076, 1.000000000000000000, 0.8660254037844387076, 1.000000000000000000, 0.8660254037844387076, 1.000000000000000000, 0.8660254037844387076, 1.000000000000000000, 0.8660254037844387076, 1.000000000000000000, 0.8660254037844387076, 1.000000000000000000, 0.8660254037844387076, 1.000000000000000000, 0.8660254037844387076, 1.000000000000000000, 0.8660254037844387076, 1.000000000000000000, 0.8660254037844387076, 1.000000000000000000, 0.8660254037844387076, 1.000000000000000000, 0.8660254037844387076, 1.000000000000000000, 0.8660254037844387076, 1.000000000000000000, 0.8660254037844387076, 1.000000000000000000, 0.8660254037844387076, 1.000000000000000000, 0.8660254037844387076, 1.000000000000000000) ) ) 
 REPRESENTATION_ITEM ( '' )  SURFACE ( )  );
#18791 = DIRECTION ( 'NONE',  ( 0.000000000000000000, 0.000000000000000000, -1.000000000000000000 ) ) ;
#18792 = DIRECTION ( 'NONE',  ( -0.000000000000000000, -1.000000000000000000, -0.000000000000000000 ) ) ;
#18793 = CARTESIAN_POINT ( 'NONE',  ( 14.28750000000000142, -2.886751345948129988, 4.999999999999997335 ) ) ;
#18794 = CARTESIAN_POINT ( 'NONE',  ( 9.001249775931846008E-16, 11.36562500061451786, 34.90005215228797653 ) ) ;
#18795 = CARTESIAN_POINT ( 'NONE',  ( 14.32500000122903394, 2.886751345948126879, 4.999999999999999112 ) ) ;
#18796 = CARTESIAN_POINT ( 'NONE',  ( 23.89687500061451786, 6.054752690667223547, 3.707466751127219781E-16 ) ) ;
#18797 = ORIENTED_EDGE ( 'NONE', *, *, #15596, .F. ) ;
#18798 = CARTESIAN_POINT ( 'NONE',  ( 18.74062500061451431, -3.027376345333610441, -5.243569643749999898 ) ) ;
#18799 = CARTESIAN_POINT ( 'NONE',  ( 4.228125000614517681, -4.541064518000419881, 2.621784821874995952 ) ) ;
#18800 = CARTESIAN_POINT ( 'NONE',  ( 19.43437500061451928, 4.541064518000418104, 2.621784821874999949 ) ) ;
#18801 = CARTESIAN_POINT ( 'NONE',  ( 5.250000000000000888, 0.000000000000000000, 4.999999999999998224 ) ) ;
#18802 = CARTESIAN_POINT ( 'NONE',  ( 7.078125000614516438, 6.421520780324663323E-16, -5.243569643749999010 ) ) ;
#18803 = CARTESIAN_POINT ( 'NONE',  ( 22.15312500061451573, 0.000000000000000000, 5.243569643749999010 ) ) ;
#18804 = CARTESIAN_POINT ( 'NONE',  ( -4.243569643749997233, 16.24062500061451431, 32.45002607614398471 ) ) ;
#18805 = CARTESIAN_POINT ( 'NONE',  ( 19.83750000122903145, -4.330127018922194537, 2.499999999999995559 ) ) ;
#18806 = CARTESIAN_POINT ( 'NONE',  ( 11.14687500061451608, -2.746126346562641984, -4.756430356249999214 ) ) ;
#18807 = CARTESIAN_POINT ( 'NONE',  ( 9.328125000614518214, 6.421520780324663323E-16, -5.243569643749999010 ) ) ;
#18808 = CARTESIAN_POINT ( 'NONE',  ( 2.971875000614517592, -6.054752690667223547, -1.112240025338166033E-15 ) ) ;
#18809 = CARTESIAN_POINT ( 'NONE',  ( 28.37812500061451715, 4.541064518000418104, 2.621784821874999949 ) ) ;
#18810 = CARTESIAN_POINT ( 'NONE',  ( 24.34687500061451715, 6.054752690667223547, 3.707466751127219781E-16 ) ) ;
#18811 = CARTESIAN_POINT ( 'NONE',  ( 13.90312500061451750, 4.541064518000418104, -2.621784821874998173 ) ) ;
#18812 = ADVANCED_FACE ( 'NONE', ( #53121 ), #2519, .T. ) ;
#18813 = CARTESIAN_POINT ( 'NONE',  ( 24.52500000122903145, 2.886751345948129099, -4.999999999999998224 ) ) ;
#18814 = CARTESIAN_POINT ( 'NONE',  ( 26.35312500061451857, -4.541064518000417216, -2.621784821875001281 ) ) ;
#18815 = CARTESIAN_POINT ( 'NONE',  ( 18.34687500061451715, -3.027376345333610441, -5.243569643749999898 ) ) ;
#18816 = CARTESIAN_POINT ( 'NONE',  ( 14.61562500061451608, -6.054752690667223547, -1.112240025338166033E-15 ) ) ;
#18817 = CARTESIAN_POINT ( 'NONE',  ( -4.243569643749997233, 17.64687500061452141, 32.45002607614398471 ) ) ;
#18818 = CARTESIAN_POINT ( 'NONE',  ( 21.47812500061451502, 6.421520780324663323E-16, -5.243569643749999010 ) ) ;
#18819 = DIRECTION ( 'NONE',  ( -1.000000000000000000, -0.000000000000000000, -0.000000000000000000 ) ) ;
#18820 = VERTEX_POINT ( 'NONE', #30594 ) ;
#18821 = CARTESIAN_POINT ( 'NONE',  ( 25.87500000000000000, 4.330127018922191873, 2.499999999999999556 ) ) ;
#18822 = CARTESIAN_POINT ( 'NONE',  ( 1.999999999999998668, 11.75000000000000178, -33.46410161513775705 ) ) ;
#18823 = CARTESIAN_POINT ( 'NONE',  ( 3.756430356250000102, 20.40312499938548285, 30.00000000000000000 ) ) ;
#18824 = CARTESIAN_POINT ( 'NONE',  ( 29.12812500061451715, 6.421520780324663323E-16, -5.243569643749999010 ) ) ;
#18825 = CARTESIAN_POINT ( 'NONE',  ( 6.815625000614517148, 3.027376345333611329, 5.243569643749999010 ) ) ;
#18826 = CARTESIAN_POINT ( 'NONE',  ( 23.17500000122903359, 2.886751345948129099, -4.999999999999998224 ) ) ;
#18827 = CARTESIAN_POINT ( 'NONE',  ( 27.66562500061451146, -6.054752690667223547, -1.112240025338166033E-15 ) ) ;
#18828 = CARTESIAN_POINT ( 'NONE',  ( 24.37500000000000000, 6.123233995736764310E-16, -4.999999999999998224 ) ) ;
#18829 = CARTESIAN_POINT ( 'NONE',  ( -2.000000000000000000, 15.98750000122903181, -33.46410161513775705 ) ) ;
#18830 = CARTESIAN_POINT ( 'NONE',  ( 29.57812500061451644, 6.421520780324663323E-16, -5.243569643749999010 ) ) ;
#18831 = CARTESIAN_POINT ( 'NONE',  ( 11.05312500061451608, -4.541064518000417216, -2.621784821875001281 ) ) ;
#18832 = ORIENTED_EDGE ( 'NONE', *, *, #69351, .F. ) ;
#18833 = CARTESIAN_POINT ( 'NONE',  ( 24.92812500061451431, -4.541064518000419881, 2.621784821874995952 ) ) ;
#18834 = CARTESIAN_POINT ( 'NONE',  ( 6.740625000614516082, 6.054752690667223547, 3.707466751127219781E-16 ) ) ;
#18835 = UNCERTAINTY_MEASURE_WITH_UNIT (LENGTH_MEASURE( 1.000000000000000082E-05 ), #51409, 'distance_accuracy_value', 'NONE');
#18836 = CARTESIAN_POINT ( 'NONE',  ( 4.715625000614516615, -6.054752690667223547, -1.112240025338166033E-15 ) ) ;
#18837 = CARTESIAN_POINT ( 'NONE',  ( 15.57187500061451679, -5.492252693125287522, -1.008910452111647106E-15 ) ) ;
#18838 = CARTESIAN_POINT ( 'NONE',  ( 12.90000000000000213, 0.000000000000000000, 4.999999999999998224 ) ) ;
#18839 =( BOUNDED_CURVE ( )  B_SPLINE_CURVE ( 2, ( #12234, #51769, #11518, #34040, #3714, #41763, #47308 ),
 .UNSPECIFIED., .F., .F. ) 
 B_SPLINE_CURVE_WITH_KNOTS ( ( 3, 2, 2, 3 ),
 ( 0.3166666666666666519, 0.3194444444444444198, 0.3222222222222222432, 0.3250000000000000111 ),
 .UNSPECIFIED. ) 
 CURVE ( )  GEOMETRIC_REPRESENTATION_ITEM ( )  RATIONAL_B_SPLINE_CURVE ( ( 1.000000000000000000, 0.8660254037844387076, 1.000000000000000000, 0.8660254037844387076, 1.000000000000000000, 0.8660254037844387076, 1.000000000000000000 ) ) 
 REPRESENTATION_ITEM ( '' )  );
#18840 = CARTESIAN_POINT ( 'NONE',  ( 13.72500000000000142, 4.330127018922191873, 2.499999999999999556 ) ) ;
#18841 =( BOUNDED_CURVE ( )  B_SPLINE_CURVE ( 2, ( #22527, #51338, #5550, #29168, #16256, #51701, #22168, #33256, #61326 ),
 .UNSPECIFIED., .F., .F. ) 
 B_SPLINE_CURVE_WITH_KNOTS ( ( 3, 2, 2, 2, 3 ),
 ( 0.7282608695652174058, 0.7318840579710145233, 0.7391304347826086474, 0.7463768115942028825, 0.7500000000000000000 ),
 .UNSPECIFIED. ) 
 CURVE ( )  GEOMETRIC_REPRESENTATION_ITEM ( )  RATIONAL_B_SPLINE_CURVE ( ( 0.9330127018922194093, 0.9330127018922194093, 1.000000000000000000, 0.8660254037844387076, 1.000000000000000000, 0.8660254037844387076, 1.000000000000000000, 0.9330127018922194093, 0.9330127018922194093 ) ) 
 REPRESENTATION_ITEM ( '' )  );
#18842 = CARTESIAN_POINT ( 'NONE',  ( 12.68437500061451573, 4.541064518000418104, 2.621784821874999949 ) ) ;
#18843 = CARTESIAN_POINT ( 'NONE',  ( 9.300000001229035362, 5.773502691896255534, 3.535250795749688894E-16 ) ) ;
#18844 = CARTESIAN_POINT ( 'NONE',  ( 17.70937500061451431, 0.000000000000000000, 5.243569643749999010 ) ) ;
#18845 = CARTESIAN_POINT ( 'NONE',  ( 18.41250000000000142, -5.773502691896255534, -1.060575238724906372E-15 ) ) ;
#18846 = CARTESIAN_POINT ( 'NONE',  ( 8.296875000614516438, -3.027376345333614438, 5.243569643749998122 ) ) ;
#18847 = CARTESIAN_POINT ( 'NONE',  ( 4.243569643749999898, 10.99062500061451786, -27.54997392385601529 ) ) ;
#18848 = DIRECTION ( 'NONE',  ( 0.000000000000000000, 0.000000000000000000, 1.000000000000000000 ) ) ;
#18849 = CARTESIAN_POINT ( 'NONE',  ( 22.58437500061451786, -2.746126346562646425, 4.756430356249996549 ) ) ;
#18850 = ORIENTED_EDGE ( 'NONE', *, *, #62575, .F. ) ;
#18851 = CARTESIAN_POINT ( 'NONE',  ( 24.62812500061451715, 6.421520780324663323E-16, -5.243569643749999010 ) ) ;
#18852 = CARTESIAN_POINT ( 'NONE',  ( 29.10937500061451644, -4.541064518000417216, -2.621784821875001281 ) ) ;
#18853 = EDGE_CURVE ( 'NONE', #70559, #33433, #41748, .T. ) ;
#18854 = CARTESIAN_POINT ( 'NONE',  ( 21.44999999999999929, 0.000000000000000000, 4.999999999999998224 ) ) ;
#18855 =( BOUNDED_CURVE ( )  B_SPLINE_CURVE ( 2, ( #66213, #55865, #71768, #49961, #72485, #21871, #27796 ),
 .UNSPECIFIED., .F., .F. ) 
 B_SPLINE_CURVE_WITH_KNOTS ( ( 3, 2, 2, 3 ),
 ( 0.6700000000000000400, 0.6733333333333333393, 0.6766666666666667496, 0.6800000000000001599 ),
 .UNSPECIFIED. ) 
 CURVE ( )  GEOMETRIC_REPRESENTATION_ITEM ( )  RATIONAL_B_SPLINE_CURVE ( ( 1.000000000000000000, 0.8660254037844387076, 1.000000000000000000, 0.8660254037844387076, 1.000000000000000000, 0.8660254037844342667, 1.000000000000004441 ) ) 
 REPRESENTATION_ITEM ( '' )  );
#18856 = CARTESIAN_POINT ( 'NONE',  ( 7.940625000614518036, -3.027376345333610441, -5.243569643749999898 ) ) ;
#18857 = CARTESIAN_POINT ( 'NONE',  ( 25.80937500061451217, -5.492252693125287522, -1.008910452111647106E-15 ) ) ;
#18858 = CARTESIAN_POINT ( 'NONE',  ( 15.72187500061451892, 3.027376345333613106, -5.243569643749998122 ) ) ;
#18859 = CARTESIAN_POINT ( 'NONE',  ( 8.709375000614517859, -5.492252693125287522, -1.008910452111647106E-15 ) ) ;
#18860 = CARTESIAN_POINT ( 'NONE',  ( 3.853125000614517681, -4.541064518000417216, -2.621784821875001281 ) ) ;
#18861 = CARTESIAN_POINT ( 'NONE',  ( 7.471875000614519813, -6.054752690667223547, -1.112240025338166033E-15 ) ) ;
#18862 = ORIENTED_EDGE ( 'NONE', *, *, #68921, .F. ) ;
#18863 = CARTESIAN_POINT ( 'NONE',  ( 19.77187500061451786, 3.027376345333613106, -5.243569643749998122 ) ) ;
#18864 = CARTESIAN_POINT ( 'NONE',  ( 21.52499999999999858, -4.330127018922194537, 2.499999999999995559 ) ) ;
#18865 = CARTESIAN_POINT ( 'NONE',  ( 26.77499999999999858, 4.330127018922191873, 2.499999999999999556 ) ) ;
#18866 = CARTESIAN_POINT ( 'NONE',  ( 28.84687500061452070, 6.054752690667223547, 3.707466751127219781E-16 ) ) ;
#18867 = CARTESIAN_POINT ( 'NONE',  ( 19.38750000000000284, -2.886751345948209480, -4.999999999999856115 ) ) ;
#18868 = ORIENTED_EDGE ( 'NONE', *, *, #13955, .T. ) ;
#18869 = CARTESIAN_POINT ( 'NONE',  ( 10.46249999999999858, 2.886751345948129099, -4.999999999999998224 ) ) ;
#18870 = CARTESIAN_POINT ( 'NONE',  ( 11.97187500061451537, 5.824947211148865298E-16, -4.756430356249998326 ) ) ;
#18871 = CARTESIAN_POINT ( 'NONE',  ( 22.45312500061451644, 4.541064518000418104, -2.621784821874998173 ) ) ;
#18872 = CARTESIAN_POINT ( 'NONE',  ( 13.19999999999999929, 4.330127018922192761, -2.499999999999997780 ) ) ;
#18873 = CARTESIAN_POINT ( 'NONE',  ( 7.950000001229033053, 5.773502691896255534, 3.535250795749688894E-16 ) ) ;
#18874 = CARTESIAN_POINT ( 'NONE',  ( 5.690625000614516260, -3.027376345333610441, -5.243569643749999898 ) ) ;
#18875 = CARTESIAN_POINT ( 'NONE',  ( 21.07499999999999929, -4.330127018922194537, 2.499999999999995559 ) ) ;
#18876 = CARTESIAN_POINT ( 'NONE',  ( 22.00312500061451360, 4.541064518000418104, -2.621784821874998173 ) ) ;
#18877 = CARTESIAN_POINT ( 'NONE',  ( 24.52500000122903145, 2.886751345948129099, -4.999999999999998224 ) ) ;
#18878 = CARTESIAN_POINT ( 'NONE',  ( 1.878215178125000495, 16.76562499938548356, 26.74683588394047007 ) ) ;
#18879 = CARTESIAN_POINT ( 'NONE',  ( 6.150000000000003020, 0.000000000000000000, 4.999999999999998224 ) ) ;
#18880 = ORIENTED_EDGE ( 'NONE', *, *, #23767, .F. ) ;
#18881 = CARTESIAN_POINT ( 'NONE',  ( 20.42812500061451431, -4.541064518000419881, 2.621784821874995952 ) ) ;
#18882 = CARTESIAN_POINT ( 'NONE',  ( 27.44062500061451715, 6.054752690667223547, 3.707466751127219781E-16 ) ) ;
#18883 = CARTESIAN_POINT ( 'NONE',  ( 27.08437500061451786, 4.541064518000418104, 2.621784821874999949 ) ) ;
#18884 = CARTESIAN_POINT ( 'NONE',  ( 13.82812500061451466, 6.421520780324663323E-16, -5.243569643749999010 ) ) ;
#18885 = CARTESIAN_POINT ( 'NONE',  ( 29.88749999999999929, 5.773502691896255534, 3.535250795749688401E-16 ) ) ;
#18886 = EDGE_CURVE ( 'NONE', #68472, #48472, #36214, .T. ) ;
#18887 = CARTESIAN_POINT ( 'NONE',  ( 26.13750000122903216, -4.330127018922194537, 2.499999999999995559 ) ) ;
#18888 = CARTESIAN_POINT ( 'NONE',  ( 18.98437500061451644, 4.119189519843966529, 2.378215178124999607 ) ) ;
#18889 = CARTESIAN_POINT ( 'NONE',  ( 16.75312500061451715, 0.000000000000000000, 5.243569643749999010 ) ) ;
#18890 = CARTESIAN_POINT ( 'NONE',  ( 0.000000000000000000, 20.00000000000000000, 30.00000000000000000 ) ) ;
#18891 = CARTESIAN_POINT ( 'NONE',  ( 28.05937500061451573, 0.000000000000000000, 5.243569643749999010 ) ) ;
#18892 = CARTESIAN_POINT ( 'NONE',  ( 11.55937500061451928, -4.541064518000417216, -2.621784821875001281 ) ) ;
#18893 = CARTESIAN_POINT ( 'NONE',  ( 8.521875000614516082, 3.027376345333613106, -5.243569643749998122 ) ) ;
#18894 = CARTESIAN_POINT ( 'NONE',  ( 18.57187500061451857, 3.027376345333611329, 5.243569643749999010 ) ) ;
#18895 = VERTEX_POINT ( 'NONE', #13959 ) ;
#18896 = CARTESIAN_POINT ( 'NONE',  ( -5.678847837524353181, 8.233079231341500659, 28.02470760206609057 ) ) ;
#18897 = CARTESIAN_POINT ( 'NONE',  ( 24.59062500061451573, -3.027376345333610441, -5.243569643749999898 ) ) ;
#18898 = CARTESIAN_POINT ( 'NONE',  ( 19.05937500061451928, 0.000000000000000000, 5.243569643749999010 ) ) ;
#18899 = CARTESIAN_POINT ( 'NONE',  ( 22.15312500061451573, 0.000000000000000000, 5.243569643749999010 ) ) ;
#18900 = CARTESIAN_POINT ( 'NONE',  ( -0.6945863667395647534, 9.663023495605401081, 26.06076786935074097 ) ) ;
#18901 = CARTESIAN_POINT ( 'NONE',  ( 3.999999999999998668, 13.51250000000000107, 27.69059892324149175 ) ) ;
#18902 = CARTESIAN_POINT ( 'NONE',  ( 28.82812500061451644, 4.541064518000418104, 2.621784821874999949 ) ) ;
#18903 = CARTESIAN_POINT ( 'NONE',  ( 10.05000000122903181, -2.886751345948125991, -5.000000000000000000 ) ) ;
#18904 = ORIENTED_EDGE ( 'NONE', *, *, #16392, .F. ) ;
#18905 = CARTESIAN_POINT ( 'NONE',  ( 5.250000001229035540, 5.773502691896255534, 3.535250795749688894E-16 ) ) ;
#18906 = CARTESIAN_POINT ( 'NONE',  ( 3.999999999999998668, 19.36250000000000426, -32.30940107675850470 ) ) ;
#18907 = CARTESIAN_POINT ( 'NONE',  ( 24.56250000122903288, 4.330127018922192761, -2.499999999999997780 ) ) ;
#18908 = CARTESIAN_POINT ( 'NONE',  ( -8.484601909799255319E-16, 20.43124999877096570, 34.61880215351700940 ) ) ;
#18909 = CARTESIAN_POINT ( 'NONE',  ( 9.346875000614517148, -3.027376345333610441, -5.243569643749999898 ) ) ;
#18910 = LINE ( 'NONE', #57720, #33762 ) ;
#18911 = ADVANCED_FACE ( 'NONE', ( #42047 ), #23949, .T. ) ;
#18912 = CARTESIAN_POINT ( 'NONE',  ( 15.92812500061451608, -4.541064518000419881, 2.621784821874995952 ) ) ;
#18913 = CARTESIAN_POINT ( 'NONE',  ( 11.37187500061451750, 3.027376345333611329, 5.243569643749999010 ) ) ;
#18914 = CARTESIAN_POINT ( 'NONE',  ( 28.76250000122903216, 0.000000000000000000, 4.999999999999998224 ) ) ;
#18915 = ADVANCED_FACE ( 'NONE', ( #53490 ), #23591, .F. ) ;
#18916 = CARTESIAN_POINT ( 'NONE',  ( 20.18437500061451573, 6.421520780324663323E-16, -5.243569643749999010 ) ) ;
#18917 = CARTESIAN_POINT ( 'NONE',  ( 8.296875000614516438, -3.027376345333614438, 5.243569643749998122 ) ) ;
#18918 = LINE ( 'NONE', #20014, #21471 ) ;
#18919 = CARTESIAN_POINT ( 'NONE',  ( 7.903125000614515727, -4.541064518000417216, -2.621784821875001281 ) ) ;
#18920 = CARTESIAN_POINT ( 'NONE',  ( 18.59062500061451573, -3.027376345333614438, 5.243569643749998122 ) ) ;
#18921 = ORIENTED_EDGE ( 'NONE', *, *, #3889, .F. ) ;
#18922 = CARTESIAN_POINT ( 'NONE',  ( 16.00312500061451715, -4.541064518000417216, -2.621784821875001281 ) ) ;
#18923 = CARTESIAN_POINT ( 'NONE',  ( 10.22812500061451679, 6.421520780324663323E-16, -5.243569643749999010 ) ) ;
#18924 = CARTESIAN_POINT ( 'NONE',  ( 23.52187500061451786, 2.746126346562643317, 4.756430356249998326 ) ) ;
#18925 = CARTESIAN_POINT ( 'NONE',  ( 11.84999999999999964, 4.330127018922192761, -2.499999999999997780 ) ) ;
#18926 = CARTESIAN_POINT ( 'NONE',  ( 6.487500001229034474, 6.123233995736764310E-16, -4.999999999999998224 ) ) ;
#18927 = ADVANCED_FACE ( 'NONE', ( #64570 ), #68676, .F. ) ;
#18928 = CARTESIAN_POINT ( 'NONE',  ( 15.94687500061451502, -3.027376345333614438, 5.243569643749998122 ) ) ;
#18929 = CARTESIAN_POINT ( 'NONE',  ( 15.75000000122902932, -2.886751345948129988, 4.999999999999997335 ) ) ;
#18930 = CARTESIAN_POINT ( 'NONE',  ( 23.77499999999999858, -4.330127018922194537, 2.499999999999995559 ) ) ;
#18931 = CARTESIAN_POINT ( 'NONE',  ( 4.243569643749999898, 18.64062500061451644, -27.54997392385601529 ) ) ;
#18932 = CARTESIAN_POINT ( 'NONE',  ( 1.626862140677534470E-15, 13.28750000000000142, 34.00000000000000000 ) ) ;
#18933 = CARTESIAN_POINT ( 'NONE',  ( 22.95000000122903216, -2.886751345948130876, 4.999999999999996447 ) ) ;
#18934 = EDGE_CURVE ( 'NONE', #36091, #3869, #48871, .T. ) ;
#18935 = CYLINDRICAL_SURFACE ( 'NONE', #29255, 4.999999999999998224 ) ;
#18936 = CARTESIAN_POINT ( 'NONE',  ( 1.626862140677534273E-15, 13.36250000000000071, 34.00000000000000000 ) ) ;
#18937 = CARTESIAN_POINT ( 'NONE',  ( 18.00937500061451502, 4.541064518000418104, -2.621784821874998173 ) ) ;
#18938 = CARTESIAN_POINT ( 'NONE',  ( 27.93750000000000000, -2.886751345948125991, -5.000000000000000000 ) ) ;
#18939 = CARTESIAN_POINT ( 'NONE',  ( 15.06562500061451537, -6.054752690667223547, -1.112240025338166033E-15 ) ) ;
#18940 = CARTESIAN_POINT ( 'NONE',  ( 8.231250001229033941, 6.123233995736764310E-16, -4.999999999999998224 ) ) ;
#18941 = DIRECTION ( 'NONE',  ( -0.000000000000000000, -1.000000000000000000, -0.000000000000000000 ) ) ;
#18942 = CARTESIAN_POINT ( 'NONE',  ( 23.55937500061451573, 0.000000000000000000, 5.243569643749999010 ) ) ;
#18943 = CARTESIAN_POINT ( 'NONE',  ( 16.50937500061451502, 2.746126346562645981, -4.756430356249997438 ) ) ;
#18944 = CARTESIAN_POINT ( 'NONE',  ( 9.553125000614517859, 0.000000000000000000, 5.243569643749999010 ) ) ;
#18945 = CARTESIAN_POINT ( 'NONE',  ( 15.42187500061451821, 3.027376345333611329, 5.243569643749999010 ) ) ;
#18946 = ORIENTED_EDGE ( 'NONE', *, *, #36053, .T. ) ;
#18947 = CARTESIAN_POINT ( 'NONE',  ( 27.30937500061451573, -4.541064518000417216, -2.621784821875001281 ) ) ;
#18948 = CARTESIAN_POINT ( 'NONE',  ( 28.60312500061451502, -4.541064518000417216, -2.621784821875001281 ) ) ;
#18949 = CARTESIAN_POINT ( 'NONE',  ( 17.05312500061451786, 4.541064518000418104, -2.621784821874998173 ) ) ;
#18950 = CARTESIAN_POINT ( 'NONE',  ( 29.80312500061451431, 0.000000000000000000, 5.243569643749999010 ) ) ;
#18951 = CARTESIAN_POINT ( 'NONE',  ( 3.999999999999998668, 12.72500000122903430, -32.30940107675850470 ) ) ;
#18952 = CARTESIAN_POINT ( 'NONE',  ( 9.637499999999999289, 5.773502691896255534, 3.535250795749688894E-16 ) ) ;
#18953 = CARTESIAN_POINT ( 'NONE',  ( 20.17500000122903359, 2.886751345948126879, 4.999999999999999112 ) ) ;
#18954 = CARTESIAN_POINT ( 'NONE',  ( 4.000000000000000000, 10.28750000000000142, 32.30940107675849760 ) ) ;
#18955 = CARTESIAN_POINT ( 'NONE',  ( 11.14687500061451608, 4.119189519843966529, -2.378215178124998275 ) ) ;
#18956 = ORIENTED_EDGE ( 'NONE', *, *, #72743, .F. ) ;
#18957 = CARTESIAN_POINT ( 'NONE',  ( 18.00000000000000355, -4.330127018922190985, -2.500000000000001332 ) ) ;
#18958 = CARTESIAN_POINT ( 'NONE',  ( 22.16250000000000142, 2.886751345948129099, -4.999999999999998224 ) ) ;
#18959 = CARTESIAN_POINT ( 'NONE',  ( 18.08437500061451431, 4.541064518000418104, 2.621784821874999949 ) ) ;
#18960 = CARTESIAN_POINT ( 'NONE',  ( 14.31562500061451537, 3.027376345333613106, -5.243569643749998122 ) ) ;
#18961 = VERTEX_POINT ( 'NONE', #57927 ) ;
#18962 = CARTESIAN_POINT ( 'NONE',  ( 10.35000000000000142, -4.330127018922190985, -2.500000000000001332 ) ) ;
#18963 = CARTESIAN_POINT ( 'NONE',  ( 6.590625000614518392, -3.027376345333610441, -5.243569643749999898 ) ) ;
#18964 = CARTESIAN_POINT ( 'NONE',  ( 8.981250001229033941, -4.330127018922194537, 2.499999999999995559 ) ) ;
#18965 = CARTESIAN_POINT ( 'NONE',  ( 12.90000000000000213, 0.000000000000000000, 4.999999999999998224 ) ) ;
#18966 = CARTESIAN_POINT ( 'NONE',  ( 29.29687500061451644, 0.000000000000000000, 4.756430356249998326 ) ) ;
#18967 = CARTESIAN_POINT ( 'NONE',  ( -2.121784821874996840, 14.02812500061451750, 33.67503911421598417 ) ) ;
#18968 = CARTESIAN_POINT ( 'NONE',  ( 3.271875000614519635, 3.027376345333611329, 5.243569643749999010 ) ) ;
#18969 = CARTESIAN_POINT ( 'NONE',  ( 9.074999999999999289, 6.123233995736764310E-16, -4.999999999999998224 ) ) ;
#18970 = CARTESIAN_POINT ( 'NONE',  ( 2.655984681222220721E-16, 17.70312499938548356, 25.66244784525396483 ) ) ;
#18971 = CARTESIAN_POINT ( 'NONE',  ( 24.87187500061451573, 3.027376345333611329, 5.243569643749999010 ) ) ;
#18972 = ORIENTED_EDGE ( 'NONE', *, *, #39310, .T. ) ;
#18973 = CARTESIAN_POINT ( 'NONE',  ( 21.62812500061451360, 4.541064518000418104, 2.621784821874999949 ) ) ;
#18974 = CARTESIAN_POINT ( 'NONE',  ( 23.74687500061451573, -3.027376345333610441, -5.243569643749999898 ) ) ;
#18975 = CARTESIAN_POINT ( 'NONE',  ( -2.121784821874996840, 16.27812500061459389, -26.32496088578401583 ) ) ;
#18976 = CARTESIAN_POINT ( 'NONE',  ( 5.990625000614517859, -3.027376345333614438, 5.243569643749998122 ) ) ;
#18977 = CARTESIAN_POINT ( 'NONE',  ( 28.02187500061451431, 2.746126346562643317, 4.756430356249998326 ) ) ;
#18978 = CARTESIAN_POINT ( 'NONE',  ( 24.92812500061451431, -4.541064518000419881, 2.621784821874995952 ) ) ;
#18979 = CARTESIAN_POINT ( 'NONE',  ( 26.89687500061451431, 4.119189519843966529, -2.378215178124998275 ) ) ;
#18980 = CARTESIAN_POINT ( 'NONE',  ( 11.55937500061451928, -4.119189519843965641, -2.378215178125001383 ) ) ;
#18981 = CARTESIAN_POINT ( 'NONE',  ( 16.73437500061451644, 4.541064518000418104, 2.621784821874999949 ) ) ;
#18982 = CARTESIAN_POINT ( 'NONE',  ( 27.87187500061451573, 3.027376345333613106, -5.243569643749998122 ) ) ;
#18983 = CARTESIAN_POINT ( 'NONE',  ( 4.243569643749999898, 17.34687500061451715, 32.45002607614398471 ) ) ;
#18984 = CARTESIAN_POINT ( 'NONE',  ( 6.365625000614518747, 3.027376345333611329, 5.243569643749999010 ) ) ;
#18985 = CARTESIAN_POINT ( 'NONE',  ( 30.00000000000000000, 0.000000000000000000, 0.000000000000000000 ) ) ;
#18986 = CARTESIAN_POINT ( 'NONE',  ( 4.171875000614517326, 3.027376345333611329, 5.243569643749999010 ) ) ;
#18987 = CARTESIAN_POINT ( 'NONE',  ( -1.626862140677534273E-15, 17.33749999999999858, 34.00000000000000000 ) ) ;
#18988 = CARTESIAN_POINT ( 'NONE',  ( 5.953125000614519102, 0.000000000000000000, 5.243569643749999010 ) ) ;
#18989 = CARTESIAN_POINT ( 'NONE',  ( 9.421875000614519990, 3.027376345333613106, -5.243569643749998122 ) ) ;
#18990 = CARTESIAN_POINT ( 'NONE',  ( 16.91250000122903430, 4.330127018922192761, -2.499999999999997780 ) ) ;
#18991 = CARTESIAN_POINT ( 'NONE',  ( 3.084375000614519191, 6.421520780324663323E-16, -5.243569643749999010 ) ) ;
#18992 = CARTESIAN_POINT ( 'NONE',  ( 7.228125000614517681, 4.541064518000418104, 2.621784821874999949 ) ) ;
#18993 = DIRECTION ( 'NONE',  ( -0.000000000000000000, -1.000000000000000000, -0.000000000000000000 ) ) ;
#18994 = CARTESIAN_POINT ( 'NONE',  ( 22.10625000122903216, -4.330127018922190985, -2.500000000000001332 ) ) ;
#18995 = CARTESIAN_POINT ( 'NONE',  ( 15.60937500061451644, -4.541064518000417216, -2.621784821875001281 ) ) ;
#18996 = CARTESIAN_POINT ( 'NONE',  ( 45.00000000000000000, 6.123233995736764310E-16, -4.999999999999998224 ) ) ;
#18997 = VERTEX_POINT ( 'NONE', #26518 ) ;
#18998 = CARTESIAN_POINT ( 'NONE',  ( 24.89062500061451644, -3.027376345333614438, 5.243569643749998122 ) ) ;
#18999 = CARTESIAN_POINT ( 'NONE',  ( 10.30312500061451431, 4.541064518000418104, -2.621784821874998173 ) ) ;
#19000 = CARTESIAN_POINT ( 'NONE',  ( 27.27187500061451431, -6.054752690667223547, -1.112240025338166033E-15 ) ) ;
#19001 = CARTESIAN_POINT ( 'NONE',  ( 10.30312500061451431, 4.541064518000418104, -2.621784821874998173 ) ) ;
#19002 = FACE_OUTER_BOUND ( 'NONE', #12905, .T. ) ;
#19003 = CARTESIAN_POINT ( 'NONE',  ( 9.937500001229032875, -4.330127018922194537, 2.499999999999995559 ) ) ;
#19004 = CARTESIAN_POINT ( 'NONE',  ( 25.94062500061451715, -3.027376345333610441, -5.243569643749999898 ) ) ;
#19005 = CARTESIAN_POINT ( 'NONE',  ( -4.243569643749999898, 12.56562500061451715, -32.45002607614398471 ) ) ;
#19006 = CARTESIAN_POINT ( 'NONE',  ( 12.82500000122903394, 2.886751345948129099, -4.999999999999998224 ) ) ;
#19007 = CARTESIAN_POINT ( 'NONE',  ( 21.47812500061451502, 6.421520780324663323E-16, -5.243569643749999010 ) ) ;
#19008 = CARTESIAN_POINT ( 'NONE',  ( 18.81562500061452070, 3.027376345333613106, -5.243569643749998122 ) ) ;
#19009 = CARTESIAN_POINT ( 'NONE',  ( 6.084375000614518747, -4.541064518000419881, 2.621784821874995952 ) ) ;
#19010 = CARTESIAN_POINT ( 'NONE',  ( 18.33749999999999858, -2.886751345948129988, 4.999999999999997335 ) ) ;
#19011 = EDGE_CURVE ( 'NONE', #58630, #41088, #26889, .T. ) ;
#19012 = CARTESIAN_POINT ( 'NONE',  ( 14.40000000122903323, -2.886751345948129988, 4.999999999999997335 ) ) ;
#19013 = CARTESIAN_POINT ( 'NONE',  ( 10.04062500061451502, -3.027376345333614438, 5.243569643749998122 ) ) ;
#19014 =( GEOMETRIC_REPRESENTATION_CONTEXT ( 3 ) GLOBAL_UNCERTAINTY_ASSIGNED_CONTEXT ( ( #57285 ) ) GLOBAL_UNIT_ASSIGNED_CONTEXT ( ( #53357, #41912, #64802 ) ) REPRESENTATION_CONTEXT ( 'NONE', 'WORKASPACE' ) );
#19015 = CARTESIAN_POINT ( 'NONE',  ( 14.12812500061451715, -4.541064518000419881, 2.621784821874995952 ) ) ;
#19016 = CARTESIAN_POINT ( 'NONE',  ( 24.78750000122903074, -4.330127018922194537, 2.499999999999995559 ) ) ;
#19017 = CARTESIAN_POINT ( 'NONE',  ( 21.08437500061451786, 6.421520780324663323E-16, -5.243569643749999010 ) ) ;
#19018 = CARTESIAN_POINT ( 'NONE',  ( 20.14687500061451786, -3.027376345333610441, -5.243569643749999898 ) ) ;
#19019 = LINE ( 'NONE', #17938, #50125 ) ;
#19020 = EDGE_CURVE ( 'NONE', #48662, #47727, #43696, .T. ) ;
#19021 = CARTESIAN_POINT ( 'NONE',  ( 7.237500001229035362, -4.330127018922194537, 2.499999999999995559 ) ) ;
#19022 = CARTESIAN_POINT ( 'NONE',  ( 6.909375000614518036, 0.000000000000000000, 5.243569643749999010 ) ) ;
#19023 = CARTESIAN_POINT ( 'NONE',  ( 26.52187500061451431, 3.027376345333613106, -5.243569643749998122 ) ) ;
#19024 = ADVANCED_FACE ( 'NONE', ( #20957 ), #66035, .T. ) ;
#19025 = CARTESIAN_POINT ( 'NONE',  ( 15.30000000122903181, -2.886751345948063374, 5.000000000000112799 ) ) ;
#19026 = CARTESIAN_POINT ( 'NONE',  ( 21.10312500061451502, 4.541064518000418104, -2.621784821874998173 ) ) ;
#19028 = ADVANCED_FACE ( 'NONE', ( #59377 ), #25785, .F. ) ;
#19027 = CARTESIAN_POINT ( 'NONE',  ( 27.04687500061451644, 6.054752690667223547, 3.707466751127219781E-16 ) ) ;
#19029 = CARTESIAN_POINT ( 'NONE',  ( 1.878215178124997609, 16.72812499938548214, 33.25316411605952993 ) ) ;
#19030 = CARTESIAN_POINT ( 'NONE',  ( 3.228505727505837974, -3.817951121670090320, 3.373270459396892296 ) ) ;
#19031 = DIRECTION ( 'NONE',  ( 0.000000000000000000, -1.000000000000000000, 0.000000000000000000 ) ) ;
#19032 = CARTESIAN_POINT ( 'NONE',  ( 7.321875000614516793, 3.027376345333611329, 5.243569643749999010 ) ) ;
#19033 = CARTESIAN_POINT ( 'NONE',  ( 18.40312500061451573, 4.541064518000418104, -2.621784821874998173 ) ) ;
#19034 = VERTEX_POINT ( 'NONE', #64934 ) ;
#19035 = LINE ( 'NONE', #68951, #34827 ) ;
#19036 = CARTESIAN_POINT ( 'NONE',  ( 26.57812500061451644, 4.541064518000418104, 2.621784821874999949 ) ) ;
#19037 = CARTESIAN_POINT ( 'NONE',  ( 5.109375000614518214, 0.000000000000000000, 5.243569643749999010 ) ) ;
#19038 = CARTESIAN_POINT ( 'NONE',  ( -3.999999999999999112, 15.94999999999999929, -30.00000000000000000 ) ) ;
#19039 = DIRECTION ( 'NONE',  ( 1.000000000000000000, -0.000000000000000000, -0.000000000000000000 ) ) ;
#19040 = CARTESIAN_POINT ( 'NONE',  ( 17.28750000000000142, 5.773502691896255534, 3.535250795749688894E-16 ) ) ;
#19041 = CARTESIAN_POINT ( 'NONE',  ( 20.57812500061451644, 6.421520780324663323E-16, -5.243569643749999010 ) ) ;
#19042 = ORIENTED_EDGE ( 'NONE', *, *, #67227, .F. ) ;
#19043 = CARTESIAN_POINT ( 'NONE',  ( 24.89999999999999858, 4.330127018922192761, -2.499999999999997780 ) ) ;
#19044 = CARTESIAN_POINT ( 'NONE',  ( 25.35937500061451644, 0.000000000000000000, 5.243569643749999010 ) ) ;
#19045 = ORIENTED_EDGE ( 'NONE', *, *, #26050, .T. ) ;
#19046 = CARTESIAN_POINT ( 'NONE',  ( 2.964777361493091679, -4.026176250088806086, -3.359304602455296607 ) ) ;
#19047 = CARTESIAN_POINT ( 'NONE',  ( 12.81562500061451537, -6.054752690667223547, -1.112240025338166033E-15 ) ) ;
#19048 = CARTESIAN_POINT ( 'NONE',  ( 6.328125000614515550, 4.541064518000418104, 2.621784821874999949 ) ) ;
#19049 = CARTESIAN_POINT ( 'NONE',  ( 15.98437500061451644, -2.746126346562642428, -4.756430356249999214 ) ) ;
#19050 = CARTESIAN_POINT ( 'NONE',  ( 29.35312500061451502, 0.000000000000000000, 5.243569643749999010 ) ) ;
#19051 = CARTESIAN_POINT ( 'NONE',  ( 16.05000000122903359, 5.773502691896255534, 3.535250795749688894E-16 ) ) ;
#19052 = CARTESIAN_POINT ( 'NONE',  ( 19.65000000000000213, 0.000000000000000000, 4.999999999999998224 ) ) ;
#19053 = CARTESIAN_POINT ( 'NONE',  ( 28.49999999999999645, 4.330127018922192761, -2.499999999999997780 ) ) ;
#19054 = CARTESIAN_POINT ( 'NONE',  ( 2.000000000000001332, 10.70000000000000107, -26.53589838486224650 ) ) ;
#19055 = CARTESIAN_POINT ( 'NONE',  ( 8.671875000614518214, 3.027376345333611329, 5.243569643749999010 ) ) ;
#19056 = CARTESIAN_POINT ( 'NONE',  ( 19.69687500061451857, -3.027376345333610441, -5.243569643749999898 ) ) ;
#19057 = DIRECTION ( 'NONE',  ( -1.000000000000000000, -0.000000000000000000, -0.000000000000000000 ) ) ;
#19058 = EDGE_LOOP ( 'NONE', ( #49261, #47435 ) ) ;
#19059 = CARTESIAN_POINT ( 'NONE',  ( 28.90312500061451217, 0.000000000000000000, 5.243569643749999010 ) ) ;
#19060 = CARTESIAN_POINT ( 'NONE',  ( 29.59687500061451715, -3.027376345333610441, -5.243569643749999898 ) ) ;
#19061 = CARTESIAN_POINT ( 'NONE',  ( 3.721875000614518036, 3.027376345333611329, 5.243569643749999010 ) ) ;
#19062 = CARTESIAN_POINT ( 'NONE',  ( 17.10000000000000142, -4.330127018922190985, -2.500000000000001332 ) ) ;
#19063 = CARTESIAN_POINT ( 'NONE',  ( 13.11562500061451786, 3.027376345333611329, 5.243569643749999010 ) ) ;
#19064 = CARTESIAN_POINT ( 'NONE',  ( 1.999999999999997335, 18.72499999999999787, 33.46410161513775705 ) ) ;
#19066 = FACE_OUTER_BOUND ( 'NONE', #63225, .T. ) ;
#19065 = PRODUCT_DEFINITION_FORMATION_WITH_SPECIFIED_SOURCE ( 'ANY', '', #65012, .NOT_KNOWN. ) ;
#19067 = CARTESIAN_POINT ( 'NONE',  ( 18.90000000122902790, -2.886751345948129988, 4.999999999999997335 ) ) ;
#19068 = DIRECTION ( 'NONE',  ( -0.000000000000000000, -1.000000000000000000, -0.000000000000000000 ) ) ;
#19069 = CARTESIAN_POINT ( 'NONE',  ( 18.23437500061451999, -4.119189519843968306, 2.378215178124996054 ) ) ;
#19070 = CARTESIAN_POINT ( 'NONE',  ( 8.240625000614516082, -3.027376345333614438, 5.243569643749998122 ) ) ;
#19071 = CARTESIAN_POINT ( 'NONE',  ( 24.75937500061451502, 4.541064518000418104, -2.621784821874998173 ) ) ;
#19072 = CARTESIAN_POINT ( 'NONE',  ( -4.243569643749999898, 19.37187500061451928, 27.54997392385601529 ) ) ;
#19073 = CARTESIAN_POINT ( 'NONE',  ( 27.57187500061451857, 3.027376345333611329, 5.243569643749999010 ) ) ;
#19074 = CARTESIAN_POINT ( 'NONE',  ( 7.012500000000001066, 2.886751345948126879, 4.999999999999999112 ) ) ;
#19075 = CARTESIAN_POINT ( 'NONE',  ( -3.999999999999999556, 12.42500000122903359, 27.69059892324149530 ) ) ;
#19076 = CARTESIAN_POINT ( 'NONE',  ( 15.17812500061451608, 6.421520780324663323E-16, -5.243569643749999010 ) ) ;
#19078 =( BOUNDED_CURVE ( )  B_SPLINE_CURVE ( 2, ( #22794, #67881, #33164, #39813, #55702, #5096, #50166, #72695, #22077 ),
 .UNSPECIFIED., .F., .F. ) 
 B_SPLINE_CURVE_WITH_KNOTS ( ( 3, 2, 2, 2, 3 ),
 ( 0.5760869565217391353, 0.5797101449275362528, 0.5869565217391304879, 0.5942028985507246119, 0.5978260869565217295 ),
 .UNSPECIFIED. ) 
 CURVE ( )  GEOMETRIC_REPRESENTATION_ITEM ( )  RATIONAL_B_SPLINE_CURVE ( ( 0.9330127018922194093, 0.9330127018922194093, 1.000000000000000000, 0.8660254037844387076, 1.000000000000000000, 0.8660254037844387076, 1.000000000000000000, 0.9330127018922194093, 0.9330127018922194093 ) ) 
 REPRESENTATION_ITEM ( '' )  );
#19077 = CARTESIAN_POINT ( 'NONE',  ( 5.737500001229033586, 4.330127018922191873, 2.499999999999999556 ) ) ;
#19079 = VECTOR ( 'NONE', #40375, 1000.000000000000000 ) ;
#19080 = CARTESIAN_POINT ( 'NONE',  ( 10.95937500061451964, 0.000000000000000000, 5.243569643749999010 ) ) ;
#19081 = DIRECTION ( 'NONE',  ( 0.000000000000000000, 0.000000000000000000, 1.000000000000000000 ) ) ;
#19082 = ORIENTED_EDGE ( 'NONE', *, *, #41965, .F. ) ;
#19083 = CARTESIAN_POINT ( 'NONE',  ( 11.61562500061451608, 3.027376345333613106, -5.243569643749998122 ) ) ;
#19084 = CARTESIAN_POINT ( 'NONE',  ( 4.000000000000000000, 19.64374999877096428, 30.00000000000000000 ) ) ;
#19085 = CARTESIAN_POINT ( 'NONE',  ( 24.33750000122903145, -4.330127018922194537, 2.499999999999995559 ) ) ;
#19086 = CARTESIAN_POINT ( 'NONE',  ( 11.74687500061451573, 6.054752690667223547, 3.707466751127219781E-16 ) ) ;
#19087 = CARTESIAN_POINT ( 'NONE',  ( 15.21562500061451750, 3.027376345333613106, -5.243569643749998122 ) ) ;
#19088 = CARTESIAN_POINT ( 'NONE',  ( 29.56875000122903074, 2.886751345948126879, 4.999999999999999112 ) ) ;
#19089 = CARTESIAN_POINT ( 'NONE',  ( 23.33437500061451786, 6.421520780324663323E-16, -5.243569643749999010 ) ) ;
#19090 = FACE_OUTER_BOUND ( 'NONE', #20198, .T. ) ;
#19091 = CARTESIAN_POINT ( 'NONE',  ( -3.305248395036964552E-15, 5.000000000000034639, 25.99999999999995737 ) ) ;
#19092 = DIRECTION ( 'NONE',  ( 0.000000000000000000, 0.000000000000000000, -1.000000000000000000 ) ) ;
#19093 = CARTESIAN_POINT ( 'NONE',  ( 4.243569643749999898, 15.54687500061451644, -27.54997392385601529 ) ) ;
#19094 = CARTESIAN_POINT ( 'NONE',  ( 16.02187500061451786, -6.054752690667223547, -1.112240025338166033E-15 ) ) ;
#19095 = CARTESIAN_POINT ( 'NONE',  ( 17.96250000122903501, 0.000000000000000000, 4.999999999999998224 ) ) ;
#19096 = CARTESIAN_POINT ( 'NONE',  ( 11.48437500061451644, -4.541064518000419881, 2.621784821874995952 ) ) ;
#19097 = CARTESIAN_POINT ( 'NONE',  ( 9.001249775931846008E-16, 19.01562500061451644, -25.09994784771203058 ) ) ;
#19098 = CARTESIAN_POINT ( 'NONE',  ( 19.42500000122903714, -5.773502691896255534, -1.060575238724906372E-15 ) ) ;
#19099 = CARTESIAN_POINT ( 'NONE',  ( 13.15312500061451750, 0.000000000000000000, 5.243569643749999010 ) ) ;
#19100 = ORIENTED_EDGE ( 'NONE', *, *, #446, .T. ) ;
#19101 = EDGE_LOOP ( 'NONE', ( #49490, #13262, #30473, #69462 ) ) ;
#19102 = CARTESIAN_POINT ( 'NONE',  ( 17.28750000000000142, 5.773502691896255534, 3.535250795749688894E-16 ) ) ;
#19103 = CARTESIAN_POINT ( 'NONE',  ( 27.29999999999999716, 0.000000000000000000, 4.999999999999998224 ) ) ;
#19104 = CARTESIAN_POINT ( 'NONE',  ( 11.74687500061451573, 6.054752690667223547, 3.707466751127219781E-16 ) ) ;
#19105 = CARTESIAN_POINT ( 'NONE',  ( 22.42500000000000071, -4.330127018922194537, 2.499999999999995559 ) ) ;
#19106 = CARTESIAN_POINT ( 'NONE',  ( 12.97500000122903252, 2.886751345948126879, 4.999999999999999112 ) ) ;
#19107 = CARTESIAN_POINT ( 'NONE',  ( 21.90000000122903145, 5.773502691896255534, 3.535250795749688894E-16 ) ) ;
#19108 = CARTESIAN_POINT ( 'NONE',  ( 18.14062500061451644, -3.027376345333614438, 5.243569643749998122 ) ) ;
#19109 = CARTESIAN_POINT ( 'NONE',  ( 20.05312500061451431, -4.541064518000417216, -2.621784821875001281 ) ) ;
#19110 = CARTESIAN_POINT ( 'NONE',  ( 3.140625000614516882, 6.054752690667223547, 3.707466751127219781E-16 ) ) ;
#19111 = CARTESIAN_POINT ( 'NONE',  ( 27.00000000000000000, -4.330127018922190985, -2.500000000000001332 ) ) ;
#19112 = CARTESIAN_POINT ( 'NONE',  ( 45.00000000000000000, 0.000000000000000000, 0.000000000000000000 ) ) ;
#19113 = CARTESIAN_POINT ( 'NONE',  ( 28.49999999999999645, 4.330127018922192761, -2.499999999999997780 ) ) ;
#19114 = CARTESIAN_POINT ( 'NONE',  ( 28.43437500061451573, 4.541064518000418104, 2.621784821874999949 ) ) ;
#19115 = CARTESIAN_POINT ( 'NONE',  ( 3.999999999999998668, 14.41250000000000142, -32.30940107675850470 ) ) ;
#19116 = CARTESIAN_POINT ( 'NONE',  ( 2.121784821874999061, 16.55937500061451573, -33.67503911421598417 ) ) ;
#19117 = CARTESIAN_POINT ( 'NONE',  ( 4.800000001229032698, 5.773502691896255534, 3.535250795749688894E-16 ) ) ;
#19118 = CARTESIAN_POINT ( 'NONE',  ( 6.637500000000001066, -2.886751345948129988, 4.999999999999997335 ) ) ;
#19119 = EDGE_CURVE ( 'NONE', #33154, #60311, #5940, .T. ) ;
#19120 = CARTESIAN_POINT ( 'NONE',  ( 27.52500000000000213, 6.123233995736764310E-16, -4.999999999999998224 ) ) ;
#19121 = CARTESIAN_POINT ( 'NONE',  ( 9.534375000614517148, 4.541064518000418104, 2.621784821874999949 ) ) ;
#19122 = CARTESIAN_POINT ( 'NONE',  ( 27.85312500061451502, 4.541064518000418104, -2.621784821874998173 ) ) ;
#19123 = CARTESIAN_POINT ( 'NONE',  ( 1.071796769724491893, 10.68259618943233313, 33.99999999999999289 ) ) ;
#19124 = CARTESIAN_POINT ( 'NONE',  ( -4.513148444473915610, 8.924709038934331318, -33.95832947008857872 ) ) ;
#19125 = CARTESIAN_POINT ( 'NONE',  ( 1.071796769724493892, 17.72990381179669583, -34.00000000000000000 ) ) ;
#19126 = CARTESIAN_POINT ( 'NONE',  ( 8.146875000614516082, 6.054752690667223547, 3.707466751127219781E-16 ) ) ;
#19127 = CARTESIAN_POINT ( 'NONE',  ( 10.35937500061451644, 4.541064518000418104, -2.621784821874998173 ) ) ;
#19128 = CARTESIAN_POINT ( 'NONE',  ( 4.087500000000001243, -2.886751345948125991, -5.000000000000000000 ) ) ;
#19129 = CARTESIAN_POINT ( 'NONE',  ( 4.243569643749999898, 14.17812500061459247, 30.00000000000000000 ) ) ;
#19130 = CARTESIAN_POINT ( 'NONE',  ( 1.626862140677534470E-15, 13.28750000000000142, 34.00000000000000000 ) ) ;
#19131 = CARTESIAN_POINT ( 'NONE',  ( 6.975000000000002309, 4.330127018922191873, 2.499999999999999556 ) ) ;
#19132 = CARTESIAN_POINT ( 'NONE',  ( 16.09687500061451715, 4.119189519843966529, -2.378215178124998275 ) ) ;
#19133 = CARTESIAN_POINT ( 'NONE',  ( 20.87812500061451715, -4.541064518000419881, 2.621784821874995952 ) ) ;
#19134 = CARTESIAN_POINT ( 'NONE',  ( 12.85312500061451502, -4.541064518000417216, -2.621784821875001281 ) ) ;
#19135 = CARTESIAN_POINT ( 'NONE',  ( 22.80937500061451573, 2.746126346562645981, -4.756430356249997438 ) ) ;
#19136 = CARTESIAN_POINT ( 'NONE',  ( 9.159375000614515372, 0.000000000000000000, 5.243569643749999010 ) ) ;
#19137 = CARTESIAN_POINT ( 'NONE',  ( 25.68750000000000000, -2.886751345948125991, -5.000000000000000000 ) ) ;
#19138 = CARTESIAN_POINT ( 'NONE',  ( 21.93750000122903288, 4.330127018922191873, 2.499999999999999556 ) ) ;
#19139 = CARTESIAN_POINT ( 'NONE',  ( -1.071796769724487453, 18.22009619066136565, -34.00000000000000000 ) ) ;
#19140 = CARTESIAN_POINT ( 'NONE',  ( 11.07187500061451679, -6.054752690667223547, -1.112240025338166033E-15 ) ) ;
#19141 = CARTESIAN_POINT ( 'NONE',  ( 27.27187500061451431, -6.054752690667223547, -1.112240025338166033E-15 ) ) ;
#19142 = CARTESIAN_POINT ( 'NONE',  ( 3.871875000614519280, -6.054752690667223547, -1.112240025338166033E-15 ) ) ;
#19143 = CARTESIAN_POINT ( 'NONE',  ( 34.99999999999999289, 0.000000000000000000, 0.000000000000000000 ) ) ;
#19144 = CARTESIAN_POINT ( 'NONE',  ( 19.84687500061451360, 6.054752690667223547, 3.707466751127219781E-16 ) ) ;
#19145 = CARTESIAN_POINT ( 'NONE',  ( 11.25937500061451679, 4.541064518000418104, -2.621784821874998173 ) ) ;
#19146 = CARTESIAN_POINT ( 'NONE',  ( 3.756430356250000102, 18.15312499938548285, 30.00000000000000000 ) ) ;
#19147 = CARTESIAN_POINT ( 'NONE',  ( 23.51249999999999574, 2.886751345948129099, -4.999999999999998224 ) ) ;
#19148 = CARTESIAN_POINT ( 'NONE',  ( -1.878215178124999163, 19.99062499938548143, 26.74683588394047007 ) ) ;
#19149 = CARTESIAN_POINT ( 'NONE',  ( 4.243569643749999898, 13.33437500061451786, -30.00000000000000000 ) ) ;
#19150 = CARTESIAN_POINT ( 'NONE',  ( 24.19687500061451857, -2.746126346562642428, -4.756430356249999214 ) ) ;
#19151 = CARTESIAN_POINT ( 'NONE',  ( 14.39062500061451821, 6.054752690667223547, 3.707466751127219781E-16 ) ) ;
#19152 = CARTESIAN_POINT ( 'NONE',  ( 4.650000000000001243, 4.330127018922192761, -2.499999999999997780 ) ) ;
#19153 = CARTESIAN_POINT ( 'NONE',  ( -1.071796769724490339, 18.03259618943233633, 26.00000000000000000 ) ) ;
#19154 = CARTESIAN_POINT ( 'NONE',  ( -1.999999999999997113, 12.87500000000000178, 33.46410161513775705 ) ) ;
#19155 = CARTESIAN_POINT ( 'NONE',  ( 13.91249999999999964, -5.773502691896255534, -1.060575238724906372E-15 ) ) ;
#19156 = CARTESIAN_POINT ( 'NONE',  ( 9.001249775931846008E-16, 10.91562500061451857, 34.90005215228797653 ) ) ;
#19157 = CARTESIAN_POINT ( 'NONE',  ( 14.70000000122903394, 5.773502691896255534, 3.535250795749688894E-16 ) ) ;
#19158 = CARTESIAN_POINT ( 'NONE',  ( 24.00937500061451502, 0.000000000000000000, 5.243569643749999010 ) ) ;
#19159 = CARTESIAN_POINT ( 'NONE',  ( 20.28750000122903074, -4.330127018922194537, 2.499999999999995559 ) ) ;
#19160 = ORIENTED_EDGE ( 'NONE', *, *, #21528, .F. ) ;
#19161 = CARTESIAN_POINT ( 'NONE',  ( 19.82812500061451644, 4.541064518000418104, 2.621784821874999949 ) ) ;
#19162 = CARTESIAN_POINT ( 'NONE',  ( 5.165625000614518569, -6.054752690667223547, -1.112240025338166033E-15 ) ) ;
#19163 = CARTESIAN_POINT ( 'NONE',  ( 19.92187500061451644, 3.027376345333611329, 5.243569643749999010 ) ) ;
#19164 = CARTESIAN_POINT ( 'NONE',  ( 29.59687500061451715, -3.027376345333610441, -5.243569643749999898 ) ) ;
#19165 = CARTESIAN_POINT ( 'NONE',  ( 5.953125000614519102, 0.000000000000000000, 5.243569643749999010 ) ) ;
#19166 = CARTESIAN_POINT ( 'NONE',  ( 22.19062500061451715, -3.027376345333614438, 5.243569643749998122 ) ) ;
#19167 = CARTESIAN_POINT ( 'NONE',  ( -4.243569643749999898, 14.81562500061451715, 27.54997392385601529 ) ) ;
#19168 = CARTESIAN_POINT ( 'NONE',  ( 19.23750000122903714, 4.330127018922191873, 2.499999999999999556 ) ) ;
#19169 = CARTESIAN_POINT ( 'NONE',  ( 12.49687500061451573, -2.746126346562641984, -4.756430356249999214 ) ) ;
#19170 = CARTESIAN_POINT ( 'NONE',  ( 8.765625000614518214, -6.054752690667223547, -1.112240025338166033E-15 ) ) ;
#19171 = CARTESIAN_POINT ( 'NONE',  ( 3.534375000614518036, 6.421520780324663323E-16, -5.243569643749999010 ) ) ;
#19172 = CARTESIAN_POINT ( 'NONE',  ( 21.94687500061451857, -3.027376345333610441, -5.243569643749999898 ) ) ;
#19173 = CARTESIAN_POINT ( 'NONE',  ( 14.91562500061451679, 3.027376345333611329, 5.243569643749999010 ) ) ;
#19174 = CARTESIAN_POINT ( 'NONE',  ( 26.06250000122903288, 0.000000000000000000, 4.999999999999998224 ) ) ;
#19175 = EDGE_CURVE ( 'NONE', #29564, #69714, #33769, .T. ) ;
#19176 = CARTESIAN_POINT ( 'NONE',  ( 25.90312500061451573, -4.541064518000417216, -2.621784821875001281 ) ) ;
#19177 = VECTOR ( 'NONE', #54167, 1000.000000000000000 ) ;
#19178 = CARTESIAN_POINT ( 'NONE',  ( 20.37187500061451573, 3.027376345333611329, 5.243569643749999010 ) ) ;
#19179 = CARTESIAN_POINT ( 'NONE',  ( 15.62812500061451537, 6.421520780324663323E-16, -5.243569643749999010 ) ) ;
#19180 = CARTESIAN_POINT ( 'NONE',  ( -4.243569643749999898, 17.57187500061451502, 27.54997392385601529 ) ) ;
#19181 = CARTESIAN_POINT ( 'NONE',  ( 19.52812500061451573, -4.541064518000419881, 2.621784821874995952 ) ) ;
#19182 = CARTESIAN_POINT ( 'NONE',  ( 23.45625000122903359, -4.330127018922190985, -2.500000000000001332 ) ) ;
#19183 = ORIENTED_EDGE ( 'NONE', *, *, #72365, .F. ) ;
#19184 = CARTESIAN_POINT ( 'NONE',  ( 24.22500000000000142, -4.330127018922194537, 2.499999999999995559 ) ) ;
#19185 = CARTESIAN_POINT ( 'NONE',  ( -3.999999999999999556, 10.51250000000000107, -32.30940107675850470 ) ) ;
#19186 = CARTESIAN_POINT ( 'NONE',  ( -3.756430356250000102, 18.82812499938548356, 30.00000000000000000 ) ) ;
#19187 = CARTESIAN_POINT ( 'NONE',  ( 27.02812500061451573, 4.541064518000418104, 2.621784821874999949 ) ) ;
#19188 = CARTESIAN_POINT ( 'NONE',  ( 7.978125000614517681, 6.421520780324663323E-16, -5.243569643749999010 ) ) ;
#19189 = CARTESIAN_POINT ( 'NONE',  ( 20.02500000122903145, 2.886751345948129099, -4.999999999999998224 ) ) ;
#19190 = CARTESIAN_POINT ( 'NONE',  ( 25.19062500061451715, 6.054752690667223547, 3.707466751127219781E-16 ) ) ;
#19191 = CARTESIAN_POINT ( 'NONE',  ( 26.28749999999999432, 5.773502691896255534, 3.535250795749688894E-16 ) ) ;
#19192 = CARTESIAN_POINT ( 'NONE',  ( 3.999999999999999112, 15.38750000122903394, -30.00000000000000000 ) ) ;
#19193 = CARTESIAN_POINT ( 'NONE',  ( -1.071796769724491005, 15.52009619066136814, -34.00000000000000000 ) ) ;
#19194 = CARTESIAN_POINT ( 'NONE',  ( 9.440625000614517148, 6.054752690667223547, 3.707466751127219781E-16 ) ) ;
#19195 = ORIENTED_EDGE ( 'NONE', *, *, #65590, .F. ) ;
#19196 = CARTESIAN_POINT ( 'NONE',  ( 24.81562500061451715, 3.027376345333611329, 5.243569643749999010 ) ) ;
#19197 = CARTESIAN_POINT ( 'NONE',  ( 5.728125000614515905, 6.421520780324663323E-16, -5.243569643749999010 ) ) ;
#19198 = CARTESIAN_POINT ( 'NONE',  ( 14.22187500061451537, -5.492252693125287522, -1.008910452111647106E-15 ) ) ;
#19199 = EDGE_CURVE ( 'NONE', #71220, #7083, #59197, .T. ) ;
#19200 = CARTESIAN_POINT ( 'NONE',  ( 17.77500000122903501, 2.886751345948129099, -4.999999999999997335 ) ) ;
#19201 = CARTESIAN_POINT ( 'NONE',  ( 12.78749999999999964, 5.773502691896255534, 3.535250795749688894E-16 ) ) ;
#19202 = CARTESIAN_POINT ( 'NONE',  ( 14.40937500061451715, 4.541064518000418104, -2.621784821874998173 ) ) ;
#19203 = CARTESIAN_POINT ( 'NONE',  ( 7.912500001229033408, 4.330127018922192761, -2.499999999999997780 ) ) ;
#19204 = CARTESIAN_POINT ( 'NONE',  ( 18.00937500061451502, 4.541064518000418104, -2.621784821874998173 ) ) ;
#19205 = CARTESIAN_POINT ( 'NONE',  ( 17.28750000000000142, 5.773502691896255534, 3.535250795749688894E-16 ) ) ;
#19206 = CARTESIAN_POINT ( 'NONE',  ( 8.934375000614517504, 6.421520780324663323E-16, -5.243569643749999010 ) ) ;
#19207 = CARTESIAN_POINT ( 'NONE',  ( 4.243569643749999898, 11.47812500061451679, -30.00000000000000000 ) ) ;
#19208 = CARTESIAN_POINT ( 'NONE',  ( -3.999999999999997335, 11.93750000000000000, -27.69059892324149530 ) ) ;
#19209 = CARTESIAN_POINT ( 'NONE',  ( 22.20937500061451786, -5.492252693125287522, -1.008910452111647106E-15 ) ) ;
#19210 = VERTEX_POINT ( 'NONE', #50055 ) ;
#19211 = CARTESIAN_POINT ( 'NONE',  ( 25.04062500061451502, -3.027376345333610441, -5.243569643749999898 ) ) ;
#19212 = CARTESIAN_POINT ( 'NONE',  ( 7.320879633048903241E-15, 17.30000000122903003, 26.00000000000000355 ) ) ;
#19213 = CARTESIAN_POINT ( 'NONE',  ( 26.29687500061451644, -3.027376345333614438, 5.243569643749998122 ) ) ;
#19214 =( BOUNDED_CURVE ( )  B_SPLINE_CURVE ( 2, ( #23027, #7132, #45216, #6411, #44861, #29662, #11234 ),
 .UNSPECIFIED., .F., .F. ) 
 B_SPLINE_CURVE_WITH_KNOTS ( ( 3, 2, 2, 3 ),
 ( 0.6583333333333334370, 0.6611111111111112049, 0.6638888888888888618, 0.6666666666666666297 ),
 .UNSPECIFIED. ) 
 CURVE ( )  GEOMETRIC_REPRESENTATION_ITEM ( )  RATIONAL_B_SPLINE_CURVE ( ( 0.9999999999999946709, 0.8660254037844440367, 1.000000000000000000, 0.8660254037844387076, 1.000000000000000000, 0.8660254037844387076, 1.000000000000000000 ) ) 
 REPRESENTATION_ITEM ( '' )  );
#19215 = CARTESIAN_POINT ( 'NONE',  ( 29.67187500061451644, 3.027376345333613106, -5.243569643749998122 ) ) ;
#19216 = CARTESIAN_POINT ( 'NONE',  ( 20.85000000000000142, 4.330127018922192761, -2.499999999999997780 ) ) ;
#19217 = CARTESIAN_POINT ( 'NONE',  ( 5.203125000614518214, -4.541064518000417216, -2.621784821875001281 ) ) ;
#19218 = CARTESIAN_POINT ( 'NONE',  ( 21.57187500061451146, 4.119189519843966529, 2.378215178124999607 ) ) ;
#19219 = CARTESIAN_POINT ( 'NONE',  ( 15.49687500061451750, -3.027376345333614438, 5.243569643749998122 ) ) ;
#19220 = CARTESIAN_POINT ( 'NONE',  ( 8.184375000614515727, -2.746126346562646425, 4.756430356249996549 ) ) ;
#19221 = CARTESIAN_POINT ( 'NONE',  ( 29.66250000122903074, 0.000000000000000000, 4.999999999999998224 ) ) ;
#19222 = CARTESIAN_POINT ( 'NONE',  ( 9.234375000614518214, -4.541064518000419881, 2.621784821874995952 ) ) ;
#19223 = CARTESIAN_POINT ( 'NONE',  ( 18.12187500061451573, 3.027376345333611329, 5.243569643749999010 ) ) ;
#19224 = CARTESIAN_POINT ( 'NONE',  ( -3.794534703783686069, 25.05380129398097822, 31.29271267519124322 ) ) ;
#19225 = CARTESIAN_POINT ( 'NONE',  ( 26.02499999999999858, -4.330127018922194537, 2.499999999999995559 ) ) ;
#19226 = CARTESIAN_POINT ( 'NONE',  ( 27.42187500061451644, 3.027376345333613106, -5.243569643749998122 ) ) ;
#19227 = FACE_OUTER_BOUND ( 'NONE', #55962, .T. ) ;
#19228 = VERTEX_POINT ( 'NONE', #23050 ) ;
#19229 = CARTESIAN_POINT ( 'NONE',  ( 8.062500000000000000, -5.773502691896255534, -1.060575238724906372E-15 ) ) ;
#19230 = CARTESIAN_POINT ( 'NONE',  ( 11.14687500061451608, 4.119189519843966529, -2.378215178124998275 ) ) ;
#19231 = CARTESIAN_POINT ( 'NONE',  ( 22.00312500061451360, 4.541064518000418104, -2.621784821874998173 ) ) ;
#19232 = CARTESIAN_POINT ( 'NONE',  ( 11.88749999999999751, 5.773502691896255534, 3.535250795749688894E-16 ) ) ;
#19233 = CARTESIAN_POINT ( 'NONE',  ( 7.687500001229033764, -4.330127018922194537, 2.499999999999995559 ) ) ;
#19234 = CARTESIAN_POINT ( 'NONE',  ( 6.853125000614516793, 0.000000000000000000, 5.243569643749999010 ) ) ;
#19235 = CARTESIAN_POINT ( 'NONE',  ( 21.56250000000000000, -5.773502691896255534, -1.060575238724906372E-15 ) ) ;
#19236 = CARTESIAN_POINT ( 'NONE',  ( 20.27812500061451573, 4.541064518000418104, 2.621784821874999949 ) ) ;
#19237 = DIRECTION ( 'NONE',  ( -0.000000000000000000, -1.000000000000000000, -0.000000000000000000 ) ) ;
#19238 = CARTESIAN_POINT ( 'NONE',  ( 26.62500000122903288, -5.773502691896255534, -1.060575238724906372E-15 ) ) ;
#19239 = CARTESIAN_POINT ( 'NONE',  ( -3.756430356250000990, 18.75312499938548427, 32.16877607737301048 ) ) ;
#19240 = CARTESIAN_POINT ( 'NONE',  ( 4.012500000000001954, -5.773502691896255534, -1.060575238724906372E-15 ) ) ;
#19241 = EDGE_LOOP ( 'NONE', ( #16212, #48050, #12283, #8666 ) ) ;
#19242 = CARTESIAN_POINT ( 'NONE',  ( 18.36562500061451431, 3.027376345333613106, -5.243569643749998122 ) ) ;
#19243 = CARTESIAN_POINT ( 'NONE',  ( 27.70312500061451289, -4.541064518000417216, -2.621784821875001281 ) ) ;
#19244 = CARTESIAN_POINT ( 'NONE',  ( 26.22187500061451715, 3.027376345333611329, 5.243569643749999010 ) ) ;
#19245 = CARTESIAN_POINT ( 'NONE',  ( 14.54062500061451679, -3.027376345333614438, 5.243569643749998122 ) ) ;
#19246 = CARTESIAN_POINT ( 'NONE',  ( 29.24062500061451431, 6.054752690667223547, 3.707466751127219781E-16 ) ) ;
#19247 = CARTESIAN_POINT ( 'NONE',  ( 8.803125000614517859, -4.541064518000417216, -2.621784821875001281 ) ) ;
#19248 = DIRECTION ( 'NONE',  ( 0.000000000000000000, 0.000000000000000000, -1.000000000000000000 ) ) ;
#19249 = CARTESIAN_POINT ( 'NONE',  ( 26.06250000122903288, 0.000000000000000000, 4.999999999999998224 ) ) ;
#19250 = CARTESIAN_POINT ( 'NONE',  ( 19.09687500061451360, -2.746126346562646425, 4.756430356249996549 ) ) ;
#19251 = CARTESIAN_POINT ( 'NONE',  ( 16.64062500061451289, 6.054752690667223547, 3.707466751127219781E-16 ) ) ;
#19252 = LINE ( 'NONE', #37637, #44520 ) ;
#19253 = CARTESIAN_POINT ( 'NONE',  ( 28.65937500061451715, -4.541064518000417216, -2.621784821875001281 ) ) ;
#19254 = CARTESIAN_POINT ( 'NONE',  ( 11.07187500061451679, -6.054752690667223547, -1.112240025338166033E-15 ) ) ;
#19255 = CARTESIAN_POINT ( 'NONE',  ( 9.009375000614518569, 4.541064518000418104, -2.621784821874998173 ) ) ;
#19256 = CARTESIAN_POINT ( 'NONE',  ( 18.75937500061451857, -4.541064518000417216, -2.621784821875001281 ) ) ;
#19257 = VERTEX_POINT ( 'NONE', #22331 ) ;
#19258 = CARTESIAN_POINT ( 'NONE',  ( 1.592000809091587073E-14, 15.95000000122903394, 26.00000000000000000 ) ) ;
#19259 = CARTESIAN_POINT ( 'NONE',  ( 22.82812500061451644, 6.421520780324663323E-16, -5.243569643749999010 ) ) ;
#19260 = EDGE_CURVE ( 'NONE', #46535, #41088, #64384, .T. ) ;
#19261 = CARTESIAN_POINT ( 'NONE',  ( 17.55937500061451573, 4.541064518000418104, -2.621784821874998173 ) ) ;
#19262 = CARTESIAN_POINT ( 'NONE',  ( 22.07812500061451644, 4.541064518000418104, 2.621784821874999949 ) ) ;
#19263 = CARTESIAN_POINT ( 'NONE',  ( 2.000000000000001332, 14.30000000000000071, 33.46410161513774995 ) ) ;
#19264 = CARTESIAN_POINT ( 'NONE',  ( 26.01562500061451289, 3.027376345333613106, -5.243569643749998122 ) ) ;
#19265 = CARTESIAN_POINT ( 'NONE',  ( 9.337500001229033231, 4.330127018922191873, 2.499999999999999556 ) ) ;
#19266 = ORIENTED_EDGE ( 'NONE', *, *, #48691, .T. ) ;
#19267 = CARTESIAN_POINT ( 'NONE',  ( 5.325000001229033941, 2.886751345948126879, 4.999999999999999112 ) ) ;
#19268 = CARTESIAN_POINT ( 'NONE',  ( 2.000000000000001332, 18.35000000000000142, -26.53589838486224650 ) ) ;
#19269 = CARTESIAN_POINT ( 'NONE',  ( 23.85000000122903430, -2.886751345948129988, 4.999999999999997335 ) ) ;
#19270 = CARTESIAN_POINT ( 'NONE',  ( 0.6945855708053418898, 20.89427347822356040, 33.93923227099254092 ) ) ;
#19271 = EDGE_CURVE ( 'NONE', #60913, #7096, #13465, .T. ) ;
#19272 = CARTESIAN_POINT ( 'NONE',  ( 6.759375000614516793, 4.541064518000418104, -2.621784821874998173 ) ) ;
#19273 = CARTESIAN_POINT ( 'NONE',  ( 1.071796769724491893, 9.895096190661368141, 33.99999999999999289 ) ) ;
#19274 = CARTESIAN_POINT ( 'NONE',  ( 16.07812500061451289, 6.421520780324663323E-16, -5.243569643749999010 ) ) ;
#19275 = CARTESIAN_POINT ( 'NONE',  ( 11.14687500061451608, -3.027376345333610441, -5.243569643749999898 ) ) ;
#19276 = CARTESIAN_POINT ( 'NONE',  ( 26.17500000122903359, -5.773502691896255534, -1.060575238724906372E-15 ) ) ;
#19277 =( BOUNDED_CURVE ( )  B_SPLINE_CURVE ( 2, ( #28776, #40234, #50596, #73118, #17323, #720, #23227 ),
 .UNSPECIFIED., .F., .F. ) 
 B_SPLINE_CURVE_WITH_KNOTS ( ( 3, 2, 2, 3 ),
 ( 0.000000000000000000, 0.002777777777777771812, 0.005555555555555543625, 0.008333333333333315870 ),
 .UNSPECIFIED. ) 
 CURVE ( )  GEOMETRIC_REPRESENTATION_ITEM ( )  RATIONAL_B_SPLINE_CURVE ( ( 1.000000000000000000, 0.8660254037844387076, 1.000000000000000000, 0.8660254037844387076, 1.000000000000000000, 0.8660254037844395958, 0.9999999999999991118 ) ) 
 REPRESENTATION_ITEM ( '' )  );
#19278 = CARTESIAN_POINT ( 'NONE',  ( 16.54687500061451644, -3.027376345333610441, -5.243569643749999898 ) ) ;
#19279 = CARTESIAN_POINT ( 'NONE',  ( 5.896875000614518747, 6.054752690667223547, 3.707466751127219781E-16 ) ) ;
#19280 = CYLINDRICAL_SURFACE ( 'NONE', #42732, 4.999999999999998224 ) ;
#19281 = EDGE_CURVE ( 'NONE', #47295, #21571, #46495, .T. ) ;
#19282 = CARTESIAN_POINT ( 'NONE',  ( 7.228125000614517681, 4.541064518000418104, 2.621784821874999949 ) ) ;
#19283 =( BOUNDED_CURVE ( )  B_SPLINE_CURVE ( 2, ( #28087, #39169, #21795, #72784, #5904, #370, #27357 ),
 .UNSPECIFIED., .F., .F. ) 
 B_SPLINE_CURVE_WITH_KNOTS ( ( 3, 2, 2, 3 ),
 ( 0.9940063808490070540, 0.9944444444444444642, 0.9972222222222222321, 0.9975950399704071048 ),
 .UNSPECIFIED. ) 
 CURVE ( )  GEOMETRIC_REPRESENTATION_ITEM ( )  RATIONAL_B_SPLINE_CURVE ( ( 0.9644075875924971175, 0.9788718184064328920, 1.000000000000000000, 0.8660254037844387076, 1.000000000000000000, 0.9820186813809772541, 0.9688640661581504610 ) ) 
 REPRESENTATION_ITEM ( '' )  );
#19284 = CARTESIAN_POINT ( 'NONE',  ( 17.42812500061451786, 6.421520780324663323E-16, -5.243569643749999010 ) ) ;
#19285 = EDGE_LOOP ( 'NONE', ( #35800, #17561, #34599, #70282 ) ) ;
#19286 = CARTESIAN_POINT ( 'NONE',  ( 14.95312500061451644, 0.000000000000000000, 5.243569643749999010 ) ) ;
#19287 = CARTESIAN_POINT ( 'NONE',  ( 10.79062500061451679, 6.054752690667223547, 3.707466751127219781E-16 ) ) ;
#19288 = CARTESIAN_POINT ( 'NONE',  ( 21.19687500061451502, 5.492252693125287522, 3.363034840372157021E-16 ) ) ;
#19289 = CARTESIAN_POINT ( 'NONE',  ( 10.61250000000000071, 2.886751345948126879, 4.999999999999999112 ) ) ;
#19290 = CARTESIAN_POINT ( 'NONE',  ( 6.000000001229033764, -2.886751345948125991, -5.000000000000000000 ) ) ;
#19291 =( BOUNDED_CURVE ( )  B_SPLINE_CURVE ( 2, ( #471, #1928, #64690, #12986, #8178, #53985, #41439 ),
 .UNSPECIFIED., .F., .F. ) 
 B_SPLINE_CURVE_WITH_KNOTS ( ( 3, 2, 2, 3 ),
 ( 0.9172137518328628003, 0.9194444444444443976, 0.9222222222222222765, 0.9240845911989643557 ),
 .UNSPECIFIED. ) 
 CURVE ( )  GEOMETRIC_REPRESENTATION_ITEM ( )  RATIONAL_B_SPLINE_CURVE ( ( 0.9576208616715126132, 0.8924117889096346845, 1.000000000000000000, 0.8660254037844387076, 1.000000000000000000, 0.9101763526011728000, 0.9407977426935905108 ) ) 
 REPRESENTATION_ITEM ( '' )  );
#19292 = CARTESIAN_POINT ( 'NONE',  ( 15.27187500061451786, 3.027376345333613106, -5.243569643749998122 ) ) ;
#19293 = CARTESIAN_POINT ( 'NONE',  ( 15.52500000122903323, 2.886751345948129099, -4.999999999999998224 ) ) ;
#19294 = CARTESIAN_POINT ( 'NONE',  ( 23.58749999999999858, 5.773502691896255534, 3.535250795749688894E-16 ) ) ;
#19295 = CARTESIAN_POINT ( 'NONE',  ( -4.243569643749997233, 18.04062500061451857, -27.54997392385601174 ) ) ;
#19296 = CARTESIAN_POINT ( 'NONE',  ( 11.88750000122903216, 6.123233995736764310E-16, -4.999999999999998224 ) ) ;
#19297 = CARTESIAN_POINT ( 'NONE',  ( -3.999999999999999112, 18.61250000000000426, 27.69059892324149885 ) ) ;
#19298 = CARTESIAN_POINT ( 'NONE',  ( 23.02500000122903856, -5.773502691896255534, -1.060575238724906372E-15 ) ) ;
#19299 = EDGE_CURVE ( 'NONE', #68293, #7272, #27160, .T. ) ;
#19300 = FACE_OUTER_BOUND ( 'NONE', #34060, .T. ) ;
#19301 = CARTESIAN_POINT ( 'NONE',  ( 3.886657622141069357, -3.145466273087292208, -4.195369635725843871 ) ) ;
#19302 = CARTESIAN_POINT ( 'NONE',  ( 17.07187500061451502, 3.027376345333613106, -5.243569643749998122 ) ) ;
#19303 = CARTESIAN_POINT ( 'NONE',  ( 28.53749999999999787, 5.773502691896255534, 3.535250795749688894E-16 ) ) ;
#19304 = CARTESIAN_POINT ( 'NONE',  ( 13.71562500061451750, -6.054752690667223547, -1.112240025338166033E-15 ) ) ;
#19305 = CARTESIAN_POINT ( 'NONE',  ( 29.18437500061451217, 5.492252693125287522, 3.363034840372157021E-16 ) ) ;
#19306 = CARTESIAN_POINT ( 'NONE',  ( 23.89687500061451786, 6.054752690667223547, 3.707466751127219781E-16 ) ) ;
#19307 = CARTESIAN_POINT ( 'NONE',  ( 16.02187500061451431, 5.824947211148865298E-16, -4.756430356249998326 ) ) ;
#19308 = CARTESIAN_POINT ( 'NONE',  ( 10.94062500061451537, -3.027376345333614438, 5.243569643749998122 ) ) ;
#19309 = CARTESIAN_POINT ( 'NONE',  ( 15.87187500061451573, 3.027376345333611329, 5.243569643749999010 ) ) ;
#19310 = EDGE_LOOP ( 'NONE', ( #31857, #61807, #29336, #36069 ) ) ;
#19311 = CARTESIAN_POINT ( 'NONE',  ( 26.25937500061451857, 0.000000000000000000, 5.243569643749999010 ) ) ;
#19312 = CARTESIAN_POINT ( 'NONE',  ( 28.11562500061451431, -6.054752690667223547, -1.112240025338166033E-15 ) ) ;
#19313 = CARTESIAN_POINT ( 'NONE',  ( 18.96562500061451573, 3.027376345333611329, 5.243569643749999010 ) ) ;
#19314 = CARTESIAN_POINT ( 'NONE',  ( 12.22499999999999964, 6.123233995736764310E-16, -4.999999999999998224 ) ) ;
#19315 = FACE_OUTER_BOUND ( 'NONE', #54066, .T. ) ;
#19316 = CARTESIAN_POINT ( 'NONE',  ( 6.899999999999999467, 4.330127018922192761, -2.499999999999997780 ) ) ;
#19317 = CARTESIAN_POINT ( 'NONE',  ( 18.86250000122903359, 0.000000000000000000, 4.999999999999998224 ) ) ;
#19318 = CARTESIAN_POINT ( 'NONE',  ( -1.487416814333745711E-14, 15.16250000000000142, -26.00000000000000000 ) ) ;
#19319 = CARTESIAN_POINT ( 'NONE',  ( 10.73437500061451644, 5.492252693125287522, 3.363034840372157021E-16 ) ) ;
#19320 = ORIENTED_EDGE ( 'NONE', *, *, #3723, .T. ) ;
#19321 = CARTESIAN_POINT ( 'NONE',  ( 16.87500000000000000, 4.330127018922191873, 2.499999999999999556 ) ) ;
#19322 = CARTESIAN_POINT ( 'NONE',  ( 19.38749999999999929, -2.886751345948125991, -5.000000000000000000 ) ) ;
#19323 = CARTESIAN_POINT ( 'NONE',  ( 17.85937500061451999, -4.541064518000417216, -2.621784821875001281 ) ) ;
#19324 = CARTESIAN_POINT ( 'NONE',  ( 13.94062500061451892, 6.054752690667223547, 3.707466751127219781E-16 ) ) ;
#19325 = ORIENTED_EDGE ( 'NONE', *, *, #37028, .F. ) ;
#19326 = CARTESIAN_POINT ( 'NONE',  ( 10.42500000000000071, 6.123233995736764310E-16, -4.999999999999998224 ) ) ;
#19327 = CARTESIAN_POINT ( 'NONE',  ( 6.890625000614516438, -3.027376345333614438, 5.243569643749998122 ) ) ;
#19328 = CARTESIAN_POINT ( 'NONE',  ( -4.000000000000000888, 14.11250000000000071, 32.30940107675850470 ) ) ;
#19329 = CARTESIAN_POINT ( 'NONE',  ( 13.01249999999999929, -5.773502691896255534, -1.060575238724906372E-15 ) ) ;
#19330 = CARTESIAN_POINT ( 'NONE',  ( 29.70937500061451431, 2.746126346562643317, 4.756430356249998326 ) ) ;
#19331 = VECTOR ( 'NONE', #54461, 1000.000000000000000 ) ;
#19332 = CARTESIAN_POINT ( 'NONE',  ( -2.121784821874999949, 14.77812500061451750, 26.32496088578401938 ) ) ;
#19333 = CARTESIAN_POINT ( 'NONE',  ( 26.87812500061451360, 6.421520780324663323E-16, -5.243569643749999010 ) ) ;
#19334 = CARTESIAN_POINT ( 'NONE',  ( 7.912499999999999645, 2.886751345948126879, 4.999999999999999112 ) ) ;
#19335 = CARTESIAN_POINT ( 'NONE',  ( -7.967954043666661671E-16, 17.92812499938548498, 34.33755215474603517 ) ) ;
#19336 = CARTESIAN_POINT ( 'NONE',  ( 24.64687500061451431, -3.027376345333610441, -5.243569643749999898 ) ) ;
#19337 = EDGE_LOOP ( 'NONE', ( #17398, #8334, #42234, #15604 ) ) ;
#19338 = CARTESIAN_POINT ( 'NONE',  ( 22.07812500061451644, 4.541064518000418104, 2.621784821874999949 ) ) ;
#19339 = CARTESIAN_POINT ( 'NONE',  ( 22.17187500061451644, 3.027376345333611329, 5.243569643749999010 ) ) ;
#19340 = CARTESIAN_POINT ( 'NONE',  ( -3.000416591977282496E-16, 16.99062500061459247, -34.90005215228797653 ) ) ;
#19341 = CARTESIAN_POINT ( 'NONE',  ( 7.565625000614518036, 3.027376345333613106, -5.243569643749998122 ) ) ;
#19342 = CARTESIAN_POINT ( 'NONE',  ( 25.80937500061451928, 0.000000000000000000, 4.756430356249998326 ) ) ;
#19343 = CARTESIAN_POINT ( 'NONE',  ( 23.91562500061451502, 3.027376345333611329, 5.243569643749999010 ) ) ;
#19344 = CARTESIAN_POINT ( 'NONE',  ( 9.421875000614519990, 2.746126346562645981, -4.756430356249997438 ) ) ;
#19345 = CARTESIAN_POINT ( 'NONE',  ( 2.655984681222220721E-16, 15.45312499938548179, 25.66244784525396483 ) ) ;
#19346 = CARTESIAN_POINT ( 'NONE',  ( 17.70937500061451431, 0.000000000000000000, 5.243569643749999010 ) ) ;
#19347 = CARTESIAN_POINT ( 'NONE',  ( 25.69687500061451502, 6.054752690667223547, 3.707466751127219781E-16 ) ) ;
#19348 = CARTESIAN_POINT ( 'NONE',  ( -3.000416591977282496E-16, 13.89687500061451608, 25.09994784771203058 ) ) ;
#19349 = CARTESIAN_POINT ( 'NONE',  ( 7.790625000614518569, -3.027376345333614438, 5.243569643749998122 ) ) ;
#19350 = CARTESIAN_POINT ( 'NONE',  ( 29.61562500061451431, 3.027376345333613106, -5.243569643749998122 ) ) ;
#19351 = CARTESIAN_POINT ( 'NONE',  ( 29.09062500061451573, -3.027376345333610441, -5.243569643749999898 ) ) ;
#19352 = CARTESIAN_POINT ( 'NONE',  ( 26.43749999999999645, -2.886751345948146863, 4.999999999999968026 ) ) ;
#19353 = CARTESIAN_POINT ( 'NONE',  ( 4.378125000614518925, 6.421520780324663323E-16, -5.243569643749999010 ) ) ;
#19354 = CARTESIAN_POINT ( 'NONE',  ( 9.534375000614517148, 4.541064518000418104, 2.621784821874999949 ) ) ;
#19355 = FILL_AREA_STYLE ('',( #25274 ) ) ;
#19356 = CARTESIAN_POINT ( 'NONE',  ( 16.38750000122903216, 6.123233995736764310E-16, -4.999999999999998224 ) ) ;
#19357 = CARTESIAN_POINT ( 'NONE',  ( 29.72812500061451502, 4.541064518000418104, 2.621784821874999949 ) ) ;
#19358 = CARTESIAN_POINT ( 'NONE',  ( 5.540625000614515905, -3.027376345333614438, 5.243569643749998122 ) ) ;
#19359 = CARTESIAN_POINT ( 'NONE',  ( -3.999999999999999556, 14.43124999877096570, 27.69059892324149175 ) ) ;
#19360 = CARTESIAN_POINT ( 'NONE',  ( 21.39375000122903359, 5.773502691896255534, 3.535250795749688894E-16 ) ) ;
#19361 = CARTESIAN_POINT ( 'NONE',  ( 16.47187500061452070, -6.054752690667223547, -1.112240025338166033E-15 ) ) ;
#19362 = EDGE_LOOP ( 'NONE', ( #1060, #36798, #38764, #39577 ) ) ;
#19363 = CARTESIAN_POINT ( 'NONE',  ( 22.00312500061451360, 4.541064518000418104, -2.621784821874998173 ) ) ;
#19364 = CARTESIAN_POINT ( 'NONE',  ( 10.56562500061451715, -6.054752690667223547, -1.112240025338166033E-15 ) ) ;
#19365 = CARTESIAN_POINT ( 'NONE',  ( 25.35937500061451644, 0.000000000000000000, 5.243569643749999010 ) ) ;
#19366 = CARTESIAN_POINT ( 'NONE',  ( 7.078125000614516438, 6.421520780324663323E-16, -5.243569643749999010 ) ) ;
#19367 = CARTESIAN_POINT ( 'NONE',  ( 20.40000000000000213, 4.330127018922192761, -2.499999999999997780 ) ) ;
#19368 = CARTESIAN_POINT ( 'NONE',  ( 11.13750000122903216, 4.330127018922191873, 2.499999999999999556 ) ) ;
#19369 = EDGE_CURVE ( 'NONE', #70824, #9005, #10164, .T. ) ;
#19370 = CARTESIAN_POINT ( 'NONE',  ( 24.74062500061451786, 6.054752690667223547, 3.707466751127219781E-16 ) ) ;
#19371 = CARTESIAN_POINT ( 'NONE',  ( 4.243569643749999898, 10.09062500061451928, -27.54997392385601529 ) ) ;
#19372 = CARTESIAN_POINT ( 'NONE',  ( 13.08750000122903323, -4.330127018922194537, 2.499999999999995559 ) ) ;
#19373 = CARTESIAN_POINT ( 'NONE',  ( 21.55312500061451431, 4.541064518000418104, -2.621784821874998173 ) ) ;
#19374 = CARTESIAN_POINT ( 'NONE',  ( 17.91562500061451502, 3.027376345333613106, -5.243569643749998122 ) ) ;
#19375 = FACE_OUTER_BOUND ( 'NONE', #6414, .T. ) ;
#19376 = CARTESIAN_POINT ( 'NONE',  ( 17.58749999999999858, -2.886751345948125991, -5.000000000000000000 ) ) ;
#19377 = CARTESIAN_POINT ( 'NONE',  ( 13.98750000122903359, -4.330127018922194537, 2.499999999999995559 ) ) ;
#19378 = CARTESIAN_POINT ( 'NONE',  ( 11.46562500061451573, -6.054752690667223547, -1.112240025338166033E-15 ) ) ;
#19379 = CARTESIAN_POINT ( 'NONE',  ( 14.27812500061451573, 6.421520780324663323E-16, -5.243569643749999010 ) ) ;
#19380 = CARTESIAN_POINT ( 'NONE',  ( 22.95000000122903216, -2.886751345948129988, 4.999999999999997335 ) ) ;
#19381 = AXIS2_PLACEMENT_3D ( 'NONE', #28598, #51134, #532 ) ;
#19382 = CARTESIAN_POINT ( 'NONE',  ( 22.54687500061451999, 6.054752690667223547, 3.707466751127219781E-16 ) ) ;
#19383 = CARTESIAN_POINT ( 'NONE',  ( 21.90937500061451715, -4.541064518000417216, -2.621784821875001281 ) ) ;
#19384 = CYLINDRICAL_SURFACE ( 'NONE', #54798, 4.999999999999998224 ) ;
#19385 = CARTESIAN_POINT ( 'NONE',  ( 8.175000001229031810, -5.773502691896255534, -1.060575238724906372E-15 ) ) ;
#19386 = CARTESIAN_POINT ( 'NONE',  ( 7.471875000614519813, -6.054752690667223547, -1.112240025338166033E-15 ) ) ;
#19387 = CARTESIAN_POINT ( 'NONE',  ( 26.59687500061451360, 6.054752690667223547, 3.707466751127219781E-16 ) ) ;
#19388 = CARTESIAN_POINT ( 'NONE',  ( 4.731257479987296399, -1.617158822770780269, 4.897528984835215482 ) ) ;
#19389 = AXIS2_PLACEMENT_3D ( 'NONE', #61770, #49975, #11174 ) ;
#19390 = CARTESIAN_POINT ( 'NONE',  ( 21.21562500061451573, 3.027376345333611329, 5.243569643749999010 ) ) ;
#19391 = CARTESIAN_POINT ( 'NONE',  ( 26.29687500061451644, -3.027376345333614438, 5.243569643749998122 ) ) ;
#19392 = CARTESIAN_POINT ( 'NONE',  ( 1.878215178124997609, 18.07812499938548356, 33.25316411605952993 ) ) ;
#19393 = CARTESIAN_POINT ( 'NONE',  ( 3.479729569495786379, -3.590471016896914946, -3.821457900550485398 ) ) ;
#19394 = CARTESIAN_POINT ( 'NONE',  ( 11.11875000122903323, 2.886751345948182834, 4.999999999999902300 ) ) ;
#19395 = CARTESIAN_POINT ( 'NONE',  ( 4.659375000614518925, 0.000000000000000000, 5.243569643749999010 ) ) ;
#19396 = CARTESIAN_POINT ( 'NONE',  ( 18.44062500061451715, 6.054752690667223547, 3.707466751127219781E-16 ) ) ;
#19397 = VECTOR ( 'NONE', #60115, 1000.000000000000000 ) ;
#19398 = ORIENTED_EDGE ( 'NONE', *, *, #6200, .T. ) ;
#19399 = CARTESIAN_POINT ( 'NONE',  ( 11.47499999999999964, 4.330127018922191873, 2.499999999999999556 ) ) ;
#19400 = CARTESIAN_POINT ( 'NONE',  ( 25.52812500061451573, 6.421520780324663323E-16, -5.243569643749999010 ) ) ;
#19401 = CARTESIAN_POINT ( 'NONE',  ( 2.971875000614517592, -6.054752690667223547, -1.112240025338166033E-15 ) ) ;
#19402 = CARTESIAN_POINT ( 'NONE',  ( 4.688072943975824636, 1.738382027048589684, 4.849960349263820802 ) ) ;
#19403 = EDGE_CURVE ( 'NONE', #67375, #19923, #26224, .T. ) ;
#19404 = CARTESIAN_POINT ( 'NONE',  ( 4.078125000614517326, 4.541064518000418104, 2.621784821874999949 ) ) ;
#19405 = CARTESIAN_POINT ( 'NONE',  ( 16.19999999999999929, -4.330127018922190985, -2.500000000000001332 ) ) ;
#19406 = CARTESIAN_POINT ( 'NONE',  ( 21.85312500061451502, -4.541064518000417216, -2.621784821875001281 ) ) ;
#19407 = VERTEX_POINT ( 'NONE', #55235 ) ;
#19408 = CARTESIAN_POINT ( 'NONE',  ( 24.97499999999999787, 4.330127018922191873, 2.499999999999999556 ) ) ;
#19409 = CARTESIAN_POINT ( 'NONE',  ( 26.07187500061451857, 3.027376345333613106, -5.243569643749998122 ) ) ;
#19410 = ORIENTED_EDGE ( 'NONE', *, *, #37713, .F. ) ;
#19411 = CARTESIAN_POINT ( 'NONE',  ( 30.00000000000000000, 0.000000000000000000, 0.000000000000000000 ) ) ;
#19412 = CARTESIAN_POINT ( 'NONE',  ( 13.75312500061451715, -4.541064518000417216, -2.621784821875001281 ) ) ;
#19413 = CARTESIAN_POINT ( 'NONE',  ( 25.16250000122903074, 0.000000000000000000, 4.999999999999998224 ) ) ;
#19414 = CARTESIAN_POINT ( 'NONE',  ( 16.20937500061451431, 2.746126346562643317, 4.756430356249998326 ) ) ;
#19415 = CARTESIAN_POINT ( 'NONE',  ( 3.459375000614519635, -4.541064518000417216, -2.621784821875001281 ) ) ;
#19416 = CARTESIAN_POINT ( 'NONE',  ( 12.48750000122903359, 4.330127018922191873, 2.499999999999999556 ) ) ;
#19417 = CARTESIAN_POINT ( 'NONE',  ( 18.97499999999999787, 6.123233995736764310E-16, -4.999999999999998224 ) ) ;
#19418 = CARTESIAN_POINT ( 'NONE',  ( 27.15000000000000213, 4.330127018922192761, -2.499999999999997780 ) ) ;
#19419 = CARTESIAN_POINT ( 'NONE',  ( 3.275492200589926739, -3.777717676570560901, -3.275492200590059522 ) ) ;
#19420 = CARTESIAN_POINT ( 'NONE',  ( 7.359375000614516438, 0.000000000000000000, 5.243569643749999010 ) ) ;
#19421 = CARTESIAN_POINT ( 'NONE',  ( 18.45937500061451431, 4.541064518000418104, -2.621784821874998173 ) ) ;
#19422 = FACE_OUTER_BOUND ( 'NONE', #2144, .T. ) ;
#19423 = ORIENTED_EDGE ( 'NONE', *, *, #2520, .T. ) ;
#19424 = CARTESIAN_POINT ( 'NONE',  ( 28.30312500061451431, 4.541064518000418104, -2.621784821874998173 ) ) ;
#19425 = CARTESIAN_POINT ( 'NONE',  ( 3.000000000000002665, 0.000000000000000000, 4.999999999999998224 ) ) ;
#19426 = CARTESIAN_POINT ( 'NONE',  ( 3.571875000614517237, 3.027376345333613106, -5.243569643749998122 ) ) ;
#19427 = CARTESIAN_POINT ( 'NONE',  ( 15.29999999999999893, -4.330127018922190985, -2.500000000000001332 ) ) ;
#19428 = CARTESIAN_POINT ( 'NONE',  ( 13.37812500061451715, 6.421520780324663323E-16, -5.243569643749999010 ) ) ;
#19429 = CARTESIAN_POINT ( 'NONE',  ( -2.000000000000000000, 14.97499999999999964, -33.46410161513775705 ) ) ;
#19430 = CARTESIAN_POINT ( 'NONE',  ( 5.810221930991193690E-16, 17.95624999877096784, 26.00000000000000000 ) ) ;
#19431 = FACE_OUTER_BOUND ( 'NONE', #46352, .T. ) ;
#19432 = CARTESIAN_POINT ( 'NONE',  ( 17.88750000122903216, 4.330127018922191873, 2.499999999999999556 ) ) ;
#19433 = CARTESIAN_POINT ( 'NONE',  ( -1.071796769724502107, 19.32634618820330630, 26.00000000000000711 ) ) ;
#19434 = CARTESIAN_POINT ( 'NONE',  ( 17.10937500061451999, 4.119189519843966529, -2.378215178124998275 ) ) ;
#19435 = CARTESIAN_POINT ( 'NONE',  ( 7.940625000614518036, -3.027376345333610441, -5.243569643749999898 ) ) ;
#19436 = CARTESIAN_POINT ( 'NONE',  ( 23.18437500061451573, -4.541064518000419881, 2.621784821874995952 ) ) ;
#19437 = CARTESIAN_POINT ( 'NONE',  ( 9.001249775931846008E-16, 19.52187500061451786, 34.90005215228797653 ) ) ;
#19438 = CARTESIAN_POINT ( 'NONE',  ( 22.84687500061451715, -3.027376345333610441, -5.243569643749999898 ) ) ;
#19439 = CARTESIAN_POINT ( 'NONE',  ( 5.549999999999998934, 4.330127018922192761, -2.499999999999997780 ) ) ;
#19440 = CARTESIAN_POINT ( 'NONE',  ( -3.999999999999997335, 10.25000000122903288, 32.30940107675850470 ) ) ;
#19441 = CARTESIAN_POINT ( 'NONE',  ( 14.57812500061451644, -4.541064518000419881, 2.621784821874995952 ) ) ;
#19442 = CARTESIAN_POINT ( 'NONE',  ( 3.937500001229034208, 4.330127018922191873, 2.499999999999999556 ) ) ;
#19443 = CARTESIAN_POINT ( 'NONE',  ( 10.47187500061451715, 3.027376345333611329, 5.243569643749999010 ) ) ;
#19444 = CARTESIAN_POINT ( 'NONE',  ( 45.00000000000000000, 0.000000000000000000, 0.000000000000000000 ) ) ;
#19445 = ORIENTED_EDGE ( 'NONE', *, *, #20206, .F. ) ;
#19446 = VECTOR ( 'NONE', #41636, 1000.000000000000000 ) ;
#19447 = CARTESIAN_POINT ( 'NONE',  ( 12.40312500061451573, -4.541064518000417216, -2.621784821875001281 ) ) ;
#19448 = CARTESIAN_POINT ( 'NONE',  ( 29.13750000122903216, 4.330127018922191873, 2.499999999999999556 ) ) ;
#19449 = CARTESIAN_POINT ( 'NONE',  ( 23.88750000122903216, -4.330127018922194537, 2.499999999999995559 ) ) ;
#19450 = CARTESIAN_POINT ( 'NONE',  ( 10.35937500061451644, 4.541064518000418104, -2.621784821874998173 ) ) ;
#19451 = CARTESIAN_POINT ( 'NONE',  ( 11.95312500061451644, -4.541064518000417216, -2.621784821875001281 ) ) ;
#19452 = CARTESIAN_POINT ( 'NONE',  ( 27.31875000122903074, 2.886751345948126879, 4.999999999999999112 ) ) ;
#19453 = CARTESIAN_POINT ( 'NONE',  ( 22.73437500061451644, -4.541064518000419881, 2.621784821874995952 ) ) ;
#19454 = CYLINDRICAL_SURFACE ( 'NONE', #24246, 4.000000000000000000 ) ;
#19455 = CARTESIAN_POINT ( 'NONE',  ( 23.73749999999999716, -2.886751345948114000, 5.000000000000024869 ) ) ;
#19456 = CARTESIAN_POINT ( 'NONE',  ( 20.58750000122903145, 4.330127018922191873, 2.499999999999999556 ) ) ;
#19457 = CARTESIAN_POINT ( 'NONE',  ( -4.243569643749998122, 15.39687500061451786, -27.54997392385601174 ) ) ;
#19458 = CARTESIAN_POINT ( 'NONE',  ( 15.19687500061451857, -3.027376345333610441, -5.243569643749999898 ) ) ;
#19459 = CARTESIAN_POINT ( 'NONE',  ( 16.87500000122903288, 2.886751345948129099, -4.999999999999998224 ) ) ;
#19460 = EDGE_CURVE ( 'NONE', #56329, #40333, #29036, .T. ) ;
#19461 = AXIS2_PLACEMENT_3D ( 'NONE', #8368, #56526, #36807 ) ;
#19462 = CARTESIAN_POINT ( 'NONE',  ( 13.32187500061451502, -6.054752690667223547, -1.112240025338166033E-15 ) ) ;
#19463 = CARTESIAN_POINT ( 'NONE',  ( 2.121784821875001281, 16.80312500061451786, -26.32496088578401938 ) ) ;
#19464 = CARTESIAN_POINT ( 'NONE',  ( 20.81250000122903643, -4.330127018922190985, -2.500000000000001332 ) ) ;
#19465 = CARTESIAN_POINT ( 'NONE',  ( 13.60312500061451679, 0.000000000000000000, 5.243569643749999010 ) ) ;
#19466 = VERTEX_POINT ( 'NONE', #27521 ) ;
#19467 = ORIENTED_EDGE ( 'NONE', *, *, #15878, .F. ) ;
#19468 = VECTOR ( 'NONE', #54534, 1000.000000000000000 ) ;
#19469 = CARTESIAN_POINT ( 'NONE',  ( 14.66249999999999964, 2.886751345948126879, 4.999999999999999112 ) ) ;
#19470 = CARTESIAN_POINT ( 'NONE',  ( 11.97187500061451892, -6.054752690667223547, -1.112240025338166033E-15 ) ) ;
#19471 = CARTESIAN_POINT ( 'NONE',  ( 3.965171583692859603, 3.045884815923804556, 3.965171583692790325 ) ) ;
#19472 = CARTESIAN_POINT ( 'NONE',  ( 12.03750000122903430, 4.330127018922191873, 2.499999999999999556 ) ) ;
#19473 = CARTESIAN_POINT ( 'NONE',  ( 20.13750000122903216, 4.330127018922191873, 2.499999999999999556 ) ) ;
#19474 = CARTESIAN_POINT ( 'NONE',  ( 18.36562500061451431, 3.027376345333613106, -5.243569643749998122 ) ) ;
#19475 = CARTESIAN_POINT ( 'NONE',  ( 20.50312500061451715, -4.541064518000417216, -2.621784821875001281 ) ) ;
#19476 = CARTESIAN_POINT ( 'NONE',  ( 28.08750000122903145, 6.123233995736764310E-16, -4.999999999999998224 ) ) ;
#19477 = CARTESIAN_POINT ( 'NONE',  ( 26.02499999999999858, -4.330127018922194537, 2.499999999999995559 ) ) ;
#19478 = CARTESIAN_POINT ( 'NONE',  ( 4.869423765992945796, -1.135214599616954256, -5.119209941160161037 ) ) ;
#19479 = B_SPLINE_CURVE_WITH_KNOTS ( 'NONE', 3,
 ( #20484, #70741, #14586, #43039, #53761, #58913, #65566, #3155, #42674, #65197 ),
 .UNSPECIFIED., .F., .F.,
 ( 4, 3, 3, 4 ),
 ( 1.780036773976668796E-16, 2.812506838582382114E-05, 5.625013576972328906E-05, 9.339561289900664856E-05 ),
 .UNSPECIFIED. ) ;
#19480 = CARTESIAN_POINT ( 'NONE',  ( 29.06250000000000000, 2.886751345948126879, 4.999999999999999112 ) ) ;
#19481 = CARTESIAN_POINT ( 'NONE',  ( 28.02187500061451431, 3.027376345333611329, 5.243569643749999010 ) ) ;
#19482 = CARTESIAN_POINT ( 'NONE',  ( 3.990860739963187687, -3.012222745923910594, -4.182559159433559159 ) ) ;
#19483 = CARTESIAN_POINT ( 'NONE',  ( 4.243569643749999898, 12.84687500061451715, -27.54997392385601529 ) ) ;
#19484 = CARTESIAN_POINT ( 'NONE',  ( 4.387500001229033053, 4.330127018922191873, 2.499999999999999556 ) ) ;
#19485 = CARTESIAN_POINT ( 'NONE',  ( 4.987500000000002487, -2.886751345948125991, -5.000000000000000000 ) ) ;
#19486 = CARTESIAN_POINT ( 'NONE',  ( 28.85625000122903216, -4.330127018922190985, -2.500000000000001332 ) ) ;
#19487 = CARTESIAN_POINT ( 'NONE',  ( 8.559375000614515727, 4.541064518000418104, -2.621784821874998173 ) ) ;
#19488 = CARTESIAN_POINT ( 'NONE',  ( 27.92812500061451431, 4.541064518000418104, 2.621784821874999949 ) ) ;
#19489 = CARTESIAN_POINT ( 'NONE',  ( 1.999999999999998668, 10.85000000000000142, 26.53589838486224650 ) ) ;
#19490 = CARTESIAN_POINT ( 'NONE',  ( -4.112406224592633386, 9.116497278081073574, -25.62679350102753872 ) ) ;
#19491 = VECTOR ( 'NONE', #43108, 1000.000000000000227 ) ;
#19492 = PLANE ( 'NONE',  #22949 ) ;
#19493 = CARTESIAN_POINT ( 'NONE',  ( 5.521875000614517859, 3.027376345333611329, 5.243569643749999010 ) ) ;
#19494 = CARTESIAN_POINT ( 'NONE',  ( 10.69687500061451679, -3.027376345333610441, -5.243569643749999898 ) ) ;
#19495 = CARTESIAN_POINT ( 'NONE',  ( 4.575000000000002842, 6.123233995736764310E-16, -4.999999999999998224 ) ) ;
#19496 = CARTESIAN_POINT ( 'NONE',  ( -2.121784821874999949, 14.32812500061459460, 26.32496088578401938 ) ) ;
#19497 = CARTESIAN_POINT ( 'NONE',  ( 4.000000000000000000, 13.40000000000000036, 30.00000000000000000 ) ) ;
#19498 =( BOUNDED_CURVE ( )  B_SPLINE_CURVE ( 2, ( #33777, #10884, #56320, #44151, #17142, #72946, #4986 ),
 .UNSPECIFIED., .F., .F. ) 
 B_SPLINE_CURVE_WITH_KNOTS ( ( 3, 2, 2, 3 ),
 ( 0.6500000000000001332, 0.6527777777777779011, 0.6555555555555556690, 0.6583333333333334370 ),
 .UNSPECIFIED. ) 
 CURVE ( )  GEOMETRIC_REPRESENTATION_ITEM ( )  RATIONAL_B_SPLINE_CURVE ( ( 0.9999999999999946709, 0.8660254037844440367, 1.000000000000000000, 0.8660254037844387076, 1.000000000000000000, 0.8660254037844333785, 1.000000000000005329 ) ) 
 REPRESENTATION_ITEM ( '' )  );
#19499 = CARTESIAN_POINT ( 'NONE',  ( 7.425000000000000711, 4.330127018922191873, 2.499999999999999556 ) ) ;
#19500 = CARTESIAN_POINT ( 'NONE',  ( 16.17187500061451644, 4.119189519843966529, 2.378215178124999607 ) ) ;
#19501 = CARTESIAN_POINT ( 'NONE',  ( 20.46562500061451928, -6.054752690667223547, -1.112240025338166033E-15 ) ) ;
#19502 = CARTESIAN_POINT ( 'NONE',  ( 12.44062500061451537, -3.027376345333610441, -5.243569643749999898 ) ) ;
#19503 = CARTESIAN_POINT ( 'NONE',  ( 24.34687500061451715, 0.000000000000000000, 4.756430356249998326 ) ) ;
#19504 = CARTESIAN_POINT ( 'NONE',  ( 10.09687500061451715, -3.027376345333614438, 5.243569643749998122 ) ) ;
#19505 = CARTESIAN_POINT ( 'NONE',  ( 26.88749999999999574, -2.886751345948129988, 4.999999999999997335 ) ) ;
#19506 = CARTESIAN_POINT ( 'NONE',  ( 22.16250000122903074, -4.330127018922190985, -2.500000000000001332 ) ) ;
#19507 = DIRECTION ( 'NONE',  ( 0.000000000000000000, 0.000000000000000000, -1.000000000000000000 ) ) ;
#19508 = VECTOR ( 'NONE', #51786, 1000.000000000000000 ) ;
#19509 = CARTESIAN_POINT ( 'NONE',  ( 10.58437500061451964, -4.541064518000419881, 2.621784821874995952 ) ) ;
#19510 = CARTESIAN_POINT ( 'NONE',  ( 26.29687500061451644, -3.027376345333614438, 5.243569643749998122 ) ) ;
#19511 = CARTESIAN_POINT ( 'NONE',  ( 23.75625000122903074, 0.000000000000000000, 4.999999999999998224 ) ) ;
#19512 = DIRECTION ( 'NONE',  ( 0.000000000000000000, 0.000000000000000000, -1.000000000000000000 ) ) ;
#19513 = CARTESIAN_POINT ( 'NONE',  ( 21.00937500061451857, -4.541064518000417216, -2.621784821875001281 ) ) ;
#19514 = CARTESIAN_POINT ( 'NONE',  ( 11.10937500061451644, -4.541064518000417216, -2.621784821875001281 ) ) ;
#19515 = CARTESIAN_POINT ( 'NONE',  ( 3.756430356250000102, 20.40312499938548285, 30.00000000000000000 ) ) ;
#19516 = CARTESIAN_POINT ( 'NONE',  ( 23.40000000000000213, -4.330127018922190985, -2.500000000000001332 ) ) ;
#19517 = CARTESIAN_POINT ( 'NONE',  ( -1.999999999999999112, 15.35000000000000142, 26.53589838486224650 ) ) ;
#19518 = CARTESIAN_POINT ( 'NONE',  ( 4.243569643749999898, 12.84687500061451715, -27.54997392385601529 ) ) ;
#19519 = CARTESIAN_POINT ( 'NONE',  ( 23.70937500061451786, -4.119189519843965641, -2.378215178125001383 ) ) ;
#19520 = CARTESIAN_POINT ( 'NONE',  ( 15.85312500061451857, 0.000000000000000000, 5.243569643749999010 ) ) ;
#19521 = CARTESIAN_POINT ( 'NONE',  ( 3.712499999999999911, 2.886751345948129099, -4.999999999999998224 ) ) ;
#19522 = DIRECTION ( 'NONE',  ( -0.000000000000000000, -1.000000000000000000, -0.000000000000000000 ) ) ;
#19523 = DIRECTION ( 'NONE',  ( 0.000000000000000000, 0.000000000000000000, -1.000000000000000000 ) ) ;
#19524 = CARTESIAN_POINT ( 'NONE',  ( 15.00000000000000000, 4.330127018922192761, -2.499999999999997780 ) ) ;
#19525 = CARTESIAN_POINT ( 'NONE',  ( -3.999999999999997335, 17.45000000122903216, 32.30940107675850470 ) ) ;
#19526 = CARTESIAN_POINT ( 'NONE',  ( 13.76250000122903394, 4.330127018922192761, -2.499999999999997780 ) ) ;
#19527 = EDGE_CURVE ( 'NONE', #18820, #40294, #23837, .T. ) ;
#19528 = CARTESIAN_POINT ( 'NONE',  ( 25.13437500061451502, 6.421520780324663323E-16, -5.243569643749999010 ) ) ;
#19529 = CARTESIAN_POINT ( 'NONE',  ( 19.88437500061451857, 4.541064518000418104, 2.621784821874999949 ) ) ;
#19530 = CARTESIAN_POINT ( 'NONE',  ( 30.00000000000000000, 0.000000000000000000, 0.000000000000000000 ) ) ;
#19531 = VERTEX_POINT ( 'NONE', #51861 ) ;
#19532 = CARTESIAN_POINT ( 'NONE',  ( 19.64062500061451644, -3.027376345333610441, -5.243569643749999898 ) ) ;
#19533 = CARTESIAN_POINT ( 'NONE',  ( 3.253125000614518036, 0.000000000000000000, 5.243569643749999010 ) ) ;
#19534 = CARTESIAN_POINT ( 'NONE',  ( 17.14687500061451786, 6.054752690667223547, 3.707466751127219781E-16 ) ) ;
#19535 = CARTESIAN_POINT ( 'NONE',  ( 29.48437500061451644, -4.541064518000419881, 2.621784821874995952 ) ) ;
#19536 = CARTESIAN_POINT ( 'NONE',  ( 4.303125000614516971, -4.541064518000417216, -2.621784821875001281 ) ) ;
#19537 = CARTESIAN_POINT ( 'NONE',  ( 21.36562500061451431, -6.054752690667223547, -1.112240025338166033E-15 ) ) ;
#19538 = CARTESIAN_POINT ( 'NONE',  ( 9.001249775931846008E-16, 15.86562500061451608, 34.90005215228797653 ) ) ;
#19539 = CARTESIAN_POINT ( 'NONE',  ( 16.87500000122903288, 2.886751345948129099, -4.999999999999998224 ) ) ;
#19540 = CARTESIAN_POINT ( 'NONE',  ( 12.87187500061451750, -5.492252693125287522, -1.008910452111647106E-15 ) ) ;
#19541 = CARTESIAN_POINT ( 'NONE',  ( 6.553125000614518747, -4.541064518000417216, -2.621784821875001281 ) ) ;
#19542 = CARTESIAN_POINT ( 'NONE',  ( 3.834375000614519635, -4.541064518000419881, 2.621784821874995952 ) ) ;
#19543 = CARTESIAN_POINT ( 'NONE',  ( 28.75312500061451715, 4.541064518000418104, -2.621784821874998173 ) ) ;
#19544 = CARTESIAN_POINT ( 'NONE',  ( 23.89687500061451786, 6.054752690667223547, 3.707466751127219781E-16 ) ) ;
#19545 = CARTESIAN_POINT ( 'NONE',  ( 14.65312500061451573, -4.541064518000417216, -2.621784821875001281 ) ) ;
#19546 = CARTESIAN_POINT ( 'NONE',  ( 23.73750000122903359, 4.330127018922191873, 2.499999999999999556 ) ) ;
#19547 = ADVANCED_FACE ( 'NONE', ( #45960 ), #52223, .F. ) ;
#19548 = CARTESIAN_POINT ( 'NONE',  ( 24.40312500061451573, 0.000000000000000000, 5.243569643749999010 ) ) ;
#19549 = CARTESIAN_POINT ( 'NONE',  ( 20.40937500061451715, 0.000000000000000000, 5.243569643749999010 ) ) ;
#19550 = CARTESIAN_POINT ( 'NONE',  ( 13.71562500061451750, -6.054752690667223547, -1.112240025338166033E-15 ) ) ;
#19551 = CARTESIAN_POINT ( 'NONE',  ( -4.243569643749997233, 14.04687500061451999, 32.45002607614398471 ) ) ;
#19552 = CARTESIAN_POINT ( 'NONE',  ( 19.56562500061451715, -6.054752690667223547, -1.112240025338166033E-15 ) ) ;
#19553 = ORIENTED_EDGE ( 'NONE', *, *, #32305, .F. ) ;
#19554 = CARTESIAN_POINT ( 'NONE',  ( 25.80000000000000071, 4.330127018922192761, -2.499999999999997780 ) ) ;
#19555 = CARTESIAN_POINT ( 'NONE',  ( 2.000000000000001332, 11.60000000000000142, -26.53589838486224650 ) ) ;
#19556 = CARTESIAN_POINT ( 'NONE',  ( 12.56250000000000000, -5.773502691896255534, -1.060575238724906372E-15 ) ) ;
#19557 = AXIS2_PLACEMENT_3D ( 'NONE', #28510, #23319, #68044 ) ;
#19558 = CARTESIAN_POINT ( 'NONE',  ( 28.00312500061451715, 0.000000000000000000, 5.243569643749999010 ) ) ;
#19559 = CARTESIAN_POINT ( 'NONE',  ( 8.165625000614516793, 3.027376345333611329, 5.243569643749999010 ) ) ;
#19560 = CARTESIAN_POINT ( 'NONE',  ( 20.66250000122903074, 0.000000000000000000, 4.999999999999998224 ) ) ;
#19561 = CARTESIAN_POINT ( 'NONE',  ( 23.72812500061451502, 6.421520780324663323E-16, -5.243569643749999010 ) ) ;
#19562 = CARTESIAN_POINT ( 'NONE',  ( 26.55000000000000071, -4.330127018922190985, -2.500000000000001332 ) ) ;
#19563 = EDGE_CURVE ( 'NONE', #62090, #24437, #47045, .T. ) ;
#19564 = CARTESIAN_POINT ( 'NONE',  ( 27.40312500061451573, 4.541064518000418104, -2.621784821874998173 ) ) ;
#19565 = CARTESIAN_POINT ( 'NONE',  ( 8.315625000614515372, -6.054752690667223547, -1.112240025338166033E-15 ) ) ;
#19566 = EDGE_LOOP ( 'NONE', ( #29823, #23392, #23928, #33429 ) ) ;
#19567 = CARTESIAN_POINT ( 'NONE',  ( 25.86562500061451431, -6.054752690667223547, -1.112240025338166033E-15 ) ) ;
#19568 = CARTESIAN_POINT ( 'NONE',  ( 5.165625000614518569, -6.054752690667223547, -1.112240025338166033E-15 ) ) ;
#19569 = CARTESIAN_POINT ( 'NONE',  ( 13.65937500061451715, 0.000000000000000000, 4.756430356249998326 ) ) ;
#19570 = CYLINDRICAL_SURFACE ( 'NONE', #21991, 4.000000000000000000 ) ;
#19571 = CARTESIAN_POINT ( 'NONE',  ( 12.07499999999999929, -4.330127018922194537, 2.499999999999995559 ) ) ;
#19572 = CARTESIAN_POINT ( 'NONE',  ( 12.98437500061451821, 6.421520780324663323E-16, -5.243569643749999010 ) ) ;
#19573 = CARTESIAN_POINT ( 'NONE',  ( 9.487500001229033586, -4.330127018922194537, 2.499999999999995559 ) ) ;
#19574 = CARTESIAN_POINT ( 'NONE',  ( 16.32187500061451502, 3.027376345333611329, 5.243569643749999010 ) ) ;
#19575 = CARTESIAN_POINT ( 'NONE',  ( 15.82499999999999929, 6.123233995736764310E-16, -4.999999999999998224 ) ) ;
#19576 = CARTESIAN_POINT ( 'NONE',  ( 7.246875000614518392, 6.054752690667223547, 3.707466751127219781E-16 ) ) ;
#19577 = CARTESIAN_POINT ( 'NONE',  ( -2.121784821874996840, 11.32812500061451644, -26.32496088578401583 ) ) ;
#19578 = CARTESIAN_POINT ( 'NONE',  ( 20.21250000000000213, -5.773502691896255534, -1.060575238724906372E-15 ) ) ;
#19579 = CARTESIAN_POINT ( 'NONE',  ( 24.00937500061451502, -5.492252693125287522, -1.008910452111647106E-15 ) ) ;
#19580 = CARTESIAN_POINT ( 'NONE',  ( 26.32499999999999929, 4.330127018922191873, 2.499999999999999556 ) ) ;
#19581 = CARTESIAN_POINT ( 'NONE',  ( 25.26562500061451289, 3.027376345333611329, 5.243569643749999010 ) ) ;
#19582 = CARTESIAN_POINT ( 'NONE',  ( -4.243569643749999898, 10.40937500061451892, 30.00000000000000000 ) ) ;
#19583 = DIRECTION ( 'NONE',  ( -1.000000000000000000, -0.000000000000000000, -0.000000000000000000 ) ) ;
#19584 = CARTESIAN_POINT ( 'NONE',  ( 26.55937500061451573, 4.541064518000418104, -2.621784821874998173 ) ) ;
#19585 = CARTESIAN_POINT ( 'NONE',  ( 28.54687500061451644, -3.027376345333614438, 5.243569643749998122 ) ) ;
#19586 = CARTESIAN_POINT ( 'NONE',  ( 4.040625000614517681, 6.054752690667223547, 3.707466751127219781E-16 ) ) ;
#19587 = CARTESIAN_POINT ( 'NONE',  ( 22.73437500061451999, -2.746126346562642428, -4.756430356249999214 ) ) ;
#19588 = CARTESIAN_POINT ( 'NONE',  ( 16.58437500061451786, 6.421520780324663323E-16, -5.243569643749999010 ) ) ;
#19589 = CARTESIAN_POINT ( 'NONE',  ( 8.484375000614518214, 5.492252693125287522, 3.363034840372157021E-16 ) ) ;
#19590 = CARTESIAN_POINT ( 'NONE',  ( 29.43750000122903288, 6.123233995736764310E-16, -4.999999999999998224 ) ) ;
#19591 = CARTESIAN_POINT ( 'NONE',  ( 6.384375000614516793, 4.541064518000418104, 2.621784821874999949 ) ) ;
#19592 = CARTESIAN_POINT ( 'NONE',  ( 15.68437500061451573, 6.421520780324663323E-16, -5.243569643749999010 ) ) ;
#19593 = CARTESIAN_POINT ( 'NONE',  ( 3.397178649298551179, 3.668675132081069545, -3.397178649298551179 ) ) ;
#19594 = CARTESIAN_POINT ( 'NONE',  ( 25.68750000000000000, -2.886751345948125991, -5.000000000000000000 ) ) ;
#19595 = CARTESIAN_POINT ( 'NONE',  ( 27.12187500061451573, 3.027376345333611329, 5.243569643749999010 ) ) ;
#19596 = CARTESIAN_POINT ( 'NONE',  ( 2.655984681222220721E-16, 12.86562499938548321, 25.66244784525396483 ) ) ;
#19597 = CARTESIAN_POINT ( 'NONE',  ( 4.247151432104769420, -2.638504256727666863, 4.531370421416291983 ) ) ;
#19598 = ORIENTED_EDGE ( 'NONE', *, *, #19260, .T. ) ;
#19599 = CARTESIAN_POINT ( 'NONE',  ( 7.875000000000000000, 4.330127018922191873, 2.499999999999999556 ) ) ;
#19600 = CARTESIAN_POINT ( 'NONE',  ( 8.371875000614515727, 5.824947211148865298E-16, -4.756430356249998326 ) ) ;
#19601 = CARTESIAN_POINT ( 'NONE',  ( 22.67812500061451431, -4.541064518000419881, 2.621784821874995952 ) ) ;
#19602 = CARTESIAN_POINT ( 'NONE',  ( 10.83750000000000036, -2.886751345948125991, -5.000000000000000000 ) ) ;
#19603 = CARTESIAN_POINT ( 'NONE',  ( 8.250000001229034652, -2.886751345948125991, -5.000000000000000000 ) ) ;
#19604 = CARTESIAN_POINT ( 'NONE',  ( 6.103125000614515905, -4.541064518000417216, -2.621784821875001281 ) ) ;
#19605 = CARTESIAN_POINT ( 'NONE',  ( 22.64999999999999858, 4.330127018922192761, -2.499999999999997780 ) ) ;
#19606 = CARTESIAN_POINT ( 'NONE',  ( 17.31562500061451715, -6.054752690667223547, -1.112240025338166033E-15 ) ) ;
#19607 = CARTESIAN_POINT ( 'NONE',  ( 14.92500000000000071, 6.123233995736764310E-16, -4.999999999999998224 ) ) ;
#19608 = CARTESIAN_POINT ( 'NONE',  ( 25.61250000122903359, 0.000000000000000000, 4.999999999999998224 ) ) ;
#19609 = CARTESIAN_POINT ( 'NONE',  ( -3.756430356250000990, 20.10312499938548925, 32.16877607737301048 ) ) ;
#19610 = CARTESIAN_POINT ( 'NONE',  ( 5.287500000000000533, -2.886751345948129988, 4.999999999999997335 ) ) ;
#19611 = ORIENTED_EDGE ( 'NONE', *, *, #43245, .T. ) ;
#19612 = CARTESIAN_POINT ( 'NONE',  ( 18.77812500061451573, 6.421520780324663323E-16, -5.243569643749999010 ) ) ;
#19613 = CARTESIAN_POINT ( 'NONE',  ( 26.31562500061451715, -6.054752690667223547, -1.112240025338166033E-15 ) ) ;
#19614 = CARTESIAN_POINT ( 'NONE',  ( 27.90937500061451715, 4.541064518000418104, -2.621784821874998173 ) ) ;
#19615 = CARTESIAN_POINT ( 'NONE',  ( 9.525000000000002132, 6.123233995736764310E-16, -4.999999999999998224 ) ) ;
#19616 = EDGE_CURVE ( 'NONE', #17423, #70720, #31400, .T. ) ;
#19617 = CARTESIAN_POINT ( 'NONE',  ( 10.86562500061451431, 3.027376345333611329, 5.243569643749999010 ) ) ;
#19618 = CARTESIAN_POINT ( 'NONE',  ( 28.67812500061451431, 6.421520780324663323E-16, -5.243569643749999010 ) ) ;
#19619 = CARTESIAN_POINT ( 'NONE',  ( 8.728125000614518569, -4.541064518000419881, 2.621784821874995952 ) ) ;
#19620 = CARTESIAN_POINT ( 'NONE',  ( 30.00000000000000000, 0.000000000000000000, 0.000000000000000000 ) ) ;
#19621 = CARTESIAN_POINT ( 'NONE',  ( 2.121784821874999061, 12.95937500061451786, 26.32496088578401583 ) ) ;
#19622 = CARTESIAN_POINT ( 'NONE',  ( 25.35000000122903074, -2.886751345948125991, -5.000000000000000000 ) ) ;
#19623 = CARTESIAN_POINT ( 'NONE',  ( 19.58437500061451786, -4.119189519843968306, 2.378215178124996054 ) ) ;
#19624 = CARTESIAN_POINT ( 'NONE',  ( 13.56562500061451537, 3.027376345333611329, 5.243569643749999010 ) ) ;
#19625 = CARTESIAN_POINT ( 'NONE',  ( 8.099999999999999645, -4.330127018922190985, -2.500000000000001332 ) ) ;
#19626 = CARTESIAN_POINT ( 'NONE',  ( 9.984375000614518214, 4.541064518000418104, 2.621784821874999949 ) ) ;
#19627 = CARTESIAN_POINT ( 'NONE',  ( 10.05937500061451750, 0.000000000000000000, 5.243569643749999010 ) ) ;
#19628 = CARTESIAN_POINT ( 'NONE',  ( 17.55937500061451573, 4.541064518000418104, -2.621784821874998173 ) ) ;
#19629 = ORIENTED_EDGE ( 'NONE', *, *, #44872, .T. ) ;
#19630 = CARTESIAN_POINT ( 'NONE',  ( 29.10937500061451644, -4.541064518000417216, -2.621784821875001281 ) ) ;
#19631 = CARTESIAN_POINT ( 'NONE',  ( 21.14062500061451289, 6.054752690667223547, 3.707466751127219781E-16 ) ) ;
#19632 = CARTESIAN_POINT ( 'NONE',  ( 15.79687500061451821, 6.054752690667223547, 3.707466751127219781E-16 ) ) ;
#19633 = CARTESIAN_POINT ( 'NONE',  ( 21.14062500061451289, 6.054752690667223547, 3.707466751127219781E-16 ) ) ;
#19634 = CARTESIAN_POINT ( 'NONE',  ( 3.999999999999999112, 14.82500000000000107, 30.00000000000000000 ) ) ;
#19635 = CARTESIAN_POINT ( 'NONE',  ( 27.02812500061451573, 4.541064518000418104, 2.621784821874999949 ) ) ;
#19636 = CARTESIAN_POINT ( 'NONE',  ( 7.200000001229035718, -2.886751345948129988, 4.999999999999997335 ) ) ;
#19637 = ORIENTED_EDGE ( 'NONE', *, *, #32035, .F. ) ;
#19638 = CARTESIAN_POINT ( 'NONE',  ( 3.450000001229036162, 5.773502691896255534, 3.535250795749688894E-16 ) ) ;
#19639 = CARTESIAN_POINT ( 'NONE',  ( -3.999999999999997335, 17.78750000000000142, -27.69059892324149175 ) ) ;
#19640 = CIRCLE ( 'NONE', #63305, 1.499999999999999556 ) ;
#19641 = CARTESIAN_POINT ( 'NONE',  ( 24.00000000122902932, -2.886751345948125991, -5.000000000000000000 ) ) ;
#19642 = CARTESIAN_POINT ( 'NONE',  ( 4.000000000000000000, 20.58124999877096784, 27.69059892324149530 ) ) ;
#19643 = CARTESIAN_POINT ( 'NONE',  ( 7.771875000614516971, 3.027376345333611329, 5.243569643749999010 ) ) ;
#19644 = CARTESIAN_POINT ( 'NONE',  ( 4.898587196589411843E-16, 20.00000000000000000, -26.00000000000000000 ) ) ;
#19645 = CARTESIAN_POINT ( 'NONE',  ( 15.10312500061451502, -4.541064518000417216, -2.621784821875001281 ) ) ;
#19646 = CARTESIAN_POINT ( 'NONE',  ( 9.309375000614517504, -4.541064518000417216, -2.621784821875001281 ) ) ;
#19647 = CARTESIAN_POINT ( 'NONE',  ( 26.77500000122903145, 2.886751345948129099, -4.999999999999998224 ) ) ;
#19648 = CARTESIAN_POINT ( 'NONE',  ( 17.67187500061451999, 3.027376345333611329, 5.243569643749999010 ) ) ;
#19649 = CARTESIAN_POINT ( 'NONE',  ( 4.209375000614516971, 0.000000000000000000, 5.243569643749999010 ) ) ;
#19650 = CARTESIAN_POINT ( 'NONE',  ( 2.000000000000000444, 18.87500000000000000, 26.53589838486224650 ) ) ;
#19651 = CARTESIAN_POINT ( 'NONE',  ( 6.290625000614517681, 6.054752690667223547, 3.707466751127219781E-16 ) ) ;
#19652 = CARTESIAN_POINT ( 'NONE',  ( 16.56562500061451715, 3.027376345333613106, -5.243569643749998122 ) ) ;
#19653 = ORIENTED_EDGE ( 'NONE', *, *, #47041, .F. ) ;
#19654 = CARTESIAN_POINT ( 'NONE',  ( 13.15312500061451750, 0.000000000000000000, 5.243569643749999010 ) ) ;
#19655 = VECTOR ( 'NONE', #12514, 1000.000000000000000 ) ;
#19656 = CARTESIAN_POINT ( 'NONE',  ( 4.912500001229034297, 0.000000000000000000, 4.999999999999998224 ) ) ;
#19657 = CARTESIAN_POINT ( 'NONE',  ( 11.01562500061451821, -6.054752690667223547, -1.112240025338166033E-15 ) ) ;
#19658 = CARTESIAN_POINT ( 'NONE',  ( 21.42187500061451644, -5.492252693125287522, -1.008910452111647106E-15 ) ) ;
#19659 = CARTESIAN_POINT ( 'NONE',  ( 11.17500000000000071, -4.330127018922194537, 2.499999999999995559 ) ) ;
#19660 = CARTESIAN_POINT ( 'NONE',  ( 6.825000001229034829, -5.773502691896255534, -1.060575238724906372E-15 ) ) ;
#19661 = CARTESIAN_POINT ( 'NONE',  ( 19.94999999999999929, 4.330127018922192761, -2.499999999999997780 ) ) ;
#19662 =( BOUNDED_SURFACE ( )  B_SPLINE_SURFACE ( 1, 2, ( 
 ( #52735, #690, #23198, #47197, #13200, #7309, #45752, #63089, #52374, #17648, #40208, #12490, #1780, #24291, #18734, #57546, #41298, #35740, #58259, #7665, #69728, #19097, #9131, #15389, #9498, #8396, #13935, #54563, #25387, #30925, #19835, #48659, #43115, #53466, #53837, #14299, #60451, #20934, #59351, #26120, #58990, #25759, #25015, #36837, #37931, #3232, #2857, #31296, #70460, #71184, #47557, #20557, #31668, #70086, #30569, #47931, #42387, #59723, #53095, #36472, #42749, #64909, #2491, #26488, #49030, #71559, #8762, #65640, #15028, #43485, #48295, #37565, #42021, #60089, #65270, #20195, #70821, #14657, #32027, #37200, #19463, #54201, #66009, #64542, #3598, #3966, #66377, #16482, #5417, #44593, #27590, #27222, #27956, #61920, #4336, #73014, #33476, #39039, #33846, #67484, #66753, #67124, #72285, #9859, #22755, #26861, #55657, #61553, #55298, #21663, #49759, #4692, #61197, #72653, #50488, #50122, #10955, #43852, #11326, #5053, #56025, #44947, #247, #32389, #22398, #71923, #21298, #56390, #39775, #16847, #49392, #39403, #5780, #28311, #50847, #67841, #16123, #22034, #45306, #17213, #60821, #54929, #15753, #38292, #10227, #32761, #44220, #38676, #10592, #33120, #46753, #1328, #17924, #24200, #46388, #23840, #12397, #69643, #18279, #68923, #6139, #40487, #51931, #29397, #40855, #24566, #62291, #63372, #69288, #18651, #41213, #68208, #68565, #35653, #57813, #7223, #34933, #29038, #47111, #45672, #2054, #51210, #51573, #610, #17569, #23117, #12756, #6502, #58173, #35292, #29752, #52289, #1690, #19005, #11687, #63721, #40131, #34203, #13113, #62645, #7578, #56737, #57459, #30113, #28670, #12042, #52648, #34565, #57094, #972, #23482, #46029, #63002, #6865, #53746, #70368, #3513, #25669, #3143, #64820, #48943, #70728, #48206, #58533, #19746, #31205, #8674, #20105, #3879, #41567, #42660, #48572, #71100, #20473, #47469, #47839, #14944, #37108, #59634, #14209, #8311, #26400, #24926, #54479, #30482, #30840, #53011, #70001, #2405, #65185, #58899, #37482, #14575, #9047, #31578, #54117, #71471, #64085, #43026, #19371, #13467, #26033, #41928, #65554, #36015, #36746, #60003, #7945, #64454 ),
 ( #13845, #9413, #31943, #36385, #59266, #53374, #2770, #25293, #42295, #11863, #45491, #28492, #45848, #6320, #4610, #5958, #10143, #20847, #34746, #37843, #66661, #51028, #66289, #32676, #38206, #15668, #72203, #10508, #39952, #38586, #22932, #54841, #789, #16038, #55576, #56916, #12218, #43400, #68022, #9773, #32307, #68383, #51751, #28849, #60364, #34384, #17744, #51387, #62465, #6687, #27140, #61112, #23298, #17395, #71841, #424, #33036, #40303, #62825, #4250, #57278, #29215, #65925, #15305, #26775, #49307, #21212, #43765, #49674, #60734, #55215, #21580, #44134, #46568, #53194, #12581, #8135, #40666, #69112, #63185, #35115, #57638, #63905, #24019, #13662, #69472, #7765, #46935, #1880, #2590, #25109, #41745, #7044, #23661, #24386, #29574, #41392, #1152, #18829, #69827, #52111, #1515, #52835, #47292, #13294, #52472, #30661, #46206, #68746, #18104, #35831, #58722, #18472, #36204, #19192, #58354, #41036, #63551, #7404, #12937, #35473, #57995, #29932, #30302, #2235, #24749, #64273, #9965, #21403, #43960, #31406, #32503, #66114, #53946, #44328, #9240, #14767, #43592, #72385, #20302, #26598, #42856, #14405, #10331, #32865, #55401, #31776, #55037, #4440, #4796, #37311, #26968, #25866, #72026, #49138, #4072, #60193, #59833, #49497, #54314, #21766, #3343, #71666, #9603, #36942, #27329, #65378, #66481, #70931, #15859, #71292, #15133, #60558, #3704, #48769, #26231, #20671, #48406, #21041, #54668, #32135, #38405, #59462, #15493, #43229, #60928, #65749, #38036, #49862, #8870, #37671, #23584, #61655, #67225, #22850, #51671, #72754, #5876, #22139, #66857, #62748, #12141, #34666, #11054, #34300, #56832, #57195, #16586, #6239, #5156, #51306, #28409, #56484, #39501, #39137, #28767, #33582, #1076, #10693, #50945, #62025, #16228, #6610, #44693, #11784, #50229, #710, #50587, #67582, #39873, #56128, #28059, #5521, #73115, #33224, #344, #33941, #11424, #23217, #38781, #45404, #55762, #62385, #27691, #67940, #61299, #22497, #45047, #45770, #68306, #16948, #17313, #17665, #40226, #29138, #57563, #52755, #6966, #7326, #63826, #7685, #1436, #29857, #69030, #53483, #25033, #8412, #2875, #47576 ) ),
 .UNSPECIFIED., .F., .F., .F. ) 
 B_SPLINE_SURFACE_WITH_KNOTS ( ( 2, 2 ),
 ( 3, 2, 2, 2, 2, 2, 2, 2, 2, 2, 2, 2, 2, 2, 2, 2, 2, 2, 2, 2, 2, 2, 2, 2, 2, 2, 2, 2, 2, 2, 2, 2, 2, 2, 2, 2, 2, 2, 2, 2, 2, 2, 2, 2, 2, 2, 2, 2, 2, 2, 2, 2, 2, 2, 2, 2, 2, 2, 2, 2, 2, 2, 2, 2, 2, 2, 2, 2, 2, 2, 2, 2, 2, 2, 2, 2, 2, 2, 2, 2, 2, 2, 2, 2, 2, 2, 2, 2, 2, 2, 2, 2, 2, 2, 2, 2, 2, 2, 2, 2, 2, 2, 2, 2, 2, 2, 2, 2, 2, 2, 2, 2, 2, 2, 2, 2, 2, 2, 2, 2, 2, 2, 2, 2, 2, 2, 2, 2, 2, 2, 2, 2, 2, 2, 3 ),
 ( 0.000000000000000000, 1.000000000000000000 ),
 ( 0.000000000000000000, 0.007246376811594202987, 0.01449275362318840597, 0.02173913043478260809, 0.02898550724637681195, 0.03623188405797101580, 0.04347826086956521618, 0.05072463768115942351, 0.05797101449275362389, 0.06521739130434782428, 0.07246376811594203160, 0.07971014492753622505, 0.08695652173913043237, 0.09420289855072463969, 0.1014492753623188470, 0.1086956521739130405, 0.1159420289855072478, 0.1231884057971014551, 0.1304347826086956486, 0.1376811594202898559, 0.1449275362318840632, 0.1521739130434782705, 0.1594202898550724501, 0.1666666666666666574, 0.1739130434782608647, 0.1811594202898550721, 0.1884057971014492794, 0.1956521739130434867, 0.2028985507246376940, 0.2101449275362318736, 0.2173913043478260809, 0.2246376811594202882, 0.2318840579710144956, 0.2391304347826087029, 0.2463768115942029102, 0.2536231884057971175, 0.2608695652173912971, 0.2681159420289855322, 0.2753623188405797118, 0.2826086956521738913, 0.2898550724637681264, 0.2971014492753623060, 0.3043478260869565410, 0.3115942028985507206, 0.3188405797101449002, 0.3260869565217391353, 0.3333333333333333148, 0.3405797101449275499, 0.3478260869565217295, 0.3550724637681159646, 0.3623188405797101441, 0.3695652173913043237, 0.3768115942028985588, 0.3840579710144927383, 0.3913043478260869734, 0.3985507246376811530, 0.4057971014492753881, 0.4130434782608695676, 0.4202898550724637472, 0.4275362318840579823, 0.4347826086956521618, 0.4420289855072463969, 0.4492753623188405765, 0.4565217391304347561, 0.4637681159420289911, 0.4710144927536231707, 0.4782608695652174058, 0.4855072463768115854, 0.4927536231884058204, 0.5000000000000000000, 0.5072463768115942351, 0.5144927536231883591, 0.5217391304347825942, 0.5289855072463768293, 0.5362318840579710644, 0.5434782608695651884, 0.5507246376811594235, 0.5579710144927536586, 0.5652173913043477826, 0.5724637681159420177, 0.5797101449275362528, 0.5869565217391304879, 0.5942028985507246119, 0.6014492753623188470, 0.6086956521739130821, 0.6159420289855072062, 0.6231884057971014412, 0.6304347826086956763, 0.6376811594202898004, 0.6449275362318840354, 0.6521739130434782705, 0.6594202898550725056, 0.6666666666666666297, 0.6739130434782608647, 0.6811594202898550998, 0.6884057971014492239, 0.6956521739130434590, 0.7028985507246376940, 0.7101449275362319291, 0.7173913043478260532, 0.7246376811594202882, 0.7318840579710145233, 0.7391304347826086474, 0.7463768115942028825, 0.7536231884057971175, 0.7608695652173913526, 0.7681159420289854767, 0.7753623188405797118, 0.7826086956521739468, 0.7898550724637680709, 0.7971014492753623060, 0.8043478260869565410, 0.8115942028985507761, 0.8188405797101449002, 0.8260869565217391353, 0.8333333333333333703, 0.8405797101449274944, 0.8478260869565217295, 0.8550724637681159646, 0.8623188405797101996, 0.8695652173913043237, 0.8768115942028985588, 0.8840579710144927938, 0.8913043478260869179, 0.8985507246376811530, 0.9057971014492753881, 0.9130434782608695121, 0.9202898550724637472, 0.9275362318840579823, 0.9347826086956522174, 0.9420289855072463414, 0.9492753623188405765, 0.9565217391304348116, 0.9637681159420289356, 0.9662083003288912675 ),
 .UNSPECIFIED. ) 
 GEOMETRIC_REPRESENTATION_ITEM ( )  RATIONAL_B_SPLINE_SURFACE ( (
 ( 1.000000000000000000, 0.8660254037844387076, 1.000000000000000000, 0.8660254037844387076, 1.000000000000000000, 0.8660254037844387076, 1.000000000000000000, 0.8660254037844387076, 1.000000000000000000, 0.8660254037844387076, 1.000000000000000000, 0.8660254037844387076, 1.000000000000000000, 0.8660254037844387076, 1.000000000000000000, 0.8660254037844387076, 1.000000000000000000, 0.8660254037844387076, 1.000000000000000000, 0.8660254037844387076, 1.000000000000000000, 0.8660254037844387076, 1.000000000000000000, 0.8660254037844387076, 1.000000000000000000, 0.8660254037844387076, 1.000000000000000000, 0.8660254037844387076, 1.000000000000000000, 0.8660254037844387076, 1.000000000000000000, 0.8660254037844387076, 1.000000000000000000, 0.8660254037844387076, 1.000000000000000000, 0.8660254037844387076, 1.000000000000000000, 0.8660254037844387076, 1.000000000000000000, 0.8660254037844387076, 1.000000000000000000, 0.8660254037844387076, 1.000000000000000000, 0.8660254037844387076, 1.000000000000000000, 0.8660254037844387076, 1.000000000000000000, 0.8660254037844387076, 1.000000000000000000, 0.8660254037844387076, 1.000000000000000000, 0.8660254037844387076, 1.000000000000000000, 0.8660254037844387076, 1.000000000000000000, 0.8660254037844387076, 1.000000000000000000, 0.8660254037844387076, 1.000000000000000000, 0.8660254037844387076, 1.000000000000000000, 0.8660254037844387076, 1.000000000000000000, 0.8660254037844387076, 1.000000000000000000, 0.8660254037844387076, 1.000000000000000000, 0.8660254037844387076, 1.000000000000000000, 0.8660254037844387076, 1.000000000000000000, 0.8660254037844387076, 1.000000000000000000, 0.8660254037844387076, 1.000000000000000000, 0.8660254037844387076, 1.000000000000000000, 0.8660254037844387076, 1.000000000000000000, 0.8660254037844387076, 1.000000000000000000, 0.8660254037844387076, 1.000000000000000000, 0.8660254037844387076, 1.000000000000000000, 0.8660254037844387076, 1.000000000000000000, 0.8660254037844387076, 1.000000000000000000, 0.8660254037844387076, 1.000000000000000000, 0.8660254037844387076, 1.000000000000000000, 0.8660254037844387076, 1.000000000000000000, 0.8660254037844387076, 1.000000000000000000, 0.8660254037844387076, 1.000000000000000000, 0.8660254037844387076, 1.000000000000000000, 0.8660254037844387076, 1.000000000000000000, 0.8660254037844387076, 1.000000000000000000, 0.8660254037844387076, 1.000000000000000000, 0.8660254037844387076, 1.000000000000000000, 0.8660254037844387076, 1.000000000000000000, 0.8660254037844387076, 1.000000000000000000, 0.8660254037844387076, 1.000000000000000000, 0.8660254037844387076, 1.000000000000000000, 0.8660254037844387076, 1.000000000000000000, 0.8660254037844387076, 1.000000000000000000, 0.8660254037844387076, 1.000000000000000000, 0.8660254037844387076, 1.000000000000000000, 0.8660254037844387076, 1.000000000000000000, 0.8660254037844387076, 1.000000000000000000, 0.8660254037844387076, 1.000000000000000000, 0.8660254037844387076, 1.000000000000000000, 0.8660254037844387076, 1.000000000000000000, 0.8660254037844387076, 1.000000000000000000, 0.8660254037844387076, 1.000000000000000000, 0.8660254037844387076, 1.000000000000000000, 0.8660254037844387076, 1.000000000000000000, 0.8660254037844387076, 1.000000000000000000, 0.8660254037844387076, 1.000000000000000000, 0.8660254037844387076, 1.000000000000000000, 0.8660254037844387076, 1.000000000000000000, 0.8660254037844387076, 1.000000000000000000, 0.8660254037844387076, 1.000000000000000000, 0.8660254037844387076, 1.000000000000000000, 0.8660254037844387076, 1.000000000000000000, 0.8660254037844387076, 1.000000000000000000, 0.8660254037844387076, 1.000000000000000000, 0.8660254037844387076, 1.000000000000000000, 0.8660254037844387076, 1.000000000000000000, 0.8660254037844387076, 1.000000000000000000, 0.8660254037844387076, 1.000000000000000000, 0.8660254037844387076, 1.000000000000000000, 0.8660254037844387076, 1.000000000000000000, 0.8660254037844387076, 1.000000000000000000, 0.8660254037844387076, 1.000000000000000000, 0.8660254037844387076, 1.000000000000000000, 0.8660254037844387076, 1.000000000000000000, 0.8660254037844387076, 1.000000000000000000, 0.8660254037844387076, 1.000000000000000000, 0.8660254037844387076, 1.000000000000000000, 0.8660254037844387076, 1.000000000000000000, 0.8660254037844387076, 1.000000000000000000, 0.8660254037844387076, 1.000000000000000000, 0.8660254037844387076, 1.000000000000000000, 0.8660254037844387076, 1.000000000000000000, 0.8660254037844387076, 1.000000000000000000, 0.8660254037844387076, 1.000000000000000000, 0.8660254037844387076, 1.000000000000000000, 0.8660254037844387076, 1.000000000000000000, 0.8660254037844387076, 1.000000000000000000, 0.8660254037844387076, 1.000000000000000000, 0.8660254037844387076, 1.000000000000000000, 0.8660254037844387076, 1.000000000000000000, 0.8660254037844387076, 1.000000000000000000, 0.8660254037844387076, 1.000000000000000000, 0.8660254037844387076, 1.000000000000000000, 0.8660254037844387076, 1.000000000000000000, 0.8660254037844387076, 1.000000000000000000, 0.8660254037844387076, 1.000000000000000000, 0.8660254037844387076, 1.000000000000000000, 0.8660254037844387076, 1.000000000000000000, 0.8660254037844387076, 1.000000000000000000, 0.8660254037844387076, 1.000000000000000000, 0.8660254037844387076, 1.000000000000000000, 0.8660254037844387076, 1.000000000000000000, 0.8660254037844387076, 1.000000000000000000, 0.8660254037844387076, 1.000000000000000000, 0.8660254037844387076, 1.000000000000000000, 0.8660254037844387076, 1.000000000000000000, 0.8660254037844387076, 1.000000000000000000, 0.8660254037844387076, 1.000000000000000000, 0.8660254037844387076, 1.000000000000000000, 0.8660254037844387076, 1.000000000000000000, 0.8660254037844387076, 1.000000000000000000, 0.8660254037844387076, 1.000000000000000000, 0.8660254037844387076, 1.000000000000000000, 0.8660254037844387076, 1.000000000000000000, 0.8660254037844387076, 1.000000000000000000, 0.8660254037844387076, 1.000000000000000000, 0.9548846649268474263, 0.9401540970596797830),
 ( 1.000000000000000000, 0.8660254037844387076, 1.000000000000000000, 0.8660254037844387076, 1.000000000000000000, 0.8660254037844387076, 1.000000000000000000, 0.8660254037844387076, 1.000000000000000000, 0.8660254037844387076, 1.000000000000000000, 0.8660254037844387076, 1.000000000000000000, 0.8660254037844387076, 1.000000000000000000, 0.8660254037844387076, 1.000000000000000000, 0.8660254037844387076, 1.000000000000000000, 0.8660254037844387076, 1.000000000000000000, 0.8660254037844387076, 1.000000000000000000, 0.8660254037844387076, 1.000000000000000000, 0.8660254037844387076, 1.000000000000000000, 0.8660254037844387076, 1.000000000000000000, 0.8660254037844387076, 1.000000000000000000, 0.8660254037844387076, 1.000000000000000000, 0.8660254037844387076, 1.000000000000000000, 0.8660254037844387076, 1.000000000000000000, 0.8660254037844387076, 1.000000000000000000, 0.8660254037844387076, 1.000000000000000000, 0.8660254037844387076, 1.000000000000000000, 0.8660254037844387076, 1.000000000000000000, 0.8660254037844387076, 1.000000000000000000, 0.8660254037844387076, 1.000000000000000000, 0.8660254037844387076, 1.000000000000000000, 0.8660254037844387076, 1.000000000000000000, 0.8660254037844387076, 1.000000000000000000, 0.8660254037844387076, 1.000000000000000000, 0.8660254037844387076, 1.000000000000000000, 0.8660254037844387076, 1.000000000000000000, 0.8660254037844387076, 1.000000000000000000, 0.8660254037844387076, 1.000000000000000000, 0.8660254037844387076, 1.000000000000000000, 0.8660254037844387076, 1.000000000000000000, 0.8660254037844387076, 1.000000000000000000, 0.8660254037844387076, 1.000000000000000000, 0.8660254037844387076, 1.000000000000000000, 0.8660254037844387076, 1.000000000000000000, 0.8660254037844387076, 1.000000000000000000, 0.8660254037844387076, 1.000000000000000000, 0.8660254037844387076, 1.000000000000000000, 0.8660254037844387076, 1.000000000000000000, 0.8660254037844387076, 1.000000000000000000, 0.8660254037844387076, 1.000000000000000000, 0.8660254037844387076, 1.000000000000000000, 0.8660254037844387076, 1.000000000000000000, 0.8660254037844387076, 1.000000000000000000, 0.8660254037844387076, 1.000000000000000000, 0.8660254037844387076, 1.000000000000000000, 0.8660254037844387076, 1.000000000000000000, 0.8660254037844387076, 1.000000000000000000, 0.8660254037844387076, 1.000000000000000000, 0.8660254037844387076, 1.000000000000000000, 0.8660254037844387076, 1.000000000000000000, 0.8660254037844387076, 1.000000000000000000, 0.8660254037844387076, 1.000000000000000000, 0.8660254037844387076, 1.000000000000000000, 0.8660254037844387076, 1.000000000000000000, 0.8660254037844387076, 1.000000000000000000, 0.8660254037844387076, 1.000000000000000000, 0.8660254037844387076, 1.000000000000000000, 0.8660254037844387076, 1.000000000000000000, 0.8660254037844387076, 1.000000000000000000, 0.8660254037844387076, 1.000000000000000000, 0.8660254037844387076, 1.000000000000000000, 0.8660254037844387076, 1.000000000000000000, 0.8660254037844387076, 1.000000000000000000, 0.8660254037844387076, 1.000000000000000000, 0.8660254037844387076, 1.000000000000000000, 0.8660254037844387076, 1.000000000000000000, 0.8660254037844387076, 1.000000000000000000, 0.8660254037844387076, 1.000000000000000000, 0.8660254037844387076, 1.000000000000000000, 0.8660254037844387076, 1.000000000000000000, 0.8660254037844387076, 1.000000000000000000, 0.8660254037844387076, 1.000000000000000000, 0.8660254037844387076, 1.000000000000000000, 0.8660254037844387076, 1.000000000000000000, 0.8660254037844387076, 1.000000000000000000, 0.8660254037844387076, 1.000000000000000000, 0.8660254037844387076, 1.000000000000000000, 0.8660254037844387076, 1.000000000000000000, 0.8660254037844387076, 1.000000000000000000, 0.8660254037844387076, 1.000000000000000000, 0.8660254037844387076, 1.000000000000000000, 0.8660254037844387076, 1.000000000000000000, 0.8660254037844387076, 1.000000000000000000, 0.8660254037844387076, 1.000000000000000000, 0.8660254037844387076, 1.000000000000000000, 0.8660254037844387076, 1.000000000000000000, 0.8660254037844387076, 1.000000000000000000, 0.8660254037844387076, 1.000000000000000000, 0.8660254037844387076, 1.000000000000000000, 0.8660254037844387076, 1.000000000000000000, 0.8660254037844387076, 1.000000000000000000, 0.8660254037844387076, 1.000000000000000000, 0.8660254037844387076, 1.000000000000000000, 0.8660254037844387076, 1.000000000000000000, 0.8660254037844387076, 1.000000000000000000, 0.8660254037844387076, 1.000000000000000000, 0.8660254037844387076, 1.000000000000000000, 0.8660254037844387076, 1.000000000000000000, 0.8660254037844387076, 1.000000000000000000, 0.8660254037844387076, 1.000000000000000000, 0.8660254037844387076, 1.000000000000000000, 0.8660254037844387076, 1.000000000000000000, 0.8660254037844387076, 1.000000000000000000, 0.8660254037844387076, 1.000000000000000000, 0.8660254037844387076, 1.000000000000000000, 0.8660254037844387076, 1.000000000000000000, 0.8660254037844387076, 1.000000000000000000, 0.8660254037844387076, 1.000000000000000000, 0.8660254037844387076, 1.000000000000000000, 0.8660254037844387076, 1.000000000000000000, 0.8660254037844387076, 1.000000000000000000, 0.8660254037844387076, 1.000000000000000000, 0.8660254037844387076, 1.000000000000000000, 0.8660254037844387076, 1.000000000000000000, 0.8660254037844387076, 1.000000000000000000, 0.8660254037844387076, 1.000000000000000000, 0.8660254037844387076, 1.000000000000000000, 0.8660254037844387076, 1.000000000000000000, 0.8660254037844387076, 1.000000000000000000, 0.8660254037844387076, 1.000000000000000000, 0.8660254037844387076, 1.000000000000000000, 0.8660254037844387076, 1.000000000000000000, 0.8660254037844387076, 1.000000000000000000, 0.8660254037844387076, 1.000000000000000000, 0.8660254037844387076, 1.000000000000000000, 0.8660254037844387076, 1.000000000000000000, 0.8660254037844387076, 1.000000000000000000, 0.8660254037844387076, 1.000000000000000000, 0.8660254037844387076, 1.000000000000000000, 0.9548846649268474263, 0.9401540970596797830) ) ) 
 REPRESENTATION_ITEM ( '' )  SURFACE ( )  );
#19663 = CARTESIAN_POINT ( 'NONE',  ( 14.14687500061451786, -3.027376345333614438, 5.243569643749998122 ) ) ;
#19664 = CARTESIAN_POINT ( 'NONE',  ( 17.13750000122903216, -4.330127018922194537, 2.499999999999995559 ) ) ;
#19665 = CARTESIAN_POINT ( 'NONE',  ( 22.72499999999999787, 4.330127018922191873, 2.499999999999999556 ) ) ;
#19666 = CARTESIAN_POINT ( 'NONE',  ( 5.190092854996874117, 9.755146338944483020, -35.22418694837048037 ) ) ;
#19667 = CARTESIAN_POINT ( 'NONE',  ( 9.112499999999998934, 2.886751345948073588, -5.000000000000094147 ) ) ;
#19668 = CARTESIAN_POINT ( 'NONE',  ( 2.000000000000001332, 14.86250000122903536, -26.53589838486224650 ) ) ;
#19669 = CARTESIAN_POINT ( 'NONE',  ( 4.284375000614518925, -4.541064518000419881, 2.621784821874995952 ) ) ;
#19670 = CARTESIAN_POINT ( 'NONE',  ( 45.00000000000000000, 0.000000000000000000, 0.000000000000000000 ) ) ;
#19671 = CARTESIAN_POINT ( 'NONE',  ( 4.714058847239782857, -1.672958453767266818, -4.806836186950011580 ) ) ;
#19672 = CARTESIAN_POINT ( 'NONE',  ( 16.05937500061451573, -4.541064518000417216, -2.621784821875001281 ) ) ;
#19673 = CARTESIAN_POINT ( 'NONE',  ( 28.27499999999999858, -4.330127018922194537, 2.499999999999995559 ) ) ;
#19674 = EDGE_CURVE ( 'NONE', #3427, #13717, #35228, .T. ) ;
#19675 = CARTESIAN_POINT ( 'NONE',  ( 11.24062500061451608, 6.054752690667223547, 3.707466751127219781E-16 ) ) ;
#19676 = CARTESIAN_POINT ( 'NONE',  ( 29.40937500061451360, -5.492252693125287522, -1.008910452111647106E-15 ) ) ;
#19677 = CARTESIAN_POINT ( 'NONE',  ( 23.40937500061451715, 4.541064518000418104, -2.621784821874998173 ) ) ;
#19678 = CARTESIAN_POINT ( 'NONE',  ( 14.93437500061451573, -2.746126346562646425, 4.756430356249996549 ) ) ;
#19679 = CARTESIAN_POINT ( 'NONE',  ( 8.953125000614518214, 4.541064518000418104, -2.621784821874998173 ) ) ;
#19680 = CARTESIAN_POINT ( 'NONE',  ( 15.12187500061451750, -6.054752690667223547, -1.112240025338166033E-15 ) ) ;
#19681 = ORIENTED_EDGE ( 'NONE', *, *, #33045, .T. ) ;
#19682 = CARTESIAN_POINT ( 'NONE',  ( 27.15937500061451360, 0.000000000000000000, 5.243569643749999010 ) ) ;
#19683 = CARTESIAN_POINT ( 'NONE',  ( 27.02812500061451573, 4.541064518000418104, 2.621784821874999949 ) ) ;
#19684 = CARTESIAN_POINT ( 'NONE',  ( 28.67812500061451431, 6.421520780324663323E-16, -5.243569643749999010 ) ) ;
#19685 = DIRECTION ( 'NONE',  ( -1.000000000000000000, -0.000000000000000000, -0.000000000000000000 ) ) ;
#19686 = CARTESIAN_POINT ( 'NONE',  ( 6.412500000000001421, 2.886751345948129099, -4.999999999999998224 ) ) ;
#19687 = VECTOR ( 'NONE', #9430, 1000.000000000000000 ) ;
#19688 = CARTESIAN_POINT ( 'NONE',  ( 18.52500000122903145, -5.773502691896255534, -1.060575238724906372E-15 ) ) ;
#19689 = CARTESIAN_POINT ( 'NONE',  ( 4.898587196589411843E-16, 20.00000000000000000, -26.00000000000000000 ) ) ;
#19690 = CARTESIAN_POINT ( 'NONE',  ( 7.284375000614517148, -2.746126346562646425, 4.756430356249996549 ) ) ;
#19691 = ORIENTED_EDGE ( 'NONE', *, *, #7459, .T. ) ;
#19692 = CARTESIAN_POINT ( 'NONE',  ( 14.58750000000000036, 5.773502691896255534, 3.535250795749688894E-16 ) ) ;
#19693 = CARTESIAN_POINT ( 'NONE',  ( 19.46249999999999858, 2.886751345948129099, -4.999999999999998224 ) ) ;
#19694 = CARTESIAN_POINT ( 'NONE',  ( 14.91562500061451679, 3.027376345333611329, 5.243569643749999010 ) ) ;
#19695 = ORIENTED_EDGE ( 'NONE', *, *, #5795, .T. ) ;
#19696 = CARTESIAN_POINT ( 'NONE',  ( 10.38750000000000107, -2.886751345948126435, -5.000000000000000000 ) ) ;
#19697 = CARTESIAN_POINT ( 'NONE',  ( -4.243569643749999898, 16.67187500061451644, -32.45002607614398471 ) ) ;
#19698 = CARTESIAN_POINT ( 'NONE',  ( 6.290625000614517681, 6.054752690667223547, 3.707466751127219781E-16 ) ) ;
#19699 = CARTESIAN_POINT ( 'NONE',  ( 1.878215178124997609, 13.01562499938548356, 33.25316411605952993 ) ) ;
#19700 = CARTESIAN_POINT ( 'NONE',  ( 11.28749999999999787, -2.886751345948125991, -5.000000000000000000 ) ) ;
#19701 = CARTESIAN_POINT ( 'NONE',  ( 28.80937500061451217, 2.746126346562643317, 4.756430356249998326 ) ) ;
#19702 = ORIENTED_EDGE ( 'NONE', *, *, #65676, .T. ) ;
#19703 = CARTESIAN_POINT ( 'NONE',  ( 4.243569643749999898, 14.62812500061451715, 30.00000000000000000 ) ) ;
#19704 = CARTESIAN_POINT ( 'NONE',  ( 25.64062500061451644, 6.054752690667223547, 3.707466751127219781E-16 ) ) ;
#19705 = CARTESIAN_POINT ( 'NONE',  ( 8.212500000000000355, 2.886751345948129099, -4.999999999999998224 ) ) ;
#19706 = CARTESIAN_POINT ( 'NONE',  ( 1.878215178125000495, 17.21562499938548285, 26.74683588394047007 ) ) ;
#19707 = CARTESIAN_POINT ( 'NONE',  ( 23.89687500061451786, 6.054752690667223547, 3.707466751127219781E-16 ) ) ;
#19708 = ADVANCED_FACE ( 'NONE', ( #53963 ), #23770, .T. ) ;
#19709 = CARTESIAN_POINT ( 'NONE',  ( 20.50312500061451715, -4.541064518000417216, -2.621784821875001281 ) ) ;
#19710 = CARTESIAN_POINT ( 'NONE',  ( 4.243569643749999898, 14.62812500061459353, -30.00000000000000000 ) ) ;
#19711 = CARTESIAN_POINT ( 'NONE',  ( 22.95000000122903216, -2.886751345948129988, 4.999999999999997335 ) ) ;
#19712 = CARTESIAN_POINT ( 'NONE',  ( 6.028125000614517504, -4.541064518000419881, 2.621784821874995952 ) ) ;
#19713 = CARTESIAN_POINT ( 'NONE',  ( 25.58437500061451431, 5.824947211148865298E-16, -4.756430356249998326 ) ) ;
#19714 = CARTESIAN_POINT ( 'NONE',  ( 23.27812500061451573, 6.421520780324663323E-16, -5.243569643749999010 ) ) ;
#19715 = CARTESIAN_POINT ( 'NONE',  ( 11.07187500061451679, -5.492252693125287522, -1.008910452111647106E-15 ) ) ;
#19716 = CARTESIAN_POINT ( 'NONE',  ( 1.878215178124997609, 15.71562499938548108, 33.25316411605952993 ) ) ;
#19717 = CARTESIAN_POINT ( 'NONE',  ( 16.95937500061451786, -4.541064518000417216, -2.621784821875001281 ) ) ;
#19718 = CARTESIAN_POINT ( 'NONE',  ( 25.28437500061451715, 4.541064518000418104, 2.621784821874999949 ) ) ;
#19719 = CARTESIAN_POINT ( 'NONE',  ( -4.243569643749998122, 13.59687500061451892, 32.45002607614398471 ) ) ;
#19720 = CARTESIAN_POINT ( 'NONE',  ( 5.540625000614515905, -3.027376345333614438, 5.243569643749998122 ) ) ;
#19722 =( BOUNDED_CURVE ( )  B_SPLINE_CURVE ( 2, ( #11084, #28088, #50616, #11452, #56512, #28439, #50974 ),
 .UNSPECIFIED., .F., .F. ) 
 B_SPLINE_CURVE_WITH_KNOTS ( ( 3, 2, 2, 3 ),
 ( 0.6100000000000002087, 0.6133333333333333970, 0.6166666666666668073, 0.6199999999999999956 ),
 .UNSPECIFIED. ) 
 CURVE ( )  GEOMETRIC_REPRESENTATION_ITEM ( )  RATIONAL_B_SPLINE_CURVE ( ( 0.9999999999999911182, 0.8660254037844475894, 1.000000000000000000, 0.8660254037844387076, 1.000000000000000000, 0.8660254037844387076, 1.000000000000000000 ) ) 
 REPRESENTATION_ITEM ( '' )  );
#19721 = CARTESIAN_POINT ( 'NONE',  ( 29.39062500061451289, -3.027376345333614438, 5.243569643749998122 ) ) ;
#19723 = CARTESIAN_POINT ( 'NONE',  ( 29.35312500061451502, 0.000000000000000000, 5.243569643749999010 ) ) ;
#19724 = CARTESIAN_POINT ( 'NONE',  ( -1.243387493232115393E-14, 14.86250000000000071, 26.00000000000000000 ) ) ;
#19725 = CARTESIAN_POINT ( 'NONE',  ( 3.293689335155384867, 4.087229415801913568, -2.920710989641019495 ) ) ;
#19726 = CARTESIAN_POINT ( 'NONE',  ( 3.365625000614516082, -6.054752690667223547, -1.112240025338166033E-15 ) ) ;
#19727 = CARTESIAN_POINT ( 'NONE',  ( 8.409375000614518925, -4.541064518000417216, -2.621784821875001281 ) ) ;
#19728 = CARTESIAN_POINT ( 'NONE',  ( 0.000000000000000000, 0.000000000000000000, 0.000000000000000000 ) ) ;
#19729 = CARTESIAN_POINT ( 'NONE',  ( 14.70000000122903394, 5.773502691896255534, 3.535250795749688894E-16 ) ) ;
#19730 = CARTESIAN_POINT ( 'NONE',  ( 4.209375000614516971, 0.000000000000000000, 5.243569643749999010 ) ) ;
#19731 = CARTESIAN_POINT ( 'NONE',  ( 12.41250000122903430, 4.330127018922192761, -2.499999999999997780 ) ) ;
#19732 = CARTESIAN_POINT ( 'NONE',  ( 5.690625000614516260, -3.027376345333610441, -5.243569643749999898 ) ) ;
#19733 = DIRECTION ( 'NONE',  ( 0.000000000000000000, 0.000000000000000000, -1.000000000000000000 ) ) ;
#19734 = CARTESIAN_POINT ( 'NONE',  ( 20.34375000122903288, -2.886751345948125991, -5.000000000000000000 ) ) ;
#19735 = CARTESIAN_POINT ( 'NONE',  ( 13.92187500061451644, 3.027376345333613106, -5.243569643749998122 ) ) ;
#19736 = CARTESIAN_POINT ( 'NONE',  ( 21.50625000122903074, 0.000000000000000000, 4.999999999999998224 ) ) ;
#19737 = ORIENTED_EDGE ( 'NONE', *, *, #8112, .T. ) ;
#19738 = CARTESIAN_POINT ( 'NONE',  ( 22.11562500061451786, 3.027376345333611329, 5.243569643749999010 ) ) ;
#19739 = CARTESIAN_POINT ( 'NONE',  ( 6.628125000614517148, 6.421520780324663323E-16, -5.243569643749999010 ) ) ;
#19740 = EDGE_CURVE ( 'NONE', #24417, #34969, #61180, .T. ) ;
#19741 = CARTESIAN_POINT ( 'NONE',  ( 24.83437500061451431, 4.541064518000418104, 2.621784821874999949 ) ) ;
#19742 = CARTESIAN_POINT ( 'NONE',  ( 6.815625000614517148, 3.027376345333611329, 5.243569643749999010 ) ) ;
#19743 = FACE_OUTER_BOUND ( 'NONE', #58575, .T. ) ;
#19744 = CARTESIAN_POINT ( 'NONE',  ( 7.462500001229035007, 4.330127018922192761, -2.499999999999997780 ) ) ;
#19745 = CARTESIAN_POINT ( 'NONE',  ( 25.22812500061451502, 4.541064518000418104, 2.621784821874999949 ) ) ;
#19746 = CARTESIAN_POINT ( 'NONE',  ( 2.121784821875001281, 11.40312500061451750, -26.32496088578401938 ) ) ;
#19747 = CARTESIAN_POINT ( 'NONE',  ( 9.450000001229033941, -2.886751345948129988, 4.999999999999997335 ) ) ;
#19748 = CARTESIAN_POINT ( 'NONE',  ( 19.94062500061451715, -3.027376345333614438, 5.243569643749998122 ) ) ;
#19749 = CARTESIAN_POINT ( 'NONE',  ( 18.62812500061451715, -4.541064518000419881, 2.621784821874995952 ) ) ;
#19750 = CARTESIAN_POINT ( 'NONE',  ( 27.53437500061451360, 4.119189519843966529, 2.378215178124999607 ) ) ;
#19751 = CARTESIAN_POINT ( 'NONE',  ( 17.66249999999999787, 2.886751345948129099, -4.999999999999998224 ) ) ;
#19752 = CARTESIAN_POINT ( 'NONE',  ( 13.87500000122903465, 2.886751345948126879, 4.999999999999999112 ) ) ;
#19753 = AXIS2_PLACEMENT_3D ( 'NONE', #57716, #7121, #24464 ) ;
#19754 = CARTESIAN_POINT ( 'NONE',  ( 9.965625000614517504, 3.027376345333611329, 5.243569643749999010 ) ) ;
#19755 = CARTESIAN_POINT ( 'NONE',  ( 13.00312500061451537, 4.541064518000418104, -2.621784821874998173 ) ) ;
#19756 = CARTESIAN_POINT ( 'NONE',  ( 23.55000000122903359, -2.886751345948125991, -5.000000000000000000 ) ) ;
#19757 = CARTESIAN_POINT ( 'NONE',  ( 22.92187500061451644, 3.027376345333613106, -5.243569643749998122 ) ) ;
#19758 = CARTESIAN_POINT ( 'NONE',  ( 21.30937500061451573, 0.000000000000000000, 5.243569643749999010 ) ) ;
#19759 = CARTESIAN_POINT ( 'NONE',  ( -1.071796769724502107, 18.48259618943233207, 26.00000000000000711 ) ) ;
#19760 = CARTESIAN_POINT ( 'NONE',  ( 8.287500001229034297, 6.123233995736764310E-16, -4.999999999999998224 ) ) ;
#19761 = CARTESIAN_POINT ( 'NONE',  ( 5.334375000614517859, 6.421520780324663323E-16, -5.243569643749999010 ) ) ;
#19762 = CARTESIAN_POINT ( 'NONE',  ( 23.74687500061451573, -3.027376345333610441, -5.243569643749999898 ) ) ;
#19763 = CARTESIAN_POINT ( 'NONE',  ( 4.775752298065365054, -1.480604602020447969, 4.856962839292451761 ) ) ;
#19764 = CARTESIAN_POINT ( 'NONE',  ( 18.81562500061452070, 3.027376345333613106, -5.243569643749998122 ) ) ;
#19765 = CARTESIAN_POINT ( 'NONE',  ( 24.98437500061451644, -4.541064518000419881, 2.621784821874995952 ) ) ;
#19766 = CARTESIAN_POINT ( 'NONE',  ( 3.756430356249998770, 19.91562499938548925, 32.16877607737301759 ) ) ;
#19767 = CARTESIAN_POINT ( 'NONE',  ( 23.06250000000000000, 2.886751345948129099, -4.999999999999997335 ) ) ;
#19768 = CARTESIAN_POINT ( 'NONE',  ( 3.999999999999999112, 15.72500000000000320, 30.00000000000000000 ) ) ;
#19769 = CARTESIAN_POINT ( 'NONE',  ( 4.621875000614516615, 3.027376345333611329, 5.243569643749999010 ) ) ;
#19770 = CARTESIAN_POINT ( 'NONE',  ( 16.67812500061451786, 4.541064518000418104, 2.621784821874999949 ) ) ;
#19771 = VERTEX_POINT ( 'NONE', #41149 ) ;
#19772 = DIRECTION ( 'NONE',  ( -1.000000000000000000, -0.000000000000000000, -0.000000000000000000 ) ) ;
#19773 = CARTESIAN_POINT ( 'NONE',  ( 24.92812500061451431, -4.541064518000419881, 2.621784821874995952 ) ) ;
#19774 = CARTESIAN_POINT ( 'NONE',  ( 4.000000000000000000, 12.98749999999999893, -27.69059892324149885 ) ) ;
#19775 = CARTESIAN_POINT ( 'NONE',  ( 28.19999999999999929, 0.000000000000000000, 4.999999999999998224 ) ) ;
#19776 = CARTESIAN_POINT ( 'NONE',  ( 3.202568429182105270, 3.863133281671067731, -27.55233077308146505 ) ) ;
#19777 = CARTESIAN_POINT ( 'NONE',  ( 15.26249999999999929, -5.773502691896255534, -1.060575238724906372E-15 ) ) ;
#19778 = CARTESIAN_POINT ( 'NONE',  ( 25.50000000122903288, 5.773502691896255534, 3.535250795749688894E-16 ) ) ;
#19779 = CARTESIAN_POINT ( 'NONE',  ( 20.39062500061451644, -3.027376345333614438, 5.243569643749998122 ) ) ;
#19780 = ORIENTED_EDGE ( 'NONE', *, *, #37028, .T. ) ;
#19781 = CARTESIAN_POINT ( 'NONE',  ( 23.06250000000000355, 2.886751345948129099, -4.999999999999998224 ) ) ;
#19782 = EDGE_CURVE ( 'NONE', #12255, #28753, #66360, .T. ) ;
#19783 = CARTESIAN_POINT ( 'NONE',  ( 23.22187500061451715, -6.054752690667223547, -1.112240025338166033E-15 ) ) ;
#19784 = EDGE_LOOP ( 'NONE', ( #51968, #47410, #67170, #13521 ) ) ;
#19785 = CARTESIAN_POINT ( 'NONE',  ( 25.72499999999999787, 6.123233995736764310E-16, -4.999999999999998224 ) ) ;
#19786 = CARTESIAN_POINT ( 'NONE',  ( 13.52812500061451750, 4.541064518000418104, 2.621784821874999949 ) ) ;
#19787 = CARTESIAN_POINT ( 'NONE',  ( 25.08750000122903145, 4.330127018922191873, 2.499999999999999556 ) ) ;
#19788 = CARTESIAN_POINT ( 'NONE',  ( 16.50937500061451502, 2.746126346562645981, -4.756430356249997438 ) ) ;
#19789 = CARTESIAN_POINT ( 'NONE',  ( 28.19062500061451715, -3.027376345333610441, -5.243569643749999898 ) ) ;
#19790 = CARTESIAN_POINT ( 'NONE',  ( 11.96250000122903501, 4.330127018922192761, -2.499999999999997780 ) ) ;
#19791 = CARTESIAN_POINT ( 'NONE',  ( 19.87500000000000000, 6.123233995736764310E-16, -4.999999999999998224 ) ) ;
#19792 = CARTESIAN_POINT ( 'NONE',  ( 26.73749999999999716, 5.773502691896255534, 3.535250795749688894E-16 ) ) ;
#19793 = CARTESIAN_POINT ( 'NONE',  ( 3.084375000614519191, 6.421520780324663323E-16, -5.243569643749999010 ) ) ;
#19794 = CARTESIAN_POINT ( 'NONE',  ( 6.759375000614516793, 4.541064518000418104, -2.621784821874998173 ) ) ;
#19795 = CARTESIAN_POINT ( 'NONE',  ( 20.14687500061451786, -3.027376345333610441, -5.243569643749999898 ) ) ;
#19796 = VERTEX_POINT ( 'NONE', #1990 ) ;
#19797 = CARTESIAN_POINT ( 'NONE',  ( 27.55312500061451786, 0.000000000000000000, 5.243569643749999010 ) ) ;
#19798 = CARTESIAN_POINT ( 'NONE',  ( 28.95937500061451431, 0.000000000000000000, 5.243569643749999010 ) ) ;
#19799 = CARTESIAN_POINT ( 'NONE',  ( 4.321875000614517681, -6.054752690667223547, -1.112240025338166033E-15 ) ) ;
#19800 = CARTESIAN_POINT ( 'NONE',  ( 15.63749999999999751, -2.886751345948129988, 4.999999999999997335 ) ) ;
#19801 = CARTESIAN_POINT ( 'NONE',  ( 14.35312500061451679, 4.541064518000418104, -2.621784821874998173 ) ) ;
#19802 = CARTESIAN_POINT ( 'NONE',  ( -5.810221930991193690E-16, 14.93750000000000000, -34.00000000000000000 ) ) ;
#19803 = CARTESIAN_POINT ( 'NONE',  ( 30.00000000000000000, 6.123233995736764310E-16, -4.999999999999998224 ) ) ;
#19804 = LINE ( 'NONE', #41992, #52832 ) ;
#19805 = CARTESIAN_POINT ( 'NONE',  ( 17.32500000122903216, 2.886751345948129099, -4.999999999999998224 ) ) ;
#19806 = CARTESIAN_POINT ( 'NONE',  ( 3.815625000614518481, -6.054752690667223547, -1.112240025338166033E-15 ) ) ;
#19807 = CARTESIAN_POINT ( 'NONE',  ( 17.67187500061451644, 2.746126346562643317, 4.756430356249998326 ) ) ;
#19808 = CARTESIAN_POINT ( 'NONE',  ( 7.715625000614515727, 3.027376345333611329, 5.243569643749999010 ) ) ;
#19809 = CARTESIAN_POINT ( 'NONE',  ( 23.55937500061451573, 0.000000000000000000, 5.243569643749999010 ) ) ;
#19810 = CARTESIAN_POINT ( 'NONE',  ( 4.243569643749999898, 18.28437500061451715, 30.00000000000000000 ) ) ;
#19811 = CARTESIAN_POINT ( 'NONE',  ( 24.38437500061451502, 4.541064518000418104, 2.621784821874999949 ) ) ;
#19812 = CARTESIAN_POINT ( 'NONE',  ( 5.700000000000000178, 0.000000000000000000, 4.999999999999998224 ) ) ;
#19813 = CARTESIAN_POINT ( 'NONE',  ( -2.828200636599751609E-16, 10.55000000122903359, 25.38119784648299770 ) ) ;
#19814 = CARTESIAN_POINT ( 'NONE',  ( 11.61562500061451608, 3.027376345333613106, -5.243569643749998122 ) ) ;
#19815 = CARTESIAN_POINT ( 'NONE',  ( 3.487500001229035362, 4.330127018922191873, 2.499999999999999556 ) ) ;
#19816 = B_SPLINE_CURVE_WITH_KNOTS ( 'NONE', 3,
 ( #63605, #1937, #52892, #2289 ),
 .UNSPECIFIED., .F., .F.,
 ( 4, 4 ),
 ( 2.168404344971008868E-19, 0.0005975612829869297133 ),
 .UNSPECIFIED. ) ;
#19817 = CARTESIAN_POINT ( 'NONE',  ( 8.521875000614516082, 3.027376345333613106, -5.243569643749998122 ) ) ;
#19818 = CARTESIAN_POINT ( 'NONE',  ( 3.828346580387561371, -3.216332247866912741, 4.095469943695211335 ) ) ;
#19819 = ORIENTED_EDGE ( 'NONE', *, *, #1067, .F. ) ;
#19820 = CARTESIAN_POINT ( 'NONE',  ( 10.34062500061451750, 6.054752690667223547, 3.707466751127219781E-16 ) ) ;
#19821 = CARTESIAN_POINT ( 'NONE',  ( 13.92187500061451644, 3.027376345333613106, -5.243569643749998122 ) ) ;
#19822 = CARTESIAN_POINT ( 'NONE',  ( 20.54999999999999716, 0.000000000000000000, 4.999999999999998224 ) ) ;
#19823 = CARTESIAN_POINT ( 'NONE',  ( 22.76250000122903216, 4.330127018922192761, -2.499999999999997780 ) ) ;
#19824 = CARTESIAN_POINT ( 'NONE',  ( 11.48437500061451644, -4.541064518000419881, 2.621784821874995952 ) ) ;
#19825 = CARTESIAN_POINT ( 'NONE',  ( 11.16562500061451679, 3.027376345333613106, -5.243569643749998122 ) ) ;
#19826 = CARTESIAN_POINT ( 'NONE',  ( 28.03125000122903288, 6.123233995736764310E-16, -4.999999999999998224 ) ) ;
#19827 = CARTESIAN_POINT ( 'NONE',  ( 21.00937500061451857, -4.541064518000417216, -2.621784821875001281 ) ) ;
#19828 = FACE_OUTER_BOUND ( 'NONE', #519, .T. ) ;
#19829 = LINE ( 'NONE', #58621, #51623 ) ;
#19830 = CARTESIAN_POINT ( 'NONE',  ( -3.999999999999999112, 19.96250000000000213, -32.30940107675850470 ) ) ;
#19831 = CARTESIAN_POINT ( 'NONE',  ( 4.243569643749999898, 15.13437500061451679, -30.00000000000000000 ) ) ;
#19832 = CARTESIAN_POINT ( 'NONE',  ( 16.47187500061452070, -6.054752690667223547, -1.112240025338166033E-15 ) ) ;
#19833 = CARTESIAN_POINT ( 'NONE',  ( 16.61250000122903359, 0.000000000000000000, 4.999999999999998224 ) ) ;
#19834 = CARTESIAN_POINT ( 'NONE',  ( 11.25937500061451679, 4.541064518000418104, -2.621784821874998173 ) ) ;
#19835 = CARTESIAN_POINT ( 'NONE',  ( 4.243569643749999898, 18.67812500061451431, -30.00000000000000000 ) ) ;
#19836 = CARTESIAN_POINT ( 'NONE',  ( 17.88750000122903216, 4.330127018922191873, 2.499999999999999556 ) ) ;
#19837 = CARTESIAN_POINT ( 'NONE',  ( 12.29062500061451857, -3.027376345333614438, 5.243569643749998122 ) ) ;
#19838 = ORIENTED_EDGE ( 'NONE', *, *, #5302, .F. ) ;
#19839 = CARTESIAN_POINT ( 'NONE',  ( 14.92500000000000071, 6.123233995736764310E-16, -4.999999999999998224 ) ) ;
#19840 = CARTESIAN_POINT ( 'NONE',  ( -3.999999999999999112, 17.37500000122903288, -32.30940107675850470 ) ) ;
#19841 = CARTESIAN_POINT ( 'NONE',  ( 10.20937500061451786, -4.541064518000417216, -2.621784821875001281 ) ) ;
#19842 = CARTESIAN_POINT ( 'NONE',  ( 3.995221338070210848, 3.006467913421217553, 4.057536123296732633 ) ) ;
#19843 = EDGE_CURVE ( 'NONE', #64855, #68118, #38962, .T. ) ;
#19844 = CARTESIAN_POINT ( 'NONE',  ( 11.47500000122903252, 2.886751345948129099, -4.999999999999998224 ) ) ;
#19845 = CARTESIAN_POINT ( 'NONE',  ( 22.05000000122903714, -2.886751345948129988, 4.999999999999997335 ) ) ;
#19846 = EDGE_CURVE ( 'NONE', #6778, #47420, #12327, .T. ) ;
#19847 = CARTESIAN_POINT ( 'NONE',  ( 16.82812500061451644, -4.541064518000419881, 2.621784821874995952 ) ) ;
#19848 = CARTESIAN_POINT ( 'NONE',  ( 19.75312500061451360, 4.541064518000418104, -2.621784821874998173 ) ) ;
#19849 = CARTESIAN_POINT ( 'NONE',  ( 26.96250000122903145, 0.000000000000000000, 4.999999999999998224 ) ) ;
#19850 = CARTESIAN_POINT ( 'NONE',  ( 26.28749999999999432, 5.773502691896255534, 3.535250795749688894E-16 ) ) ;
#19851 = DIRECTION ( 'NONE',  ( -1.000000000000000000, -0.000000000000000000, -0.000000000000000000 ) ) ;
#19852 = CARTESIAN_POINT ( 'NONE',  ( 29.25000000000000000, -4.330127018922190985, -2.500000000000001332 ) ) ;
#19853 = CARTESIAN_POINT ( 'NONE',  ( 27.45937500061451786, 4.541064518000418104, -2.621784821874998173 ) ) ;
#19854 = CARTESIAN_POINT ( 'NONE',  ( 11.70000000000000284, -4.330127018922190985, -2.500000000000001332 ) ) ;
#19855 = CARTESIAN_POINT ( 'NONE',  ( 9.001249775931846008E-16, 13.22187500061451715, -25.09994784771203058 ) ) ;
#19856 = CARTESIAN_POINT ( 'NONE',  ( 4.425000001229032698, 2.886751345948126879, 4.999999999999999112 ) ) ;
#19857 = CARTESIAN_POINT ( 'NONE',  ( 3.187500000000002220, -2.886751345948125991, -5.000000000000000000 ) ) ;
#19858 = CARTESIAN_POINT ( 'NONE',  ( 27.37500000000000000, -4.330127018922194537, 2.499999999999995559 ) ) ;
#19859 = CARTESIAN_POINT ( 'NONE',  ( 7.059375000614518392, -4.541064518000417216, -2.621784821875001281 ) ) ;
#19860 = CARTESIAN_POINT ( 'NONE',  ( 27.70312500061451289, -4.541064518000417216, -2.621784821875001281 ) ) ;
#19861 = DIRECTION ( 'NONE',  ( 0.000000000000000000, 0.000000000000000000, -1.000000000000000000 ) ) ;
#19862 = CARTESIAN_POINT ( 'NONE',  ( 5.587500000000003020, 5.773502691896255534, 3.535250795749688401E-16 ) ) ;
#19863 = FACE_OUTER_BOUND ( 'NONE', #57754, .T. ) ;
#19864 = CARTESIAN_POINT ( 'NONE',  ( 6.009375000614519458, 0.000000000000000000, 5.243569643749999010 ) ) ;
#19865 = CARTESIAN_POINT ( 'NONE',  ( 11.25937500061451679, 4.541064518000418104, -2.621784821874998173 ) ) ;
#19866 = CARTESIAN_POINT ( 'NONE',  ( 3.900000000000000799, 0.000000000000000000, 4.999999999999998224 ) ) ;
#19867 = CARTESIAN_POINT ( 'NONE',  ( 2.121784821874999061, 14.25312500061459531, 26.32496088578401583 ) ) ;
#19868 = CARTESIAN_POINT ( 'NONE',  ( 0.2655917726329427575, 25.54316770519903557, 26.00000000000000711 ) ) ;
#19869 = CARTESIAN_POINT ( 'NONE',  ( 6.225000000000001421, -4.330127018922194537, 2.499999999999995559 ) ) ;
#19870 = CARTESIAN_POINT ( 'NONE',  ( 15.19687500061451502, 4.119189519843966529, -2.378215178124998275 ) ) ;
#19871 = CARTESIAN_POINT ( 'NONE',  ( 20.84062500061451573, -3.027376345333614438, 5.243569643749998122 ) ) ;
#19872 = CARTESIAN_POINT ( 'NONE',  ( 10.30312500061451431, 4.541064518000418104, -2.621784821874998173 ) ) ;
#19873 = CARTESIAN_POINT ( 'NONE',  ( 24.57187500061451502, 5.824947211148865298E-16, -4.756430356249998326 ) ) ;
#19874 = CARTESIAN_POINT ( 'NONE',  ( 9.646875000614516082, -3.027376345333614438, 5.243569643749998122 ) ) ;
#19875 = CARTESIAN_POINT ( 'NONE',  ( 27.00000000000000000, -4.330127018922190985, -2.500000000000001332 ) ) ;
#19876 = CARTESIAN_POINT ( 'NONE',  ( 19.72500000122903074, 2.886751345948126879, 4.999999999999999112 ) ) ;
#19877 = CARTESIAN_POINT ( 'NONE',  ( 27.59062500061451573, -3.027376345333614438, 5.243569643749998122 ) ) ;
#19878 = DIRECTION ( 'NONE',  ( 0.000000000000000000, 0.000000000000000000, 1.000000000000000000 ) ) ;
#19879 = CARTESIAN_POINT ( 'NONE',  ( 10.54687500061451644, -3.027376345333614438, 5.243569643749998122 ) ) ;
#19880 = CARTESIAN_POINT ( 'NONE',  ( 13.13437500061451857, 4.541064518000418104, 2.621784821874999949 ) ) ;
#19881 = CARTESIAN_POINT ( 'NONE',  ( 26.33437500061451431, -4.541064518000419881, 2.621784821874995952 ) ) ;
#19882 = CARTESIAN_POINT ( 'NONE',  ( 23.47499999999999787, 6.123233995736764310E-16, -4.999999999999998224 ) ) ;
#19883 = CARTESIAN_POINT ( 'NONE',  ( 11.88749999999999751, 5.773502691896255534, 3.535250795749688894E-16 ) ) ;
#19884 = CARTESIAN_POINT ( 'NONE',  ( 20.07187500061451857, -6.054752690667223547, -1.112240025338166033E-15 ) ) ;
#19885 = CARTESIAN_POINT ( 'NONE',  ( 11.48437500061451644, -4.541064518000419881, 2.621784821874995952 ) ) ;
#19886 = CARTESIAN_POINT ( 'NONE',  ( -1.878215178124999163, 12.79062499938548392, 26.74683588394047007 ) ) ;
#19887 = CARTESIAN_POINT ( 'NONE',  ( 23.06250000000000355, 2.886751345948129099, -4.999999999999998224 ) ) ;
#19888 = CARTESIAN_POINT ( 'NONE',  ( -3.999999999999999556, 14.03750000000000142, 27.69059892324149175 ) ) ;
#19889 = CARTESIAN_POINT ( 'NONE',  ( 4.243569643749999010, 11.57187500061451679, -32.45002607614398471 ) ) ;
#19890 = CARTESIAN_POINT ( 'NONE',  ( 25.54687500061451644, -2.746126346562642428, -4.756430356249999214 ) ) ;
#19891 = CARTESIAN_POINT ( 'NONE',  ( 14.54062500061451679, -3.027376345333614438, 5.243569643749998122 ) ) ;
#19892 = CARTESIAN_POINT ( 'NONE',  ( 3.975000000000002753, -4.330127018922194537, 2.499999999999995559 ) ) ;
#19893 = FILL_AREA_STYLE ('',( #15445 ) ) ;
#19894 = CARTESIAN_POINT ( 'NONE',  ( 1.626862140677534273E-15, 10.21250000000000036, 34.00000000000000000 ) ) ;
#19895 = CARTESIAN_POINT ( 'NONE',  ( 12.93750000000000178, -2.886751345948129988, 4.999999999999997335 ) ) ;
#19896 = CARTESIAN_POINT ( 'NONE',  ( -3.999999999999997335, 18.80000000122903359, 32.30940107675850470 ) ) ;
#19897 = CARTESIAN_POINT ( 'NONE',  ( 10.83750000122903501, -4.330127018922194537, 2.499999999999995559 ) ) ;
#19898 = CARTESIAN_POINT ( 'NONE',  ( 22.24687500061451217, -3.027376345333614438, 5.243569643749998122 ) ) ;
#19899 = CARTESIAN_POINT ( 'NONE',  ( 16.69687500061451502, 6.054752690667223547, 3.707466751127219781E-16 ) ) ;
#19900 = DIRECTION ( 'NONE',  ( -1.000000000000000000, -0.000000000000000000, -0.000000000000000000 ) ) ;
#19901 = ORIENTED_EDGE ( 'NONE', *, *, #10704, .T. ) ;
#19902 = CARTESIAN_POINT ( 'NONE',  ( 20.01562500061451644, -6.054752690667223547, -1.112240025338166033E-15 ) ) ;
#19903 = CARTESIAN_POINT ( 'NONE',  ( 3.703125000614516882, 0.000000000000000000, 5.243569643749999010 ) ) ;
#19904 = CARTESIAN_POINT ( 'NONE',  ( 16.80937500061451573, 0.000000000000000000, 5.243569643749999010 ) ) ;
#19905 = CARTESIAN_POINT ( 'NONE',  ( 29.85937500061451644, 0.000000000000000000, 5.243569643749999010 ) ) ;
#19906 = CARTESIAN_POINT ( 'NONE',  ( 4.753125000614515372, -4.541064518000417216, -2.621784821875001281 ) ) ;
#19907 = CARTESIAN_POINT ( 'NONE',  ( 20.24062500061451431, 6.054752690667223547, 3.707466751127219781E-16 ) ) ;
#19908 = CARTESIAN_POINT ( 'NONE',  ( -3.000416591977282496E-16, 15.64062500061451644, 25.09994784771203058 ) ) ;
#19909 = CARTESIAN_POINT ( 'NONE',  ( 17.51250000122903216, 0.000000000000000000, 4.999999999999998224 ) ) ;
#19910 = CARTESIAN_POINT ( 'NONE',  ( 12.30937500061451573, 0.000000000000000000, 4.756430356249998326 ) ) ;
#19911 = CARTESIAN_POINT ( 'NONE',  ( 7.115625000614516971, 3.027376345333612662, -5.243569643749998122 ) ) ;
#19912 = CARTESIAN_POINT ( 'NONE',  ( 3.046875000614519990, -3.027376345333610441, -5.243569643749999898 ) ) ;
#19913 = CARTESIAN_POINT ( 'NONE',  ( 22.84687500061451715, -3.027376345333610441, -5.243569643749999898 ) ) ;
#19914 = CARTESIAN_POINT ( 'NONE',  ( 14.24062500061451608, -3.027376345333610441, -5.243569643749999898 ) ) ;
#19915 = CARTESIAN_POINT ( 'NONE',  ( 25.50000000122903288, 5.773502691896255534, 3.535250795749688894E-16 ) ) ;
#19916 = CARTESIAN_POINT ( 'NONE',  ( 22.60312500061451857, 0.000000000000000000, 5.243569643749999010 ) ) ;
#19917 = CARTESIAN_POINT ( 'NONE',  ( 19.32187500061451857, 3.027376345333613106, -5.243569643749998122 ) ) ;
#19918 = CARTESIAN_POINT ( 'NONE',  ( 13.79062500061451502, -3.027376345333610441, -5.243569643749999898 ) ) ;
#19919 = CARTESIAN_POINT ( 'NONE',  ( 4.243569643749999898, 15.58437500061451786, 30.00000000000000000 ) ) ;
#19920 = CARTESIAN_POINT ( 'NONE',  ( 20.50312500061451715, -4.541064518000417216, -2.621784821875001281 ) ) ;
#19921 = FACE_OUTER_BOUND ( 'NONE', #28263, .T. ) ;
#19922 = VERTEX_POINT ( 'NONE', #34863 ) ;
#19923 = VERTEX_POINT ( 'NONE', #57390 ) ;
#19924 = CARTESIAN_POINT ( 'NONE',  ( 23.96249999999999858, 2.886751345948129099, -4.999999999999998224 ) ) ;
#19925 = CARTESIAN_POINT ( 'NONE',  ( 4.243569643749999010, 19.67187500061451644, -32.45002607614398471 ) ) ;
#19926 = CARTESIAN_POINT ( 'NONE',  ( 3.881554241669678884, -3.151751365348489653, -4.190642664303462439 ) ) ;
#19927 = CARTESIAN_POINT ( 'NONE',  ( 27.40312500061451573, 4.541064518000418104, -2.621784821874998173 ) ) ;
#19928 = CARTESIAN_POINT ( 'NONE',  ( 8.803125000614517859, -4.541064518000417216, -2.621784821875001281 ) ) ;
#19929 = CARTESIAN_POINT ( 'NONE',  ( 20.40000000122903145, -2.886751345948125991, -5.000000000000000000 ) ) ;
#19930 = CARTESIAN_POINT ( 'NONE',  ( 24.96562500061451573, -6.054752690667223547, -1.112240025338166033E-15 ) ) ;
#19931 = CARTESIAN_POINT ( 'NONE',  ( 26.09999999999999787, -4.330127018922190985, -2.500000000000001332 ) ) ;
#19932 = EDGE_CURVE ( 'NONE', #3917, #20508, #13399, .T. ) ;
#19933 = CARTESIAN_POINT ( 'NONE',  ( 26.69062500061451715, -3.027376345333614438, 5.243569643749998122 ) ) ;
#19934 = CARTESIAN_POINT ( 'NONE',  ( 8.690625000614515372, -3.027376345333614438, 5.243569643749998122 ) ) ;
#19935 = EDGE_LOOP ( 'NONE', ( #56094, #5139, #2307, #13366 ) ) ;
#19936 = CARTESIAN_POINT ( 'NONE',  ( 23.39062500061451289, 6.054752690667223547, 3.707466751127219781E-16 ) ) ;
#19937 = CARTESIAN_POINT ( 'NONE',  ( 4.265625000614517326, -6.054752690667223547, -1.112240025338166033E-15 ) ) ;
#19938 = CARTESIAN_POINT ( 'NONE',  ( 13.20937500061451786, 0.000000000000000000, 4.756430356249998326 ) ) ;
#19939 = CARTESIAN_POINT ( 'NONE',  ( 1.071796769724505438, 13.11740381056766580, 26.00000000000001421 ) ) ;
#19940 = CARTESIAN_POINT ( 'NONE',  ( 13.51875000122903536, -5.773502691896255534, -1.060575238724906372E-15 ) ) ;
#19941 = CARTESIAN_POINT ( 'NONE',  ( 13.83749999999999858, -2.886751345948129988, 4.999999999999997335 ) ) ;
#19942 =( BOUNDED_CURVE ( )  B_SPLINE_CURVE ( 2, ( #38153, #27817, #66605, #44077, #50350, #4556, #22970 ),
 .UNSPECIFIED., .F., .F. ) 
 B_SPLINE_CURVE_WITH_KNOTS ( ( 3, 2, 2, 3 ),
 ( 0.4666666666666667296, 0.4694444444444444975, 0.4722222222222222654, 0.4750000000000000333 ),
 .UNSPECIFIED. ) 
 CURVE ( )  GEOMETRIC_REPRESENTATION_ITEM ( )  RATIONAL_B_SPLINE_CURVE ( ( 0.9999999999999973355, 0.8660254037844413721, 1.000000000000000000, 0.8660254037844387076, 1.000000000000000000, 0.8660254037844360431, 1.000000000000002665 ) ) 
 REPRESENTATION_ITEM ( '' )  );
#19943 = CARTESIAN_POINT ( 'NONE',  ( 11.14687500061451608, -3.027376345333610441, -5.243569643749999898 ) ) ;
#19944 = CARTESIAN_POINT ( 'NONE',  ( 9.525000001229033231, -5.773502691896255534, -1.060575238724906372E-15 ) ) ;
#19945 = CARTESIAN_POINT ( 'NONE',  ( 14.97187500061451892, 3.027376345333611329, 5.243569643749999010 ) ) ;
#19946 = CARTESIAN_POINT ( 'NONE',  ( 15.71250000000000213, -5.773502691896255534, -1.060575238724906372E-15 ) ) ;
#19947 = CARTESIAN_POINT ( 'NONE',  ( 8.784375000614518925, -4.541064518000419881, 2.621784821874995952 ) ) ;
#19948 = CARTESIAN_POINT ( 'NONE',  ( 45.00000000000000000, 0.000000000000000000, 0.000000000000000000 ) ) ;
#19949 = CARTESIAN_POINT ( 'NONE',  ( 20.32499999999999929, 6.123233995736764310E-16, -4.999999999999998224 ) ) ;
#19950 = CARTESIAN_POINT ( 'NONE',  ( 12.49687500061451573, -3.027376345333610441, -5.243569643749999898 ) ) ;
#19951 = CARTESIAN_POINT ( 'NONE',  ( 21.92812500061451431, 6.421520780324663323E-16, -5.243569643749999010 ) ) ;
#19952 = CYLINDRICAL_SURFACE ( 'NONE', #22735, 4.999999999999998224 ) ;
#19953 = CARTESIAN_POINT ( 'NONE',  ( -1.626862140677534273E-15, 20.43124999877096570, 34.00000000000000000 ) ) ;
#19954 = CARTESIAN_POINT ( 'NONE',  ( 25.65937500061451715, 4.541064518000418104, -2.621784821874998173 ) ) ;
#19955 = EDGE_CURVE ( 'NONE', #46020, #69015, #23550, .T. ) ;
#19956 = CARTESIAN_POINT ( 'NONE',  ( 3.290625000614516793, -3.027376345333614438, 5.243569643749998122 ) ) ;
#19957 = CARTESIAN_POINT ( 'NONE',  ( 22.24687500061451573, -4.119189519843965641, -2.378215178125001383 ) ) ;
#19958 = CARTESIAN_POINT ( 'NONE',  ( 16.65937500061452070, 4.541064518000418104, -2.621784821874998173 ) ) ;
#19959 = CARTESIAN_POINT ( 'NONE',  ( 9.571875000614515017, -4.119189519843968306, 2.378215178124996054 ) ) ;
#19960 = CARTESIAN_POINT ( 'NONE',  ( 26.51250000122903216, 0.000000000000000000, 4.999999999999998224 ) ) ;
#19961 = CARTESIAN_POINT ( 'NONE',  ( 6.946875000614517681, -3.027376345333614438, 5.243569643749998122 ) ) ;
#19962 = CARTESIAN_POINT ( 'NONE',  ( 16.58437500061451786, 6.421520780324663323E-16, -5.243569643749999010 ) ) ;
#19963 = CARTESIAN_POINT ( 'NONE',  ( 25.46249999999999858, 2.886751345948126879, 4.999999999999999112 ) ) ;
#19964 = CARTESIAN_POINT ( 'NONE',  ( 26.25937500061451857, 0.000000000000000000, 5.243569643749999010 ) ) ;
#19965 = CARTESIAN_POINT ( 'NONE',  ( 3.756430356250000102, 14.10312499938548392, 30.00000000000000000 ) ) ;
#19966 = CARTESIAN_POINT ( 'NONE',  ( 8.681250001229031454, 6.123233995736764310E-16, -4.999999999999998224 ) ) ;
#19967 = CARTESIAN_POINT ( 'NONE',  ( 8.550000000000002487, -4.330127018922190985, -2.500000000000001332 ) ) ;
#19968 = CARTESIAN_POINT ( 'NONE',  ( 9.684375000614517504, -2.746126346562642428, -4.756430356249999214 ) ) ;
#19969 = CARTESIAN_POINT ( 'NONE',  ( 22.04062500061451502, 6.054752690667223547, 3.707466751127219781E-16 ) ) ;
#19970 = CARTESIAN_POINT ( 'NONE',  ( 11.77500000000000036, 6.123233995736764310E-16, -4.999999999999998224 ) ) ;
#19971 = CARTESIAN_POINT ( 'NONE',  ( 5.803125000614517859, 4.541064518000418104, -2.621784821874998173 ) ) ;
#19972 = CARTESIAN_POINT ( 'NONE',  ( 20.66250000000000142, -5.773502691896255534, -1.060575238724906372E-15 ) ) ;
#19973 = CARTESIAN_POINT ( 'NONE',  ( 18.70312500061451644, -4.541064518000417216, -2.621784821875001281 ) ) ;
#19974 = CARTESIAN_POINT ( 'NONE',  ( 23.66249999999999787, 2.886751345948143754, 4.999999999999969802 ) ) ;
#19975 = CARTESIAN_POINT ( 'NONE',  ( 23.77500000122903145, 2.886751345948126879, 4.999999999999999112 ) ) ;
#19976 = CARTESIAN_POINT ( 'NONE',  ( 1.878215178124997609, 20.21562499938548285, 33.25316411605952993 ) ) ;
#19977 = CARTESIAN_POINT ( 'NONE',  ( 6.037500000000001421, 5.773502691896255534, 3.535250795749688894E-16 ) ) ;
#19978 = ORIENTED_EDGE ( 'NONE', *, *, #27431, .T. ) ;
#19979 = CARTESIAN_POINT ( 'NONE',  ( 19.19062500061452070, -3.027376345333610441, -5.243569643749999898 ) ) ;
#19980 = CARTESIAN_POINT ( 'NONE',  ( 25.97812500061451502, 6.421520780324663323E-16, -5.243569643749999010 ) ) ;
#19981 = CARTESIAN_POINT ( 'NONE',  ( 25.50937500061451502, -4.541064518000417216, -2.621784821875001281 ) ) ;
#19982 = CARTESIAN_POINT ( 'NONE',  ( 9.299999999999998934, 0.000000000000000000, 4.999999999999998224 ) ) ;
#19983 = CARTESIAN_POINT ( 'NONE',  ( 11.54062500061451857, -3.027376345333610441, -5.243569643749999898 ) ) ;
#19984 = CARTESIAN_POINT ( 'NONE',  ( 26.72812500061451502, -4.541064518000419881, 2.621784821874995952 ) ) ;
#19985 = CARTESIAN_POINT ( 'NONE',  ( 16.02187500061451786, -6.054752690667223547, -1.112240025338166033E-15 ) ) ;
#19986 = CARTESIAN_POINT ( 'NONE',  ( 9.178125000614517859, -4.541064518000419881, 2.621784821874995952 ) ) ;
#19987 = CARTESIAN_POINT ( 'NONE',  ( 3.999999999999998668, 14.65624999877096890, 32.30940107675850470 ) ) ;
#19988 = CARTESIAN_POINT ( 'NONE',  ( 9.001249775931846008E-16, 11.42187500061451999, 34.90005215228797653 ) ) ;
#19989 = CARTESIAN_POINT ( 'NONE',  ( 24.22500000122903430, 2.886751345948126879, 4.999999999999999112 ) ) ;
#19990 = CARTESIAN_POINT ( 'NONE',  ( 20.40937500061451715, 0.000000000000000000, 4.756430356249998326 ) ) ;
#19991 = CARTESIAN_POINT ( 'NONE',  ( 13.22812500061451502, -4.541064518000419881, 2.621784821874995952 ) ) ;
#19992 = CARTESIAN_POINT ( 'NONE',  ( 10.32187500061451679, 3.027376345333613106, -5.243569643749998122 ) ) ;
#19993 = CARTESIAN_POINT ( 'NONE',  ( 10.13437500061451679, -4.541064518000419881, 2.621784821874995952 ) ) ;
#19994 = VERTEX_POINT ( 'NONE', #26248 ) ;
#19995 = CARTESIAN_POINT ( 'NONE',  ( 1.626862140677534273E-15, 13.36250000000000071, 34.00000000000000000 ) ) ;
#19996 = CARTESIAN_POINT ( 'NONE',  ( 22.71562500061451573, -6.054752690667223547, -1.112240025338166033E-15 ) ) ;
#19997 = CARTESIAN_POINT ( 'NONE',  ( 17.18437500061451573, 4.541064518000418104, 2.621784821874999949 ) ) ;
#19998 = CARTESIAN_POINT ( 'NONE',  ( 22.34062500061451573, -3.027376345333610441, -5.243569643749999898 ) ) ;
#19999 = CARTESIAN_POINT ( 'NONE',  ( -2.828200636599751609E-16, 12.23750000000000249, 25.38119784648299770 ) ) ;
#20000 = CARTESIAN_POINT ( 'NONE',  ( 26.46562500061451573, 3.027376345333613106, -5.243569643749998122 ) ) ;
#20001 = CARTESIAN_POINT ( 'NONE',  ( 6.262500001229034829, 0.000000000000000000, 4.999999999999998224 ) ) ;
#20002 = ORIENTED_EDGE ( 'NONE', *, *, #12677, .F. ) ;
#20003 = CARTESIAN_POINT ( 'NONE',  ( 29.92500000000000071, 4.330127018922191873, 2.499999999999999556 ) ) ;
#20004 = CARTESIAN_POINT ( 'NONE',  ( 4.000000000000000000, 17.48750000000000071, -27.69059892324149530 ) ) ;
#20005 = CARTESIAN_POINT ( 'NONE',  ( 23.58750000122903145, 6.123233995736764310E-16, -4.999999999999998224 ) ) ;
#20006 = CARTESIAN_POINT ( 'NONE',  ( -1.878215178125001827, 14.40312499938548463, 33.25316411605952283 ) ) ;
#20007 = CARTESIAN_POINT ( 'NONE',  ( 7.509375000614517681, -4.541064518000417216, -2.621784821875001281 ) ) ;
#20008 = CARTESIAN_POINT ( 'NONE',  ( -1.487416814333745711E-14, 15.16250000000000142, 34.00000000000000000 ) ) ;
#20009 = CARTESIAN_POINT ( 'NONE',  ( 14.46562500061451750, 3.027376345333611329, 5.243569643749999010 ) ) ;
#20010 = CARTESIAN_POINT ( 'NONE',  ( 7.959375000614516971, -4.541064518000417216, -2.621784821875001281 ) ) ;
#20011 = CARTESIAN_POINT ( 'NONE',  ( 26.06250000122903288, 0.000000000000000000, 4.999999999999998224 ) ) ;
#20012 = CARTESIAN_POINT ( 'NONE',  ( 16.28437500061452070, 4.541064518000418104, 2.621784821874999949 ) ) ;
#20013 = CARTESIAN_POINT ( 'NONE',  ( 4.809375000614516615, -4.541064518000417216, -2.621784821875001281 ) ) ;
#20014 = CARTESIAN_POINT ( 'NONE',  ( 30.00000000000000000, 6.123233995736764310E-16, -4.999999999999998224 ) ) ;
#20015 = CARTESIAN_POINT ( 'NONE',  ( 4.603125000614518569, 0.000000000000000000, 5.243569643749999010 ) ) ;
#20016 = CARTESIAN_POINT ( 'NONE',  ( 14.76562500061451821, 3.027376345333613106, -5.243569643749998122 ) ) ;
#20017 = ORIENTED_EDGE ( 'NONE', *, *, #42731, .T. ) ;
#20018 = CARTESIAN_POINT ( 'NONE',  ( 13.56562500061451892, 3.027376345333611329, 5.243569643749999010 ) ) ;
#20019 = CARTESIAN_POINT ( 'NONE',  ( 5.437500001229035540, -4.330127018922194537, 2.499999999999995559 ) ) ;
#20020 = CARTESIAN_POINT ( 'NONE',  ( 9.665625000614515017, -6.054752690667223547, -1.112240025338166033E-15 ) ) ;
#20021 = CARTESIAN_POINT ( 'NONE',  ( 21.68437500061451573, 4.119189519843966529, 2.378215178124999607 ) ) ;
#20022 = CARTESIAN_POINT ( 'NONE',  ( 9.899999999999998579, -4.330127018922190985, -2.500000000000001332 ) ) ;
#20023 = CARTESIAN_POINT ( 'NONE',  ( 5.250000001229035540, 5.773502691896255534, 3.535250795749688894E-16 ) ) ;
#20024 = CARTESIAN_POINT ( 'NONE',  ( 20.54999999999999716, 0.000000000000000000, 4.999999999999998224 ) ) ;
#20025 = CARTESIAN_POINT ( 'NONE',  ( 16.02187500061451786, -6.054752690667223547, -1.112240025338166033E-15 ) ) ;
#20026 = CARTESIAN_POINT ( 'NONE',  ( 15.22500000122903252, 2.886751345948126879, 4.999999999999999112 ) ) ;
#20027 = CARTESIAN_POINT ( 'NONE',  ( 21.48750000000000071, -2.886751345948129988, 4.999999999999997335 ) ) ;
#20028 = CARTESIAN_POINT ( 'NONE',  ( 2.121784821874999061, 19.20312500061451644, -33.67503911421598417 ) ) ;
#20029 = CARTESIAN_POINT ( 'NONE',  ( 3.999999999999998668, 20.11249999999999716, 32.30940107675850470 ) ) ;
#20030 = CARTESIAN_POINT ( 'NONE',  ( 45.00000000000000000, 6.123233995736764310E-16, -4.999999999999998224 ) ) ;
#20031 = CARTESIAN_POINT ( 'NONE',  ( 28.34062500061451928, 6.054752690667223547, 3.707466751127219781E-16 ) ) ;
#20032 = DIRECTION ( 'NONE',  ( 0.000000000000000000, 0.000000000000000000, 1.000000000000000000 ) ) ;
#20033 = CARTESIAN_POINT ( 'NONE',  ( 3.930102994493983370, -3.091035892528488649, -4.235648827855108323 ) ) ;
#20034 = CARTESIAN_POINT ( 'NONE',  ( 15.19687500061451857, -3.027376345333610441, -5.243569643749999898 ) ) ;
#20035 =( REPRESENTATION_RELATIONSHIP ('NONE','NONE', #33485, #13196 ) REPRESENTATION_RELATIONSHIP_WITH_TRANSFORMATION ( #44117 )SHAPE_REPRESENTATION_RELATIONSHIP( ) );
#20036 = CARTESIAN_POINT ( 'NONE',  ( 29.06250000000000000, 2.886751345948126879, 4.999999999999999112 ) ) ;
#20037 = EDGE_CURVE ( 'NONE', #66542, #24963, #25781, .T. ) ;
#20038 = CARTESIAN_POINT ( 'NONE',  ( 11.54062500061451857, -3.027376345333610441, -5.243569643749999898 ) ) ;
#20039 = CARTESIAN_POINT ( 'NONE',  ( 29.25937500061451857, 2.746126346562643317, 4.756430356249998326 ) ) ;
#20040 = CARTESIAN_POINT ( 'NONE',  ( 24.45937500061451786, 0.000000000000000000, 5.243569643749999010 ) ) ;
#20041 = CARTESIAN_POINT ( 'NONE',  ( 16.69687500061451502, 0.000000000000000000, 4.756430356249998326 ) ) ;
#20042 = CARTESIAN_POINT ( 'NONE',  ( 8.878125000614515372, 6.421520780324663323E-16, -5.243569643749999010 ) ) ;
#20043 = CARTESIAN_POINT ( 'NONE',  ( 12.90937500061451537, -4.541064518000417216, -2.621784821875001281 ) ) ;
#20044 = EDGE_LOOP ( 'NONE', ( #26348, #9822, #40193, #36051 ) ) ;
#20045 = CARTESIAN_POINT ( 'NONE',  ( 23.44687500061451502, 6.054752690667223547, 3.707466751127219781E-16 ) ) ;
#20046 = CARTESIAN_POINT ( 'NONE',  ( 27.55312500061451786, 0.000000000000000000, 5.243569643749999010 ) ) ;
#20047 = CARTESIAN_POINT ( 'NONE',  ( 17.15625000122903288, -4.330127018922190985, -2.500000000000001332 ) ) ;
#20048 = CARTESIAN_POINT ( 'NONE',  ( 7.762500000000001954, 2.886751345948129099, -4.999999999999998224 ) ) ;
#20049 = CARTESIAN_POINT ( 'NONE',  ( 16.23750000122903359, -4.330127018922194537, 2.499999999999995559 ) ) ;
#20050 = CARTESIAN_POINT ( 'NONE',  ( 16.70625000122903359, -4.330127018922190985, -2.500000000000001332 ) ) ;
#20051 = CARTESIAN_POINT ( 'NONE',  ( 8.371875000614515727, 5.824947211148865298E-16, -4.756430356249998326 ) ) ;
#20052 = ORIENTED_EDGE ( 'NONE', *, *, #57093, .T. ) ;
#20053 = CARTESIAN_POINT ( 'NONE',  ( 14.17500000000000071, 4.330127018922191873, 2.499999999999999556 ) ) ;
#20054 = CARTESIAN_POINT ( 'NONE',  ( 18.59999999999999787, 4.330127018922192761, -2.499999999999997780 ) ) ;
#20055 = CARTESIAN_POINT ( 'NONE',  ( 12.62812500061451537, 4.541064518000418104, 2.621784821874999949 ) ) ;
#20056 = ORIENTED_EDGE ( 'NONE', *, *, #34930, .F. ) ;
#20057 = CARTESIAN_POINT ( 'NONE',  ( 16.94999999999999929, 0.000000000000000000, 4.999999999999998224 ) ) ;
#20058 = CARTESIAN_POINT ( 'NONE',  ( -4.243569643749999898, 17.12187500061451573, -32.45002607614398471 ) ) ;
#20059 = CARTESIAN_POINT ( 'NONE',  ( 29.47500000122903430, 2.886751345948129099, -4.999999999999998224 ) ) ;
#20060 = CARTESIAN_POINT ( 'NONE',  ( 19.93125000122903145, 6.123233995736764310E-16, -4.999999999999998224 ) ) ;
#20061 = CARTESIAN_POINT ( 'NONE',  ( 11.55000000000000071, 0.000000000000000000, 4.999999999999998224 ) ) ;
#20062 = CARTESIAN_POINT ( 'NONE',  ( 29.03437500061451360, -2.746126346562642428, -4.756430356249999214 ) ) ;
#20063 = ORIENTED_EDGE ( 'NONE', *, *, #55458, .F. ) ;
#20064 = CARTESIAN_POINT ( 'NONE',  ( -4.243569643749999898, 15.30312500061451608, 30.00000000000000000 ) ) ;
#20065 = CARTESIAN_POINT ( 'NONE',  ( 27.59062500061451573, -3.027376345333614438, 5.243569643749998122 ) ) ;
#20066 = CARTESIAN_POINT ( 'NONE',  ( 0.000000000000000000, 0.000000000000000000, 50.00000000000000000 ) ) ;
#20067 = CARTESIAN_POINT ( 'NONE',  ( -0.6941602726958887581, 20.61426555956768780, 33.93677853444431491 ) ) ;
#20068 = CARTESIAN_POINT ( 'NONE',  ( 23.59687500061451715, -3.027376345333614438, 5.243569643749998122 ) ) ;
#20069 = CARTESIAN_POINT ( 'NONE',  ( 19.67812500061451786, 6.421520780324663323E-16, -5.243569643749999010 ) ) ;
#20070 = CARTESIAN_POINT ( 'NONE',  ( 4.243569643749999898, 13.24062500061459424, -27.54997392385601529 ) ) ;
#20071 = CARTESIAN_POINT ( 'NONE',  ( 23.21250000122903501, 4.330127018922192761, -2.499999999999997780 ) ) ;
#20072 = CARTESIAN_POINT ( 'NONE',  ( 2.953125000614516438, -4.541064518000417216, -2.621784821875001281 ) ) ;
#20073 = CARTESIAN_POINT ( 'NONE',  ( 27.79687500061451644, -2.746126346562641984, -4.756430356249999214 ) ) ;
#20074 = CARTESIAN_POINT ( 'NONE',  ( 20.42812500061451431, -4.541064518000419881, 2.621784821874995952 ) ) ;
#20075 = CARTESIAN_POINT ( 'NONE',  ( 11.29687500061451644, 5.492252693125287522, 3.363034840372157021E-16 ) ) ;
#20076 = CARTESIAN_POINT ( 'NONE',  ( 3.756430356249998770, 16.65312499938548285, 32.16877607737302469 ) ) ;
#20077 = CARTESIAN_POINT ( 'NONE',  ( 17.97187500061451715, 3.027376345333613106, -5.243569643749998122 ) ) ;
#20078 = CARTESIAN_POINT ( 'NONE',  ( 17.25937500061451502, 0.000000000000000000, 5.243569643749999010 ) ) ;
#20079 = CARTESIAN_POINT ( 'NONE',  ( 25.58437500061451431, 6.421520780324663323E-16, -5.243569643749999010 ) ) ;
#20080 = CARTESIAN_POINT ( 'NONE',  ( 2.121784821875001281, 15.05937500061451928, 33.67503911421598417 ) ) ;
#20081 = CARTESIAN_POINT ( 'NONE',  ( 3.965625000614515727, 3.027376345333613106, -5.243569643749998122 ) ) ;
#20082 = CARTESIAN_POINT ( 'NONE',  ( 16.53750000122903430, 4.330127018922191873, 2.499999999999999556 ) ) ;
#20083 = CARTESIAN_POINT ( 'NONE',  ( 28.79062500061451502, 6.054752690667223547, 3.707466751127219781E-16 ) ) ;
#20084 = CARTESIAN_POINT ( 'NONE',  ( -2.000000000000000000, 19.02499999999999858, 26.53589838486224650 ) ) ;
#20085 = CARTESIAN_POINT ( 'NONE',  ( 3.815625000614518036, -6.054752690667223547, -1.112240025338166033E-15 ) ) ;
#20086 = CARTESIAN_POINT ( 'NONE',  ( 6.309375000614517504, 4.541064518000418104, -2.621784821874998173 ) ) ;
#20087 = PRODUCT_CONTEXT ( 'NONE', #43151, 'mechanical' ) ;
#20088 = CARTESIAN_POINT ( 'NONE',  ( 13.53750000122903430, -4.330127018922194537, 2.499999999999995559 ) ) ;
#20089 = CARTESIAN_POINT ( 'NONE',  ( 12.52500000122903145, 2.886751345948126879, 4.999999999999999112 ) ) ;
#20090 = CARTESIAN_POINT ( 'NONE',  ( 5.803125000614517859, 4.541064518000418104, -2.621784821874998173 ) ) ;
#20091 = CARTESIAN_POINT ( 'NONE',  ( 1.999999999999997335, 15.96874999877096535, 33.46410161513775705 ) ) ;
#20092 = CARTESIAN_POINT ( 'NONE',  ( 20.26875000122903003, -5.773502691896255534, -1.060575238724906372E-15 ) ) ;
#20093 = CARTESIAN_POINT ( 'NONE',  ( 14.10937500061451644, 0.000000000000000000, 5.243569643749999010 ) ) ;
#20094 = DIRECTION ( 'NONE',  ( -0.000000000000000000, -0.000000000000000000, -1.000000000000000000 ) ) ;
#20095 = ORIENTED_EDGE ( 'NONE', *, *, #51501, .F. ) ;
#20096 = CARTESIAN_POINT ( 'NONE',  ( 23.12812500061451360, -4.541064518000419881, 2.621784821874995952 ) ) ;
#20097 = CARTESIAN_POINT ( 'NONE',  ( 8.315625000614515372, -6.054752690667223547, -1.112240025338166033E-15 ) ) ;
#20098 = CARTESIAN_POINT ( 'NONE',  ( 23.44687500061451502, 6.054752690667223547, 3.707466751127219781E-16 ) ) ;
#20099 = CARTESIAN_POINT ( 'NONE',  ( 6.778125000614518392, 4.541064518000418104, 2.621784821874999949 ) ) ;
#20100 = LINE ( 'NONE', #13463, #9706 ) ;
#20101 =( BOUNDED_CURVE ( )  B_SPLINE_CURVE ( 2, ( #69216, #63290, #2332, #18574, #41141, #51852, #30036, #52575, #18932 ),
 .UNSPECIFIED., .F., .F. ) 
 B_SPLINE_CURVE_WITH_KNOTS ( ( 3, 2, 2, 2, 3 ),
 ( 0.06944444444444444753, 0.07407407407407406996, 0.08333333333333332871, 0.09259259259259258745, 0.09722222222222222376 ),
 .UNSPECIFIED. ) 
 CURVE ( )  GEOMETRIC_REPRESENTATION_ITEM ( )  RATIONAL_B_SPLINE_CURVE ( ( 0.9330127018922192983, 0.9330127018922194093, 1.000000000000000000, 0.8660254037844387076, 1.000000000000000000, 0.8660254037844387076, 1.000000000000000000, 0.9330127018922191873, 0.9330127018922192983 ) ) 
 REPRESENTATION_ITEM ( '' )  );
#20102 = CARTESIAN_POINT ( 'NONE',  ( 8.962500001229033231, 0.000000000000000000, 4.999999999999998224 ) ) ;
#20103 = EDGE_CURVE ( 'NONE', #67424, #41970, #31791, .T. ) ;
#20104 = CARTESIAN_POINT ( 'NONE',  ( 23.61562500061451431, -6.054752690667223547, -1.112240025338166033E-15 ) ) ;
#20105 = CARTESIAN_POINT ( 'NONE',  ( -4.243569643749997233, 11.29062500061451857, -27.54997392385601174 ) ) ;
#20106 = CARTESIAN_POINT ( 'NONE',  ( 11.28750000122903252, -4.330127018922194537, 2.499999999999995559 ) ) ;
#20107 = CARTESIAN_POINT ( 'NONE',  ( 19.75312500061451360, 4.541064518000418104, -2.621784821874998173 ) ) ;
#20108 = EDGE_CURVE ( 'NONE', #52020, #36659, #36130, .T. ) ;
#20109 = CARTESIAN_POINT ( 'NONE',  ( 17.16562500061451502, 3.027376345333611329, 5.243569643749999010 ) ) ;
#20110 = CARTESIAN_POINT ( 'NONE',  ( 27.34687500061451360, -2.746126346562642428, -4.756430356249999214 ) ) ;
#20111 = CARTESIAN_POINT ( 'NONE',  ( 17.13749999999999929, -2.886751345948125991, -5.000000000000000000 ) ) ;
#20112 = CARTESIAN_POINT ( 'NONE',  ( 13.08750000122903323, -4.330127018922194537, 2.499999999999995559 ) ) ;
#20113 = CARTESIAN_POINT ( 'NONE',  ( 9.253125000614517148, -4.541064518000417216, -2.621784821875001281 ) ) ;
#20114 = CARTESIAN_POINT ( 'NONE',  ( 14.01562500061451644, 3.027376345333611329, 5.243569643749999010 ) ) ;
#20115 = ADVANCED_FACE ( 'NONE', ( #32879 ), #44347, .T. ) ;
#20116 = CARTESIAN_POINT ( 'NONE',  ( 23.66250000122903430, 4.330127018922192761, -2.499999999999997780 ) ) ;
#20117 = CARTESIAN_POINT ( 'NONE',  ( 21.15937500061451715, 4.541064518000418104, -2.621784821874998173 ) ) ;
#20118 = CARTESIAN_POINT ( 'NONE',  ( 20.40937500061451715, 0.000000000000000000, 5.243569643749999010 ) ) ;
#20119 = CARTESIAN_POINT ( 'NONE',  ( 7.518750001229031810, 2.886751345948126879, 4.999999999999998224 ) ) ;
#20120 = EDGE_CURVE ( 'NONE', #10990, #41820, #51239, .T. ) ;
#20121 = CARTESIAN_POINT ( 'NONE',  ( 7.800000001229035362, -2.886751345948125991, -5.000000000000000000 ) ) ;
#20122 = CARTESIAN_POINT ( 'NONE',  ( 7.096875000614517148, -3.027376345333610441, -5.243569643749999898 ) ) ;
#20123 = CARTESIAN_POINT ( 'NONE',  ( 24.34687500061451715, 6.054752690667223547, 3.707466751127219781E-16 ) ) ;
#20124 = CARTESIAN_POINT ( 'NONE',  ( 17.99062500061451786, 6.054752690667223547, 3.707466751127219781E-16 ) ) ;
#20125 = CARTESIAN_POINT ( 'NONE',  ( 23.89687500061451786, 6.054752690667223547, 3.707466751127219781E-16 ) ) ;
#20126 = CARTESIAN_POINT ( 'NONE',  ( -1.878215178125001827, 18.45312499938548356, 33.25316411605952283 ) ) ;
#20127 = CARTESIAN_POINT ( 'NONE',  ( 3.468957575989525477, -4.154263691098152300, -3.291743506479378301 ) ) ;
#20128 = DIRECTION ( 'NONE',  ( 0.000000000000000000, 0.000000000000000000, -1.000000000000000000 ) ) ;
#20129 = CARTESIAN_POINT ( 'NONE',  ( 4.509375000614518569, 4.541064518000418104, -2.621784821874998173 ) ) ;
#20130 = CARTESIAN_POINT ( 'NONE',  ( 16.30312500061451786, 0.000000000000000000, 5.243569643749999010 ) ) ;
#20131 = CARTESIAN_POINT ( 'NONE',  ( 13.28437500061451715, -4.541064518000419881, 2.621784821874995952 ) ) ;
#20132 = ORIENTED_EDGE ( 'NONE', *, *, #68150, .F. ) ;
#20133 = DIRECTION ( 'NONE',  ( 0.000000000000000000, 0.000000000000000000, 1.000000000000000000 ) ) ;
#20134 = CARTESIAN_POINT ( 'NONE',  ( 24.14062500061451289, -3.027376345333610441, -5.243569643749999898 ) ) ;
#20135 = CARTESIAN_POINT ( 'NONE',  ( 3.397178649298551179, 3.668675132081069545, -3.397178649298551179 ) ) ;
#20136 = CARTESIAN_POINT ( 'NONE',  ( 28.04999999999999716, 4.330127018922192761, -2.499999999999997780 ) ) ;
#20137 = CARTESIAN_POINT ( 'NONE',  ( 15.18750000000000000, -2.886751345948129988, 4.999999999999997335 ) ) ;
#20138 = CARTESIAN_POINT ( 'NONE',  ( 25.01250000122903216, 4.330127018922192761, -2.499999999999997780 ) ) ;
#20139 = CARTESIAN_POINT ( 'NONE',  ( 19.30312500061451786, 4.541064518000418104, -2.621784821874998173 ) ) ;
#20140 = EDGE_LOOP ( 'NONE', ( #61509, #40122, #11990, #19183 ) ) ;
#20141 = CARTESIAN_POINT ( 'NONE',  ( 22.50000000000000000, -4.330127018922190985, -2.500000000000001332 ) ) ;
#20142 =( BOUNDED_CURVE ( )  B_SPLINE_CURVE ( 2, ( #36700, #2729, #3835, #41883, #71425, #25244, #42980, #64411, #47793, #70323, #19699, #42252, #14166, #31159, #25623, #65511, #48160, #65140, #14531, #54074, #37065, #9002, #14898, #59960, #37439, #120, #5653, #72155, #32263, #50717, #22625, #32630, #49992, #66243, #45176, #71798, #5283, #67707, #17079, #55894, #39640, #10821, #16354, #27829, #4202, #72516, #9729, #21905, #38541, #61786, #32992, #50361, #10101, #21534, #11190, #33356, #15992, #55170, #33717, #49265, #56262, #43720, #60686, #15621, #61428, #66616, #44461, #66992, #55532, #67356, #44089, #28188, #54795, #26730, #72888, #38909, #4566, #4926, #61065, #21167, #22269, #38163, #44821, #27096, #10462, #49628, #27461, #16719, #39274, #18152, #11910, #39998, #40719, #34435, #23349, #6734, #45898, #56963, #6367, #28899, #51438, #56611, #840, #68429, #68072, #62512, #17441, #18521, #6006, #11555, #18878, #63236, #62871, #17792, #69520, #28541, #24435, #45543, #51798, #58045, #40352, #12267, #62158, #34797, #57330, #29268, #1201, #23706, #35524, #46257, #68796, #12630, #57689, #51076, #52160, #35165, #7094, #29623, #12988, #1563, #24073, #46618, #69162, #41086, #63598, #34071, #473, #22981, #7453, #29980, #52521, #1930, #46984, #8545, #8180, #14809, #47340, #2639, #30708, #36980, #58405, #42529, #69874, #19239, #65420, #3004, #31446, #25158, #64692, #70236, #59875, #9280, #31073, #41441, #70970, #8915, #31814, #37353, #53241, #63959, #54353, #53987, #13343, #20345, #70603, #42896, #48446, #3384, #25906, #3746, #7818, #47699, #65055, #48075, #14446, #35880, #53613, #26271, #25533, #19609, #48808, #59502, #19976, #71337, #30353, #52882, #2280, #24797, #41794, #58771, #42166, #59137, #64322, #13714, #36256 ),
 .UNSPECIFIED., .F., .F. ) 
 B_SPLINE_CURVE_WITH_KNOTS ( ( 3, 2, 2, 2, 2, 2, 2, 2, 2, 2, 2, 2, 2, 2, 2, 2, 2, 2, 2, 2, 2, 2, 2, 2, 2, 2, 2, 2, 2, 2, 2, 2, 2, 2, 2, 2, 2, 2, 2, 2, 2, 2, 2, 2, 2, 2, 2, 2, 2, 2, 2, 2, 2, 2, 2, 2, 2, 2, 2, 2, 2, 2, 2, 2, 2, 2, 2, 2, 2, 2, 2, 2, 2, 2, 2, 2, 2, 2, 2, 2, 2, 2, 2, 2, 2, 2, 2, 2, 2, 2, 2, 2, 2, 2, 2, 2, 2, 2, 2, 2, 2, 2, 2, 2, 2, 2, 2, 3 ),
 ( 0.000000000000000000, 0.009375299769173351880, 0.01875059953834670376, 0.02812589930752005737, 0.03750119907669340752, 0.04687649884586676113, 0.05625179861504011475, 0.06562709838421346142, 0.07500239815338681504, 0.08437769792256016865, 0.09375299769173352227, 0.1031282974609068759, 0.1125035972300802295, 0.1218788969992535831, 0.1312541967684269228, 0.1406294965376002903, 0.1500047963067736301, 0.1593800960759469976, 0.1687553958451203373, 0.1781306956142937048, 0.1875059953834670445, 0.1968812951526404120, 0.2062565949218137518, 0.2156318946909871193, 0.2250071944601604590, 0.2343824942293338265, 0.2437577939985071662, 0.2531330937676805615, 0.2625083935368538457, 0.2718836933060272409, 0.2812589930752005807, 0.2906342928443739204, 0.3000095926135472602, 0.3093848923827206554, 0.3187601921518939951, 0.3281354919210673349, 0.3375107916902406746, 0.3468860914594140699, 0.3562613912285874096, 0.3656366909977607493, 0.3750119907669340891, 0.3843872905361074843, 0.3937625903052808241, 0.4031378900744541638, 0.4125131898436275035, 0.4218884896128008988, 0.4312637893819742385, 0.4406390891511475782, 0.4500143889203209180, 0.4593896886894943132, 0.4687649884586676530, 0.4781402882278409927, 0.4875155879970143324, 0.4968908877661877277, 0.5062661875353611229, 0.5156414873045345182, 0.5250167870737076914, 0.5343920868428810866, 0.5437673866120544819, 0.5531426863812277661, 0.5625179861504011614, 0.5718932859195744456, 0.5812685856887478408, 0.5906438854579212361, 0.6000191852270945203, 0.6093944849962679156, 0.6187697847654413108, 0.6281450845346145950, 0.6375203843037879903, 0.6468956840729612745, 0.6562709838421346698, 0.6656462836113080650, 0.6750215833804813492, 0.6843968831496547445, 0.6937721829188281397, 0.7031474826880014239, 0.7125227824571748192, 0.7218980822263481034, 0.7312733819955214987, 0.7406486817646948939, 0.7500239815338681781, 0.7593992813030415734, 0.7687745810722149686, 0.7781498808413882529, 0.7875251806105616481, 0.7969004803797350434, 0.8062757801489083276, 0.8156510799180817228, 0.8250263796872550071, 0.8344016794564284023, 0.8437769792256017976, 0.8531522789947750818, 0.8625275787639484770, 0.8719028785331218723, 0.8812781783022951565, 0.8906534780714685517, 0.9000287778406418360, 0.9094040776098152312, 0.9187793773789886265, 0.9281546771481619107, 0.9375299769173353059, 0.9469052766865087012, 0.9562805764556819854, 0.9656558762248553807, 0.9750311759940286649, 0.9844064757632020601, 0.9937817755323754554, 1.000000000000000000 ),
 .UNSPECIFIED. ) 
 CURVE ( )  GEOMETRIC_REPRESENTATION_ITEM ( )  RATIONAL_B_SPLINE_CURVE ( ( 1.000000000000000000, 0.8660254037844387076, 1.000000000000000000, 0.8660254037844387076, 1.000000000000000000, 0.8660254037844387076, 1.000000000000000000, 0.8660254037844387076, 1.000000000000000000, 0.8660254037844387076, 1.000000000000000000, 0.8660254037844387076, 1.000000000000000000, 0.8660254037844387076, 1.000000000000000000, 0.8660254037844387076, 1.000000000000000000, 0.8660254037844387076, 1.000000000000000000, 0.8660254037844387076, 1.000000000000000000, 0.8660254037844387076, 1.000000000000000000, 0.8660254037844387076, 1.000000000000000000, 0.8660254037844387076, 1.000000000000000000, 0.8660254037844387076, 1.000000000000000000, 0.8660254037844387076, 1.000000000000000000, 0.8660254037844387076, 1.000000000000000000, 0.8660254037844387076, 1.000000000000000000, 0.8660254037844387076, 1.000000000000000000, 0.8660254037844387076, 1.000000000000000000, 0.8660254037844387076, 1.000000000000000000, 0.8660254037844387076, 1.000000000000000000, 0.8660254037844387076, 1.000000000000000000, 0.8660254037844387076, 1.000000000000000000, 0.8660254037844387076, 1.000000000000000000, 0.8660254037844387076, 1.000000000000000000, 0.8660254037844387076, 1.000000000000000000, 0.8660254037844387076, 1.000000000000000000, 0.8660254037844387076, 1.000000000000000000, 0.8660254037844387076, 1.000000000000000000, 0.8660254037844387076, 1.000000000000000000, 0.8660254037844387076, 1.000000000000000000, 0.8660254037844387076, 1.000000000000000000, 0.8660254037844387076, 1.000000000000000000, 0.8660254037844387076, 1.000000000000000000, 0.8660254037844387076, 1.000000000000000000, 0.8660254037844387076, 1.000000000000000000, 0.8660254037844387076, 1.000000000000000000, 0.8660254037844387076, 1.000000000000000000, 0.8660254037844387076, 1.000000000000000000, 0.8660254037844387076, 1.000000000000000000, 0.8660254037844387076, 1.000000000000000000, 0.8660254037844387076, 1.000000000000000000, 0.8660254037844387076, 1.000000000000000000, 0.8660254037844387076, 1.000000000000000000, 0.8660254037844387076, 1.000000000000000000, 0.8660254037844387076, 1.000000000000000000, 0.8660254037844387076, 1.000000000000000000, 0.8660254037844387076, 1.000000000000000000, 0.8660254037844387076, 1.000000000000000000, 0.8660254037844387076, 1.000000000000000000, 0.8660254037844387076, 1.000000000000000000, 0.8660254037844387076, 1.000000000000000000, 0.8660254037844387076, 1.000000000000000000, 0.8660254037844387076, 1.000000000000000000, 0.8660254037844387076, 1.000000000000000000, 0.8660254037844387076, 1.000000000000000000, 0.8660254037844387076, 1.000000000000000000, 0.8660254037844387076, 1.000000000000000000, 0.8660254037844387076, 1.000000000000000000, 0.8660254037844387076, 1.000000000000000000, 0.8660254037844387076, 1.000000000000000000, 0.8660254037844387076, 1.000000000000000000, 0.8660254037844387076, 1.000000000000000000, 0.8660254037844387076, 1.000000000000000000, 0.8660254037844387076, 1.000000000000000000, 0.8660254037844387076, 1.000000000000000000, 0.8660254037844387076, 1.000000000000000000, 0.8660254037844387076, 1.000000000000000000, 0.8660254037844387076, 1.000000000000000000, 0.8660254037844387076, 1.000000000000000000, 0.8660254037844387076, 1.000000000000000000, 0.8660254037844387076, 1.000000000000000000, 0.8660254037844387076, 1.000000000000000000, 0.8660254037844387076, 1.000000000000000000, 0.8660254037844387076, 1.000000000000000000, 0.8660254037844387076, 1.000000000000000000, 0.8660254037844387076, 1.000000000000000000, 0.8660254037844387076, 1.000000000000000000, 0.8660254037844387076, 1.000000000000000000, 0.8660254037844387076, 1.000000000000000000, 0.8660254037844387076, 1.000000000000000000, 0.8660254037844387076, 1.000000000000000000, 0.8660254037844387076, 1.000000000000000000, 0.8660254037844387076, 1.000000000000000000, 0.8660254037844387076, 1.000000000000000000, 0.8660254037844387076, 1.000000000000000000, 0.8660254037844387076, 1.000000000000000000, 0.8660254037844387076, 1.000000000000000000, 0.8660254037844387076, 1.000000000000000000, 0.8660254037844387076, 1.000000000000000000, 0.8660254037844387076, 1.000000000000000000, 0.8660254037844387076, 1.000000000000000000, 0.8660254037844387076, 1.000000000000000000, 0.8660254037844387076, 1.000000000000000000, 0.8660254037844387076, 1.000000000000000000, 0.8660254037844387076, 1.000000000000000000, 0.8660254037844387076, 1.000000000000000000, 0.8660254037844387076, 1.000000000000000000, 0.8660254037844387076, 1.000000000000000000, 0.8660254037844387076, 1.000000000000000000, 0.8660254037844387076, 1.000000000000000000, 0.8660254037844387076, 1.000000000000000000, 0.8660254037844387076, 1.000000000000000000, 0.8660254037844387076, 1.000000000000000000, 0.8660254037844387076, 1.000000000000000000, 0.8660254037844387076, 1.000000000000000000, 0.9111405360107026619, 0.9401542295230078672 ) ) 
 REPRESENTATION_ITEM ( '' )  );
#20143 = CARTESIAN_POINT ( 'NONE',  ( 24.87187500061451573, 3.027376345333611329, 5.243569643749999010 ) ) ;
#20144 = ORIENTED_EDGE ( 'NONE', *, *, #61389, .T. ) ;
#20145 = CARTESIAN_POINT ( 'NONE',  ( 13.27500000122903323, 2.886751345948129099, -4.999999999999997335 ) ) ;
#20146 = CARTESIAN_POINT ( 'NONE',  ( 13.86562500061451431, 3.027376345333613106, -5.243569643749998122 ) ) ;
#20147 = CARTESIAN_POINT ( 'NONE',  ( 3.515625000614516882, 3.027376345333613106, -5.243569643749998122 ) ) ;
#20148 = CARTESIAN_POINT ( 'NONE',  ( 16.24687500061451573, 0.000000000000000000, 4.756430356249998326 ) ) ;
#20149 = CARTESIAN_POINT ( 'NONE',  ( 27.51562500061451644, 3.027376345333611329, 5.243569643749999010 ) ) ;
#20150 = CARTESIAN_POINT ( 'NONE',  ( 11.85000000122903430, -2.886751345948125991, -5.000000000000000000 ) ) ;
#20151 = CARTESIAN_POINT ( 'NONE',  ( 19.91250000000000142, 2.886751345948129099, -4.999999999999998224 ) ) ;
#20152 = CARTESIAN_POINT ( 'NONE',  ( 26.13749999999999929, -2.886751345948125991, -5.000000000000000000 ) ) ;
#20153 = DIRECTION ( 'NONE',  ( 0.000000000000000000, 0.000000000000000000, -1.000000000000000000 ) ) ;
#20154 = CARTESIAN_POINT ( 'NONE',  ( 7.734375000614517326, 4.541064518000418104, 2.621784821874999949 ) ) ;
#20155 = CARTESIAN_POINT ( 'NONE',  ( 16.54687500061451644, -3.027376345333610441, -5.243569643749999898 ) ) ;
#20156 = CARTESIAN_POINT ( 'NONE',  ( -3.999999999999999112, 13.77500000122903678, 27.69059892324149885 ) ) ;
#20157 = EDGE_LOOP ( 'NONE', ( #42698, #38536, #46786 ) ) ;
#20158 = CARTESIAN_POINT ( 'NONE',  ( 26.20312500061451644, 0.000000000000000000, 5.243569643749999010 ) ) ;
#20159 = CARTESIAN_POINT ( 'NONE',  ( 28.58437500061451786, -4.541064518000419881, 2.621784821874995952 ) ) ;
#20160 = LINE ( 'NONE', #26086, #69872 ) ;
#20161 = CARTESIAN_POINT ( 'NONE',  ( 17.06250000000000000, -5.773502691896255534, -1.060575238724906372E-15 ) ) ;
#20162 = CARTESIAN_POINT ( 'NONE',  ( 11.61562500061451608, 3.027376345333613106, -5.243569643749998122 ) ) ;
#20163 = CARTESIAN_POINT ( 'NONE',  ( 15.35625000122903216, -4.330127018922190985, -2.500000000000001332 ) ) ;
#20164 = CARTESIAN_POINT ( 'NONE',  ( 9.731250001229033941, 4.330127018922191873, 2.499999999999999556 ) ) ;
#20165 = CARTESIAN_POINT ( 'NONE',  ( 29.76562500061451644, 3.027376345333611329, 5.243569643749999010 ) ) ;
#20166 = CARTESIAN_POINT ( 'NONE',  ( 17.62500000122903288, -5.773502691896255534, -1.060575238724906372E-15 ) ) ;
#20167 = CARTESIAN_POINT ( 'NONE',  ( 15.07500000122903394, 2.886751345948129099, -4.999999999999997335 ) ) ;
#20168 = CARTESIAN_POINT ( 'NONE',  ( 18.45937500061451431, 4.119189519843966529, -2.378215178124998275 ) ) ;
#20169 = CARTESIAN_POINT ( 'NONE',  ( 6.290625000614517681, 6.054752690667223547, 3.707466751127219781E-16 ) ) ;
#20170 = CARTESIAN_POINT ( 'NONE',  ( 24.12187500061451217, -6.054752690667223547, -1.112240025338166033E-15 ) ) ;
#20171 = CARTESIAN_POINT ( 'NONE',  ( -3.000416591977282496E-16, 17.49687500061451573, 25.09994784771203058 ) ) ;
#20172 = CARTESIAN_POINT ( 'NONE',  ( 24.98437500061451644, -4.541064518000419881, 2.621784821874995952 ) ) ;
#20173 = CARTESIAN_POINT ( 'NONE',  ( 4.162499999999999645, 2.886751345948129099, -4.999999999999998224 ) ) ;
#20174 = CARTESIAN_POINT ( 'NONE',  ( 1.999999999999998668, 11.86250000122903359, 26.53589838486224650 ) ) ;
#20175 = CARTESIAN_POINT ( 'NONE',  ( 11.72812500061451857, 4.541064518000418104, 2.621784821874999949 ) ) ;
#20176 = CARTESIAN_POINT ( 'NONE',  ( 3.300000001229034918, -2.886751345948125991, -5.000000000000000000 ) ) ;
#20177 = PRODUCT_DEFINITION_SHAPE ( 'NONE', 'NONE',  #2500 ) ;
#20178 = CARTESIAN_POINT ( 'NONE',  ( 8.296875000614516438, -3.027376345333614438, 5.243569643749998122 ) ) ;
#20179 = CARTESIAN_POINT ( 'NONE',  ( 3.934813120841985423, -3.085075400804674572, 3.963314313556091761 ) ) ;
#20180 = CARTESIAN_POINT ( 'NONE',  ( 10.15312500061451750, -4.541064518000417216, -2.621784821875001281 ) ) ;
#20181 = CARTESIAN_POINT ( 'NONE',  ( 14.14687500061451786, -3.027376345333614438, 5.243569643749998122 ) ) ;
#20182 = FACE_OUTER_BOUND ( 'NONE', #53739, .T. ) ;
#20183 = CARTESIAN_POINT ( 'NONE',  ( 21.45000000122903216, 5.773502691896255534, 3.535250795749688894E-16 ) ) ;
#20184 = CARTESIAN_POINT ( 'NONE',  ( 9.946875000614516793, 6.054752690667223547, 3.707466751127219781E-16 ) ) ;
#20185 = CARTESIAN_POINT ( 'NONE',  ( 12.10312500061451857, 4.541064518000418104, -2.621784821874998173 ) ) ;
#20186 = CARTESIAN_POINT ( 'NONE',  ( 28.66875000122902861, 2.886751345948126879, 4.999999999999999112 ) ) ;
#20187 = CARTESIAN_POINT ( 'NONE',  ( 20.70937500061451786, 4.541064518000418104, -2.621784821874998173 ) ) ;
#20188 = DIRECTION ( 'NONE',  ( 0.000000000000000000, 0.000000000000000000, 1.000000000000000000 ) ) ;
#20189 = CARTESIAN_POINT ( 'NONE',  ( -3.026485248664595673, 3.985774251745325181, 32.62744762453846903 ) ) ;
#20190 = CYLINDRICAL_SURFACE ( 'NONE', #60820, 4.999999999999998224 ) ;
#20191 = CARTESIAN_POINT ( 'NONE',  ( 4.243569643749999898, 14.64687500061451964, -27.54997392385601529 ) ) ;
#20192 = CARTESIAN_POINT ( 'NONE',  ( 15.15937500061451715, -4.541064518000417216, -2.621784821875001281 ) ) ;
#20193 = CARTESIAN_POINT ( 'NONE',  ( 14.70000000122903394, 5.773502691896255534, 3.535250795749688894E-16 ) ) ;
#20194 = CARTESIAN_POINT ( 'NONE',  ( 12.53437500061451537, 6.421520780324663323E-16, -5.243569643749999010 ) ) ;
#20195 = CARTESIAN_POINT ( 'NONE',  ( -3.000416591977282496E-16, 16.99062500061451786, -34.90005215228797653 ) ) ;
#20196 = CARTESIAN_POINT ( 'NONE',  ( 16.76250000122903216, -4.330127018922190985, -2.500000000000001332 ) ) ;
#20197 = CARTESIAN_POINT ( 'NONE',  ( 11.42812500061451608, -4.541064518000419881, 2.621784821874995952 ) ) ;
#20198 = EDGE_LOOP ( 'NONE', ( #13004, #52313, #69522, #9648 ) ) ;
#20199 = CARTESIAN_POINT ( 'NONE',  ( 16.31250000000000000, 2.886751345948129099, -4.999999999999998224 ) ) ;
#20200 = DIRECTION ( 'NONE',  ( -1.000000000000000000, -0.000000000000000000, -0.000000000000000000 ) ) ;
#20201 = CARTESIAN_POINT ( 'NONE',  ( 10.62187500061451750, -6.054752690667223547, -1.112240025338166033E-15 ) ) ;
#20202 = CARTESIAN_POINT ( 'NONE',  ( 15.88125000122903074, 6.123233995736764310E-16, -4.999999999999998224 ) ) ;
#20203 = CARTESIAN_POINT ( 'NONE',  ( 11.96250000122903501, 4.330127018922192761, -2.499999999999997780 ) ) ;
#20204 = CARTESIAN_POINT ( 'NONE',  ( 19.91250000122903074, -4.330127018922190985, -2.500000000000001332 ) ) ;
#20205 = CARTESIAN_POINT ( 'NONE',  ( 16.86562500061451786, -6.054752690667223547, -1.112240025338166033E-15 ) ) ;
#20206 = EDGE_CURVE ( 'NONE', #45031, #7627, #6363, .T. ) ;
#20207 = CARTESIAN_POINT ( 'NONE',  ( 21.77812500061451928, -4.541064518000419881, 2.621784821874995952 ) ) ;
#20208 = CARTESIAN_POINT ( 'NONE',  ( 28.76250000122903216, 0.000000000000000000, 4.999999999999998224 ) ) ;
#20209 = CARTESIAN_POINT ( 'NONE',  ( 3.478125000614517237, 6.421520780324663323E-16, -5.243569643749999010 ) ) ;
#20210 = CARTESIAN_POINT ( 'NONE',  ( 26.06250000000000000, -5.773502691896255534, -1.060575238724906372E-15 ) ) ;
#20211 = CARTESIAN_POINT ( 'NONE',  ( 17.45625000122903003, 0.000000000000000000, 4.999999999999998224 ) ) ;
#20212 = CARTESIAN_POINT ( 'NONE',  ( 29.84999999999999787, 4.330127018922192761, -2.499999999999997780 ) ) ;
#20213 = CARTESIAN_POINT ( 'NONE',  ( 28.20937500061451786, -4.541064518000417216, -2.621784821875001281 ) ) ;
#20214 = CYLINDRICAL_SURFACE ( 'NONE', #41762, 4.999999999999998224 ) ;
#20215 = CARTESIAN_POINT ( 'NONE',  ( 4.125000001229034652, -5.773502691896255534, -1.060575238724906372E-15 ) ) ;
#20216 = CARTESIAN_POINT ( 'NONE',  ( 4.650000000000001243, 4.330127018922192761, -2.499999999999997780 ) ) ;
#20217 = DIRECTION ( 'NONE',  ( -0.000000000000000000, 8.673617379884035472E-17, 1.000000000000000000 ) ) ;
#20218 = CARTESIAN_POINT ( 'NONE',  ( 8.071875000614518569, 3.027376345333613106, -5.243569643749998122 ) ) ;
#20219 = CARTESIAN_POINT ( 'NONE',  ( 26.46562500061451573, 3.027376345333613106, -5.243569643749998122 ) ) ;
#20220 = CARTESIAN_POINT ( 'NONE',  ( 1.071796769724491227, 17.09240381056766367, 26.00000000000000000 ) ) ;
#20221 = CARTESIAN_POINT ( 'NONE',  ( 14.24999999999999822, 0.000000000000000000, 4.999999999999998224 ) ) ;
#20222 = CARTESIAN_POINT ( 'NONE',  ( 1.626862140677534273E-15, 17.52500000122903145, -26.00000000000000355 ) ) ;
#20223 = CARTESIAN_POINT ( 'NONE',  ( 5.971875000614516260, 3.027376345333611329, 5.243569643749999010 ) ) ;
#20224 = CARTESIAN_POINT ( 'NONE',  ( 9.421875000614519990, 3.027376345333613106, -5.243569643749998122 ) ) ;
#20225 = CARTESIAN_POINT ( 'NONE',  ( 4.500000000000000888, -4.330127018922190985, -2.500000000000001332 ) ) ;
#20226 = EDGE_CURVE ( 'NONE', #11359, #72067, #52942, .T. ) ;
#20227 = CARTESIAN_POINT ( 'NONE',  ( -2.121784821874996840, 12.67812500061459602, 33.67503911421598417 ) ) ;
#20228 = PRESENTATION_LAYER_ASSIGNMENT (  '', '', ( #33226 ) ) ;
#20229 = CARTESIAN_POINT ( 'NONE',  ( 28.46249999999999858, 2.886751345948129099, -4.999999999999998224 ) ) ;
#20230 = CARTESIAN_POINT ( 'NONE',  ( 4.612500000000002487, 2.886751345948129099, -4.999999999999998224 ) ) ;
#20231 = CARTESIAN_POINT ( 'NONE',  ( 15.30937500061451573, 2.746126346562643317, 4.756430356249998326 ) ) ;
#20232 = ORIENTED_EDGE ( 'NONE', *, *, #52283, .F. ) ;
#20233 = CARTESIAN_POINT ( 'NONE',  ( 19.52812500061451573, -4.541064518000419881, 2.621784821874995952 ) ) ;
#20234 = CARTESIAN_POINT ( 'NONE',  ( 10.41562500061451679, 3.027376345333611329, 5.243569643749999010 ) ) ;
#20235 = CARTESIAN_POINT ( 'NONE',  ( 24.04687500061451289, -4.119189519843965641, -2.378215178125001383 ) ) ;
#20236 = CARTESIAN_POINT ( 'NONE',  ( 6.834375000614518747, 4.541064518000418104, 2.621784821874999949 ) ) ;
#20237 = CARTESIAN_POINT ( 'NONE',  ( 23.06250000000000355, 2.886751345948129099, -4.999999999999998224 ) ) ;
#20238 = CARTESIAN_POINT ( 'NONE',  ( 19.12500000122903288, 2.886751345948129099, -4.999999999999998224 ) ) ;
#20239 = CARTESIAN_POINT ( 'NONE',  ( 28.41562500061451502, 3.027376345333611329, 5.243569643749999010 ) ) ;
#20240 = CARTESIAN_POINT ( 'NONE',  ( 45.00000000000000000, -2.499999999999999556, -3.499999999999999556 ) ) ;
#20241 = CARTESIAN_POINT ( 'NONE',  ( 10.47187500061451715, 3.027376345333611329, 5.243569643749999010 ) ) ;
#20242 = CARTESIAN_POINT ( 'NONE',  ( 14.82187500061451679, 3.027376345333613106, -5.243569643749998122 ) ) ;
#20243 = CARTESIAN_POINT ( 'NONE',  ( 25.02187500061451431, -6.054752690667223547, -1.112240025338166033E-15 ) ) ;
#20244 = ADVANCED_FACE ( 'NONE', ( #65766 ), #15148, .F. ) ;
#20245 = CARTESIAN_POINT ( 'NONE',  ( 13.27500000000000213, 4.330127018922191873, 2.499999999999999556 ) ) ;
#20246 = CARTESIAN_POINT ( 'NONE',  ( 20.14687500061451786, -3.027376345333610441, -5.243569643749999898 ) ) ;
#20247 = CARTESIAN_POINT ( 'NONE',  ( 8.709375000614517859, 0.000000000000000000, 5.243569643749999010 ) ) ;
#20248 = CARTESIAN_POINT ( 'NONE',  ( -3.756430356250001434, 19.76562499938548356, 32.16877607737301048 ) ) ;
#20249 = CARTESIAN_POINT ( 'NONE',  ( 23.02499999999999858, 6.123233995736764310E-16, -4.999999999999998224 ) ) ;
#20250 = CARTESIAN_POINT ( 'NONE',  ( -8.484601909799255319E-16, 15.08750000000000036, 34.61880215351700940 ) ) ;
#20251 = CARTESIAN_POINT ( 'NONE',  ( 4.243569643749999010, 12.47187500061451715, -32.45002607614398471 ) ) ;
#20252 = CARTESIAN_POINT ( 'NONE',  ( 24.53437500061451715, -4.119189519843968306, 2.378215178124996054 ) ) ;
#20253 = CARTESIAN_POINT ( 'NONE',  ( 13.75312500061451715, -4.541064518000417216, -2.621784821875001281 ) ) ;
#20254 = CARTESIAN_POINT ( 'NONE',  ( 5.625000000000001776, 4.330127018922191873, 2.499999999999999556 ) ) ;
#20255 = CYLINDRICAL_SURFACE ( 'NONE', #27807, 4.000000000000000000 ) ;
#20256 = CYLINDRICAL_SURFACE ( 'NONE', #62165, 4.999999999999998224 ) ;
#20257 = CARTESIAN_POINT ( 'NONE',  ( 12.52500000000000213, -4.330127018922194537, 2.499999999999995559 ) ) ;
#20258 = CARTESIAN_POINT ( 'NONE',  ( 2.000000000000001332, 17.56250000122903288, 33.46410161513774995 ) ) ;
#20259 = CARTESIAN_POINT ( 'NONE',  ( 10.57500000122903572, 2.886751345948129099, -4.999999999999998224 ) ) ;
#20260 = CARTESIAN_POINT ( 'NONE',  ( 22.13437500061451502, 4.541064518000418104, 2.621784821874999949 ) ) ;
#20261 = CARTESIAN_POINT ( 'NONE',  ( 15.42187500061451821, 3.027376345333611329, 5.243569643749999010 ) ) ;
#20262 = FACE_OUTER_BOUND ( 'NONE', #32096, .T. ) ;
#20263 = VERTEX_POINT ( 'NONE', #59851 ) ;
#20264 = CARTESIAN_POINT ( 'NONE',  ( 17.76562500061451644, -6.054752690667223547, -1.112240025338166033E-15 ) ) ;
#20265 = CARTESIAN_POINT ( 'NONE',  ( 28.31250000122903288, 0.000000000000000000, 4.999999999999998224 ) ) ;
#20266 = CARTESIAN_POINT ( 'NONE',  ( 16.69687500061451502, 6.054752690667223547, 3.707466751127219781E-16 ) ) ;
#20267 = CARTESIAN_POINT ( 'NONE',  ( 28.58437500061451786, -4.541064518000419881, 2.621784821874995952 ) ) ;
#20268 = CARTESIAN_POINT ( 'NONE',  ( 5.503125000614516260, 0.000000000000000000, 5.243569643749999010 ) ) ;
#20269 = CARTESIAN_POINT ( 'NONE',  ( 18.85312500061451502, 4.541064518000418104, -2.621784821874998173 ) ) ;
#20270 = CARTESIAN_POINT ( 'NONE',  ( -4.243569643749999898, 13.05312500061451786, 30.00000000000000000 ) ) ;
#20271 = CARTESIAN_POINT ( 'NONE',  ( 16.01250000122903216, 4.330127018922192761, -2.499999999999997780 ) ) ;
#20272 = CARTESIAN_POINT ( 'NONE',  ( 12.53437500061451537, 5.824947211148865298E-16, -4.756430356249998326 ) ) ;
#20273 = CARTESIAN_POINT ( 'NONE',  ( 7.303125000614516082, 0.000000000000000000, 5.243569643749999010 ) ) ;
#20274 = CARTESIAN_POINT ( 'NONE',  ( 28.00312500061451715, 0.000000000000000000, 5.243569643749999010 ) ) ;
#20275 = DIRECTION ( 'NONE',  ( 1.000000000000000000, 0.000000000000000000, 0.000000000000000000 ) ) ;
#20276 = CARTESIAN_POINT ( 'NONE',  ( 23.22187500061451715, -6.054752690667223547, -1.112240025338166033E-15 ) ) ;
#20277 = CARTESIAN_POINT ( 'NONE',  ( 13.67812500061451786, -4.541064518000419881, 2.621784821874995952 ) ) ;
#20278 = CARTESIAN_POINT ( 'NONE',  ( 23.17500000122903359, 2.886751345948129099, -4.999999999999998224 ) ) ;
#20279 = CARTESIAN_POINT ( 'NONE',  ( 22.82812500061451644, 6.421520780324663323E-16, -5.243569643749999010 ) ) ;
#20280 = CARTESIAN_POINT ( 'NONE',  ( 18.72187500061451360, -6.054752690667223547, -1.112240025338166033E-15 ) ) ;
#20281 = CARTESIAN_POINT ( 'NONE',  ( 15.40312500061451573, 0.000000000000000000, 5.243569643749999010 ) ) ;
#20282 = CARTESIAN_POINT ( 'NONE',  ( 2.121784821875001281, 15.05937500061451928, 33.67503911421598417 ) ) ;
#20283 = CARTESIAN_POINT ( 'NONE',  ( 19.90312500061451573, 0.000000000000000000, 5.243569643749999010 ) ) ;
#20284 = CARTESIAN_POINT ( 'NONE',  ( 29.24062500061451431, 6.054752690667223547, 3.707466751127219781E-16 ) ) ;
#20285 = ORIENTED_EDGE ( 'NONE', *, *, #18491, .T. ) ;
#20286 = ORIENTED_EDGE ( 'NONE', *, *, #70743, .T. ) ;
#20287 = CARTESIAN_POINT ( 'NONE',  ( 22.42500000000000071, -4.330127018922194537, 2.499999999999995559 ) ) ;
#20288 = CARTESIAN_POINT ( 'NONE',  ( 2.121784821875001281, 19.55937500061451573, -26.32496088578401938 ) ) ;
#20289 = CARTESIAN_POINT ( 'NONE',  ( 25.82812500061451644, -4.541064518000419881, 2.621784821874995952 ) ) ;
#20290 = CARTESIAN_POINT ( 'NONE',  ( 8.578125000614518214, 4.541064518000418104, 2.621784821874999949 ) ) ;
#20291 = CARTESIAN_POINT ( 'NONE',  ( 19.46250000122903145, -4.330127018922190985, -2.500000000000001332 ) ) ;
#20292 = CARTESIAN_POINT ( 'NONE',  ( 24.02812500061451573, -4.541064518000419881, 2.621784821874995952 ) ) ;
#20293 = CARTESIAN_POINT ( 'NONE',  ( 22.83749999999999858, -2.886751345948129988, 4.999999999999997335 ) ) ;
#20294 = CARTESIAN_POINT ( 'NONE',  ( 28.52812500061451573, -4.541064518000419881, 2.621784821874995952 ) ) ;
#20295 = CARTESIAN_POINT ( 'NONE',  ( 8.128125000614515372, 4.541064518000418104, 2.621784821874999949 ) ) ;
#20296 = ORIENTED_EDGE ( 'NONE', *, *, #50099, .F. ) ;
#20297 = AXIS2_PLACEMENT_3D ( 'NONE', #72104, #55124, #65460 ) ;
#20298 = CARTESIAN_POINT ( 'NONE',  ( 22.15312500061451573, 0.000000000000000000, 5.243569643749999010 ) ) ;
#20299 = CARTESIAN_POINT ( 'NONE',  ( 6.440625000614517148, -3.027376345333614438, 5.243569643749998122 ) ) ;
#20300 = CARTESIAN_POINT ( 'NONE',  ( 13.58437500061451786, 4.119189519843966529, 2.378215178124999607 ) ) ;
#20301 = CARTESIAN_POINT ( 'NONE',  ( 3.140625000614516882, 6.054752690667223547, 3.707466751127219781E-16 ) ) ;
#20302 = CARTESIAN_POINT ( 'NONE',  ( 4.000000000000000000, 14.45000000122903572, -27.69059892324149530 ) ) ;
#20303 = CARTESIAN_POINT ( 'NONE',  ( 1.626862140677534273E-15, 13.81250000000000000, -26.00000000000000355 ) ) ;
#20304 = CARTESIAN_POINT ( 'NONE',  ( 10.46249999999999858, 2.886751345948129099, -4.999999999999998224 ) ) ;
#20305 =( BOUNDED_CURVE ( )  B_SPLINE_CURVE ( 2, ( #60393, #14602, #9801, #15697, #36776, #3909, #8702, #9074, #37510 ),
 .UNSPECIFIED., .F., .F. ) 
 B_SPLINE_CURVE_WITH_KNOTS ( ( 3, 2, 2, 2, 3 ),
 ( 0.2717391304347826497, 0.2753623188405797118, 0.2826086956521738913, 0.2898550724637681264, 0.2934782608695652439 ),
 .UNSPECIFIED. ) 
 CURVE ( )  GEOMETRIC_REPRESENTATION_ITEM ( )  RATIONAL_B_SPLINE_CURVE ( ( 0.9330127018922194093, 0.9330127018922198534, 1.000000000000000000, 0.8660254037844387076, 1.000000000000000000, 0.8660254037844387076, 1.000000000000000000, 0.9330127018922188542, 0.9330127018922194093 ) ) 
 REPRESENTATION_ITEM ( '' )  );
#20306 = CARTESIAN_POINT ( 'NONE',  ( 10.17187500061451999, -6.054752690667223547, -1.112240025338166033E-15 ) ) ;
#20307 = CARTESIAN_POINT ( 'NONE',  ( 8.175000001229031810, -5.773502691896255534, -1.060575238724906372E-15 ) ) ;
#20308 = CARTESIAN_POINT ( 'NONE',  ( 14.25937500061451679, -4.541064518000417216, -2.621784821875001281 ) ) ;
#20309 = CARTESIAN_POINT ( 'NONE',  ( 14.32500000000000107, -4.330127018922194537, 2.499999999999995559 ) ) ;
#20310 = CARTESIAN_POINT ( 'NONE',  ( 6.459375000614518747, 0.000000000000000000, 5.243569643749999010 ) ) ;
#20311 = CARTESIAN_POINT ( 'NONE',  ( 5.190092854996874117, 9.698896338944486217, -35.22418694837048037 ) ) ;
#20312 = DIRECTION ( 'NONE',  ( -0.000000000000000000, -1.000000000000000000, -0.000000000000000000 ) ) ;
#20313 = CARTESIAN_POINT ( 'NONE',  ( 12.64687500061451608, 6.054752690667223547, 3.707466751127219781E-16 ) ) ;
#20314 = CARTESIAN_POINT ( 'NONE',  ( 3.657199499170772139, 3.409538812810354536, 3.983732690067115723 ) ) ;
#20315 = CARTESIAN_POINT ( 'NONE',  ( 22.52812500061451573, 4.541064518000418104, 2.621784821874999949 ) ) ;
#20316 = CARTESIAN_POINT ( 'NONE',  ( -4.243569643749999898, 10.82187500061451857, 27.54997392385601529 ) ) ;
#20317 = CARTESIAN_POINT ( 'NONE',  ( -2.121784821874999949, 18.82812500061459104, 26.32496088578401938 ) ) ;
#20318 = CARTESIAN_POINT ( 'NONE',  ( 25.28437500061451715, 4.541064518000418104, 2.621784821874999949 ) ) ;
#20319 = CARTESIAN_POINT ( 'NONE',  ( 4.117352459450578372, 2.836881972790640916, -4.222552775064624342 ) ) ;
#20320 = CARTESIAN_POINT ( 'NONE',  ( 4.678125000614516971, -4.541064518000419881, 2.621784821874995952 ) ) ;
#20321 = CARTESIAN_POINT ( 'NONE',  ( 21.87187500061451573, 5.824947211148865298E-16, -4.756430356249998326 ) ) ;
#20322 = CARTESIAN_POINT ( 'NONE',  ( 17.33437500061451431, -4.541064518000419881, 2.621784821874995952 ) ) ;
#20323 = CARTESIAN_POINT ( 'NONE',  ( 9.984375000614516438, -2.746126346562646425, 4.756430356249996549 ) ) ;
#20324 = CARTESIAN_POINT ( 'NONE',  ( 27.86250000122903359, 0.000000000000000000, 4.999999999999998224 ) ) ;
#20325 = CARTESIAN_POINT ( 'NONE',  ( 6.459375000614518747, 0.000000000000000000, 5.243569643749999010 ) ) ;
#20326 = CARTESIAN_POINT ( 'NONE',  ( 15.98437500061451821, -4.541064518000419881, 2.621784821874995952 ) ) ;
#20327 = CARTESIAN_POINT ( 'NONE',  ( 3.324079281300976962, 3.735364078604925364, -3.324079281300976962 ) ) ;
#20328 = CARTESIAN_POINT ( 'NONE',  ( 25.23749999999999716, -2.886751345948125991, -5.000000000000000000 ) ) ;
#20329 = EDGE_CURVE ( 'NONE', #46244, #21751, #9256, .T. ) ;
#20330 = CARTESIAN_POINT ( 'NONE',  ( 4.237500001229036251, 6.123233995736764310E-16, -4.999999999999998224 ) ) ;
#20331 = CARTESIAN_POINT ( 'NONE',  ( 26.74687500061451573, -3.027376345333614438, 5.243569643749998122 ) ) ;
#20332 = CARTESIAN_POINT ( 'NONE',  ( 1.878215178125000495, 14.62812499938548427, 26.74683588394047007 ) ) ;
#20333 = CARTESIAN_POINT ( 'NONE',  ( 14.17500000122903536, 2.886751345948129099, -4.999999999999997335 ) ) ;
#20334 = CARTESIAN_POINT ( 'NONE',  ( 8.362500000000002487, 2.886751345948126879, 4.999999999999999112 ) ) ;
#20335 = CARTESIAN_POINT ( 'NONE',  ( 10.17187500061451644, 5.824947211148865298E-16, -4.756430356249998326 ) ) ;
#20336 = CARTESIAN_POINT ( 'NONE',  ( 21.51562500061451644, 3.027376345333613106, -5.243569643749998122 ) ) ;
#20337 = CARTESIAN_POINT ( 'NONE',  ( 12.97499999999999964, -4.330127018922194537, 2.499999999999995559 ) ) ;
#20338 = CARTESIAN_POINT ( 'NONE',  ( 4.378125000614518925, 6.421520780324663323E-16, -5.243569643749999010 ) ) ;
#20339 = CARTESIAN_POINT ( 'NONE',  ( 19.31250000000000000, -5.773502691896255534, -1.060575238724906372E-15 ) ) ;
#20340 = CARTESIAN_POINT ( 'NONE',  ( 17.84062500061451573, -3.027376345333610441, -5.243569643749999898 ) ) ;
#20341 = CARTESIAN_POINT ( 'NONE',  ( -1.999999999999997113, 18.83750000122903501, 33.46410161513775705 ) ) ;
#20342 = VECTOR ( 'NONE', #48602, 1000.000000000000000 ) ;
#20344 = CARTESIAN_POINT ( 'NONE',  ( 23.06250000122903288, -4.330127018922190985, -2.500000000000001332 ) ) ;
#20343 = B_SPLINE_CURVE_WITH_KNOTS ( 'NONE', 3,
 ( #31277, #20179, #64155, #13542, #70442, #53079, #36090, #42734, #19818, #42005 ),
 .UNSPECIFIED., .F., .F.,
 ( 4, 3, 3, 4 ),
 ( 2.616501308845268417E-17, 7.861561263978005779E-05, 0.0001572308220202767550, 0.0002825258805215967667 ),
 .UNSPECIFIED. ) ;
#20345 = CARTESIAN_POINT ( 'NONE',  ( 2.655984681222220721E-16, 19.50312499938548427, 25.66244784525396483 ) ) ;
#20346 = CARTESIAN_POINT ( 'NONE',  ( 29.67187500061451644, 3.027376345333613106, -5.243569643749998122 ) ) ;
#20347 = ORIENTED_EDGE ( 'NONE', *, *, #45040, .T. ) ;
#20348 = CARTESIAN_POINT ( 'NONE',  ( 19.11562500061451431, -6.054752690667223547, -1.112240025338166033E-15 ) ) ;
#20349 = CARTESIAN_POINT ( 'NONE',  ( 25.49062500061451786, -3.027376345333610441, -5.243569643749999898 ) ) ;
#20350 = CARTESIAN_POINT ( 'NONE',  ( 23.78437500061451360, 6.421520780324663323E-16, -5.243569643749999010 ) ) ;
#20351 = CARTESIAN_POINT ( 'NONE',  ( 9.225000000000001421, 4.330127018922191873, 2.499999999999999556 ) ) ;
#20352 = CARTESIAN_POINT ( 'NONE',  ( 11.65312500061451573, 4.541064518000418104, -2.621784821874998173 ) ) ;
#20353 = CARTESIAN_POINT ( 'NONE',  ( 25.79062500061451502, -3.027376345333614438, 5.243569643749998122 ) ) ;
#20354 = CARTESIAN_POINT ( 'NONE',  ( 17.63437500061451502, 4.541064518000418104, 2.621784821874999949 ) ) ;
#20355 = CARTESIAN_POINT ( 'NONE',  ( 9.365625000614519635, 3.027376345333613106, -5.243569643749998122 ) ) ;
#20356 = CARTESIAN_POINT ( 'NONE',  ( 1.071796769724491227, 14.78615380933863044, 26.00000000000000000 ) ) ;
#20357 = CARTESIAN_POINT ( 'NONE',  ( 4.243569643749999010, 13.37187500061451750, 27.54997392385601174 ) ) ;
#20358 =( BOUNDED_CURVE ( )  B_SPLINE_CURVE ( 2, ( #41355, #63865, #53154, #47614, #70144, #64602, #59048 ),
 .UNSPECIFIED., .F., .F. ) 
 B_SPLINE_CURVE_WITH_KNOTS ( ( 3, 2, 2, 3 ),
 ( 0.2100000000000000477, 0.2133333333333333748, 0.2166666666666667018, 0.2200000000000000011 ),
 .UNSPECIFIED. ) 
 CURVE ( )  GEOMETRIC_REPRESENTATION_ITEM ( )  RATIONAL_B_SPLINE_CURVE ( ( 0.9999999999999977796, 0.8660254037844409281, 1.000000000000000000, 0.8660254037844387076, 1.000000000000000000, 0.8660254037844387076, 1.000000000000000000 ) ) 
 REPRESENTATION_ITEM ( '' )  );
#20359 = CARTESIAN_POINT ( 'NONE',  ( 23.88750000122903216, -4.330127018922194537, 2.499999999999995559 ) ) ;
#20360 = CARTESIAN_POINT ( 'NONE',  ( 18.49687500061452283, 5.492252693125287522, 3.363034840372157021E-16 ) ) ;
#20361 = CARTESIAN_POINT ( 'NONE',  ( 15.02812500061451750, -4.541064518000419881, 2.621784821874995952 ) ) ;
#20362 = CARTESIAN_POINT ( 'NONE',  ( 8.071875000614518569, 3.027376345333613106, -5.243569643749998122 ) ) ;
#20363 = CARTESIAN_POINT ( 'NONE',  ( 9.871875000614517504, 3.027376345333613106, -5.243569643749998122 ) ) ;
#20364 = EDGE_LOOP ( 'NONE', ( #43224, #52440, #69132, #50720 ) ) ;
#20365 = CARTESIAN_POINT ( 'NONE',  ( 29.37187500061451928, 3.027376345333611329, 5.243569643749999010 ) ) ;
#20366 = CARTESIAN_POINT ( 'NONE',  ( 22.64062500061451644, -3.027376345333614438, 5.243569643749998122 ) ) ;
#20367 = CARTESIAN_POINT ( 'NONE',  ( 16.73437500061451644, 4.541064518000418104, 2.621784821874999949 ) ) ;
#20368 = CARTESIAN_POINT ( 'NONE',  ( 21.74062500061451431, -3.027376345333614438, 5.243569643749998122 ) ) ;
#20369 = CARTESIAN_POINT ( 'NONE',  ( -2.828200636599751609E-16, 10.88750000000000107, 25.38119784648299770 ) ) ;
#20370 = CARTESIAN_POINT ( 'NONE',  ( 25.94062500061451715, -3.027376345333610441, -5.243569643749999898 ) ) ;
#20371 = CARTESIAN_POINT ( 'NONE',  ( 6.150000001229033231, 5.773502691896255534, 3.535250795749688894E-16 ) ) ;
#20372 = ORIENTED_EDGE ( 'NONE', *, *, #4888, .T. ) ;
#20373 = CARTESIAN_POINT ( 'NONE',  ( 29.77499999999999858, 6.123233995736764310E-16, -4.999999999999998224 ) ) ;
#20374 = CARTESIAN_POINT ( 'NONE',  ( 2.000000000000001332, 18.80000000000000071, -26.53589838486224650 ) ) ;
#20375 = CARTESIAN_POINT ( 'NONE',  ( 25.05000000122903714, 5.773502691896255534, 3.535250795749688894E-16 ) ) ;
#20376 = CARTESIAN_POINT ( 'NONE',  ( 3.756430356250000546, 15.94062499938548427, 27.83122392262697886 ) ) ;
#20377 = CARTESIAN_POINT ( 'NONE',  ( 7.096875000614517148, -3.027376345333610441, -5.243569643749999898 ) ) ;
#20378 = CARTESIAN_POINT ( 'NONE',  ( 4.291775470143723403, 2.565448060106937600, -4.323948581960670445 ) ) ;
#20379 = CARTESIAN_POINT ( 'NONE',  ( 14.16562500061451679, -6.054752690667223547, -1.112240025338166033E-15 ) ) ;
#20380 = CARTESIAN_POINT ( 'NONE',  ( 8.109375000614518214, 4.541064518000418104, -2.621784821874998173 ) ) ;
#20381 = CARTESIAN_POINT ( 'NONE',  ( 28.12500000122902932, 2.886751345948129099, -4.999999999999998224 ) ) ;
#20382 = CARTESIAN_POINT ( 'NONE',  ( 17.33437500061451431, -4.541064518000419881, 2.621784821874995952 ) ) ;
#20383 = CARTESIAN_POINT ( 'NONE',  ( 4.846875000614519813, -3.027376345333610441, -5.243569643749999898 ) ) ;
#20384 = CARTESIAN_POINT ( 'NONE',  ( 2.393811435568372112E-14, 18.23750000000000071, 34.00000000000000000 ) ) ;
#20385 = CARTESIAN_POINT ( 'NONE',  ( 5.090625000614516615, -3.027376345333614438, 5.243569643749998122 ) ) ;
#20386 = CARTESIAN_POINT ( 'NONE',  ( 14.87812500061451537, 4.541064518000418104, 2.621784821874999949 ) ) ;
#20387 = ADVANCED_FACE ( 'NONE', ( #26986 ), #33598, .F. ) ;
#20388 =( BOUNDED_CURVE ( )  B_SPLINE_CURVE ( 2, ( #62702, #50540, #12096, #68619, #57147 ),
 .UNSPECIFIED., .F., .F. ) 
 B_SPLINE_CURVE_WITH_KNOTS ( ( 3, 2, 3 ),
 ( 0.000000000000000000, 0.007246376811594202987, 0.01086956521739130578 ),
 .UNSPECIFIED. ) 
 CURVE ( )  GEOMETRIC_REPRESENTATION_ITEM ( )  RATIONAL_B_SPLINE_CURVE ( ( 1.000000000000000000, 0.8660254037844387076, 1.000000000000000000, 0.9330127018922192983, 0.9330127018922194093 ) ) 
 REPRESENTATION_ITEM ( '' )  );
#20389 = EDGE_LOOP ( 'NONE', ( #69940, #45298, #34513, #27593 ) ) ;
#20390 = CARTESIAN_POINT ( 'NONE',  ( 13.04062500061451502, 6.054752690667223547, 3.707466751127219781E-16 ) ) ;
#20391 = CARTESIAN_POINT ( 'NONE',  ( 6.300000001229033586, -2.886751345948129988, 4.999999999999997335 ) ) ;
#20392 = CARTESIAN_POINT ( 'NONE',  ( 11.72812500061451857, 4.541064518000418104, 2.621784821874999949 ) ) ;
#20393 = CARTESIAN_POINT ( 'NONE',  ( 21.49687500061451573, -2.746126346562642428, -4.756430356249999214 ) ) ;
#20394 = CARTESIAN_POINT ( 'NONE',  ( 10.08749999999999858, 5.773502691896255534, 3.535250795749688894E-16 ) ) ;
#20395 = CARTESIAN_POINT ( 'NONE',  ( 4.612500001229032698, -4.330127018922190985, -2.500000000000001332 ) ) ;
#20396 = CARTESIAN_POINT ( 'NONE',  ( 16.94999999999999929, 0.000000000000000000, 4.999999999999998224 ) ) ;
#20397 = CARTESIAN_POINT ( 'NONE',  ( 17.63437500061451502, 4.541064518000418104, 2.621784821874999949 ) ) ;
#20398 = CARTESIAN_POINT ( 'NONE',  ( 15.56250000122903465, 4.330127018922192761, -2.499999999999997780 ) ) ;
#20399 = CARTESIAN_POINT ( 'NONE',  ( 22.57499999999999929, 6.123233995736764310E-16, -4.999999999999998224 ) ) ;
#20400 =( BOUNDED_CURVE ( )  B_SPLINE_CURVE ( 2, ( #40412, #41144, #13043, #50506, #46316, #34858, #7875 ),
 .UNSPECIFIED., .F., .F. ) 
 B_SPLINE_CURVE_WITH_KNOTS ( ( 3, 2, 2, 3 ),
 ( 0.5916666666666667851, 0.5944444444444445530, 0.5972222222222222099, 0.5999999999999999778 ),
 .UNSPECIFIED. ) 
 CURVE ( )  GEOMETRIC_REPRESENTATION_ITEM ( )  RATIONAL_B_SPLINE_CURVE ( ( 0.9999999999999946709, 0.8660254037844440367, 1.000000000000000000, 0.8660254037844387076, 1.000000000000000000, 0.8660254037844387076, 1.000000000000000000 ) ) 
 REPRESENTATION_ITEM ( '' )  );
#20401 = CARTESIAN_POINT ( 'NONE',  ( 9.001249775931846008E-16, 17.66562500061451502, -25.09994784771203058 ) ) ;
#20402 = CARTESIAN_POINT ( 'NONE',  ( 3.243445638651676344, 3.805279306527807659, 3.607624186539012623 ) ) ;
#20403 = CARTESIAN_POINT ( 'NONE',  ( -3.999999999999999112, 18.64999999999999858, 30.00000000000000000 ) ) ;
#20404 = CARTESIAN_POINT ( 'NONE',  ( 3.581550526421168001, -3.489303470904949744, 3.581550526421168001 ) ) ;
#20405 = CARTESIAN_POINT ( 'NONE',  ( 29.72812500061451502, 4.541064518000418104, 2.621784821874999949 ) ) ;
#20406 = CARTESIAN_POINT ( 'NONE',  ( 11.98125000122903394, 4.330127018922191873, 2.499999999999999556 ) ) ;
#20407 = CARTESIAN_POINT ( 'NONE',  ( 17.03437500061451715, 6.421520780324663323E-16, -5.243569643749999010 ) ) ;
#20408 = CARTESIAN_POINT ( 'NONE',  ( 28.91250000000000497, 2.886751345948129099, -4.999999999999998224 ) ) ;
#20409 = CARTESIAN_POINT ( 'NONE',  ( 11.69062500061451360, 6.054752690667223547, 3.707466751127219781E-16 ) ) ;
#20410 = CARTESIAN_POINT ( 'NONE',  ( 7.856250001229033053, 4.330127018922192761, -2.499999999999997780 ) ) ;
#20411 = CARTESIAN_POINT ( 'NONE',  ( 23.33437500061451786, 6.421520780324663323E-16, -5.243569643749999010 ) ) ;
#20412 = CARTESIAN_POINT ( 'NONE',  ( 15.90937500061451537, -5.492252693125287522, -1.008910452111647106E-15 ) ) ;
#20413 = CARTESIAN_POINT ( 'NONE',  ( 7.490625000614516082, -3.027376345333610441, -5.243569643749999898 ) ) ;
#20414 = CARTESIAN_POINT ( 'NONE',  ( 12.75937500061451857, 0.000000000000000000, 5.243569643749999010 ) ) ;
#20415 = ORIENTED_EDGE ( 'NONE', *, *, #42313, .F. ) ;
#20416 = CARTESIAN_POINT ( 'NONE',  ( 23.55937500061451573, 0.000000000000000000, 5.243569643749999010 ) ) ;
#20417 = CARTESIAN_POINT ( 'NONE',  ( 27.92812500061451431, 4.541064518000418104, 2.621784821874999949 ) ) ;
#20418 = CYLINDRICAL_SURFACE ( 'NONE', #1883, 4.000000000000000000 ) ;
#20419 = CARTESIAN_POINT ( 'NONE',  ( 6.937499999999999112, 5.773502691896255534, 3.535250795749688894E-16 ) ) ;
#20420 = CARTESIAN_POINT ( 'NONE',  ( 17.62500000122903288, -5.773502691896255534, -1.060575238724906372E-15 ) ) ;
#20421 = LINE ( 'NONE', #65870, #31343 ) ;
#20422 = CARTESIAN_POINT ( 'NONE',  ( 8.746875000614515727, -4.119189519843965641, -2.378215178125001383 ) ) ;
#20423 = ORIENTED_EDGE ( 'NONE', *, *, #6209, .F. ) ;
#20424 = CARTESIAN_POINT ( 'NONE',  ( 14.77500000000000036, -4.330127018922194537, 2.499999999999995559 ) ) ;
#20425 = CARTESIAN_POINT ( 'NONE',  ( 19.91250000000000142, 2.886751345948129099, -4.999999999999998224 ) ) ;
#20426 = CARTESIAN_POINT ( 'NONE',  ( 11.61562500061451608, 3.027376345333613106, -5.243569643749998122 ) ) ;
#20427 = ORIENTED_EDGE ( 'NONE', *, *, #19299, .F. ) ;
#20428 = CARTESIAN_POINT ( 'NONE',  ( 0.000000000000000000, 20.00000000000000000, -33.99999999999999289 ) ) ;
#20429 = CARTESIAN_POINT ( 'NONE',  ( -2.121784821874996840, 17.68437500061451928, -26.32496088578401583 ) ) ;
#20430 = CARTESIAN_POINT ( 'NONE',  ( 4.378125000614518925, 6.421520780324663323E-16, -5.243569643749999010 ) ) ;
#20431 = CARTESIAN_POINT ( 'NONE',  ( 19.70625000122903359, 0.000000000000000000, 4.999999999999998224 ) ) ;
#20432 = CARTESIAN_POINT ( 'NONE',  ( 9.787499999999999645, -2.886751345948129988, 4.999999999999997335 ) ) ;
#20433 = FACE_OUTER_BOUND ( 'NONE', #5264, .T. ) ;
#20434 = ORIENTED_EDGE ( 'NONE', *, *, #53141, .F. ) ;
#20435 = CARTESIAN_POINT ( 'NONE',  ( -3.000416591977282496E-16, 14.29062500061451679, 25.09994784771203058 ) ) ;
#20436 = CARTESIAN_POINT ( 'NONE',  ( 25.97812500061451502, 6.421520780324663323E-16, -5.243569643749999010 ) ) ;
#20437 = CARTESIAN_POINT ( 'NONE',  ( 8.887499999999999289, -2.886751345948129988, 4.999999999999997335 ) ) ;
#20438 = CYLINDRICAL_SURFACE ( 'NONE', #36028, 4.999999999999998224 ) ;
#20439 = CARTESIAN_POINT ( 'NONE',  ( 22.84687500061451715, -3.027376345333610441, -5.243569643749999898 ) ) ;
#20440 = CARTESIAN_POINT ( 'NONE',  ( 20.16562500061451146, 3.027376345333613106, -5.243569643749998122 ) ) ;
#20441 = CARTESIAN_POINT ( 'NONE',  ( 4.243569643749999010, 12.86562500061459424, -32.45002607614398471 ) ) ;
#20442 = CARTESIAN_POINT ( 'NONE',  ( 24.03750000122903430, 6.123233995736764310E-16, -4.999999999999998224 ) ) ;
#20443 = CARTESIAN_POINT ( 'NONE',  ( 3.703125000614516882, 0.000000000000000000, 5.243569643749999010 ) ) ;
#20444 = CARTESIAN_POINT ( 'NONE',  ( 27.38437500061451857, 5.824947211148865298E-16, -4.756430356249998326 ) ) ;
#20445 = CARTESIAN_POINT ( 'NONE',  ( 22.71562500061451573, -6.054752690667223547, -1.112240025338166033E-15 ) ) ;
#20446 = DIRECTION ( 'NONE',  ( 0.000000000000000000, 0.000000000000000000, -1.000000000000000000 ) ) ;
#20447 = CARTESIAN_POINT ( 'NONE',  ( 2.655984681222220721E-16, 16.80312499938548143, 25.66244784525396483 ) ) ;
#20448 = CARTESIAN_POINT ( 'NONE',  ( 16.47187500061452070, -6.054752690667223547, -1.112240025338166033E-15 ) ) ;
#20449 = CARTESIAN_POINT ( 'NONE',  ( 15.75937500061451857, 4.541064518000418104, -2.621784821874998173 ) ) ;
#20450 = CARTESIAN_POINT ( 'NONE',  ( 24.79687500061451999, 6.054752690667223547, 3.707466751127219781E-16 ) ) ;
#20451 = CARTESIAN_POINT ( 'NONE',  ( 9.001249775931846008E-16, 14.57187500061451679, 34.90005215228797653 ) ) ;
#20452 = CARTESIAN_POINT ( 'NONE',  ( 4.078125000614517326, 4.541064518000418104, 2.621784821874999949 ) ) ;
#20453 = CARTESIAN_POINT ( 'NONE',  ( 28.15312500061451573, -4.541064518000417216, -2.621784821875001281 ) ) ;
#20454 = CARTESIAN_POINT ( 'NONE',  ( 34.99999999999999289, 2.500000000000000000, -3.500000000000000000 ) ) ;
#20455 = CARTESIAN_POINT ( 'NONE',  ( 2.000000000000001332, 19.25000000000000000, 33.46410161513774995 ) ) ;
#20456 = CARTESIAN_POINT ( 'NONE',  ( 6.684375000614518392, 6.421520780324663323E-16, -5.243569643749999010 ) ) ;
#20457 = CARTESIAN_POINT ( 'NONE',  ( 13.50000000122903288, -2.886751345948129988, 4.999999999999997335 ) ) ;
#20458 = CARTESIAN_POINT ( 'NONE',  ( 9.562500001229032875, -4.330127018922190985, -2.500000000000001332 ) ) ;
#20459 = CARTESIAN_POINT ( 'NONE',  ( 5.653125000614517504, -4.541064518000417216, -2.621784821875001281 ) ) ;
#20460 = CARTESIAN_POINT ( 'NONE',  ( -2.000000000000001776, 17.24374999877096570, 33.46410161513775705 ) ) ;
#20461 = CARTESIAN_POINT ( 'NONE',  ( 21.76875000122903359, 2.886751345948129099, -4.999999999999998224 ) ) ;
#20462 = CARTESIAN_POINT ( 'NONE',  ( 15.30937500061451750, 4.541064518000418104, -2.621784821874998173 ) ) ;
#20463 = CARTESIAN_POINT ( 'NONE',  ( 11.81250000000000000, 2.886751345948129099, -4.999999999999997335 ) ) ;
#20464 = ORIENTED_EDGE ( 'NONE', *, *, #23875, .T. ) ;
#20465 = CARTESIAN_POINT ( 'NONE',  ( 21.62812500061451360, 4.541064518000418104, 2.621784821874999949 ) ) ;
#20466 = CARTESIAN_POINT ( 'NONE',  ( 6.890625000614516438, -3.027376345333614438, 5.243569643749998122 ) ) ;
#20467 = CARTESIAN_POINT ( 'NONE',  ( 23.67187500061451644, -6.054752690667223547, -1.112240025338166033E-15 ) ) ;
#20468 = CARTESIAN_POINT ( 'NONE',  ( 8.503125000614515372, 4.541064518000418104, -2.621784821874998173 ) ) ;
#20469 = DIRECTION ( 'NONE',  ( 0.000000000000000000, 0.000000000000000000, -1.000000000000000000 ) ) ;
#20470 = CARTESIAN_POINT ( 'NONE',  ( 7.575000001229033053, 2.886751345948126879, 4.999999999999999112 ) ) ;
#20471 = CARTESIAN_POINT ( 'NONE',  ( 22.37812500061451360, 6.421520780324663323E-16, -5.243569643749999010 ) ) ;
#20472 = EDGE_CURVE ( 'NONE', #38561, #20937, #36209, .T. ) ;
#20473 = CARTESIAN_POINT ( 'NONE',  ( 4.243569643749999010, 11.06562500061451715, -32.45002607614398471 ) ) ;
#20474 = CARTESIAN_POINT ( 'NONE',  ( 9.300000001229035362, 5.773502691896255534, 3.535250795749688894E-16 ) ) ;
#20475 = CARTESIAN_POINT ( 'NONE',  ( 18.92812500061451431, 4.541064518000418104, 2.621784821874999949 ) ) ;
#20476 = CARTESIAN_POINT ( 'NONE',  ( 16.90312500061451573, -4.541064518000417216, -2.621784821875001281 ) ) ;
#20477 = CARTESIAN_POINT ( 'NONE',  ( 29.03437500061451715, -4.119189519843968306, 2.378215178124996054 ) ) ;
#20478 = CARTESIAN_POINT ( 'NONE',  ( 17.06250000000000000, -5.773502691896255534, -1.060575238724906372E-15 ) ) ;
#20479 = CARTESIAN_POINT ( 'NONE',  ( 11.58750000122903501, 4.330127018922191873, 2.499999999999999556 ) ) ;
#20480 = CARTESIAN_POINT ( 'NONE',  ( 7.153125000614518392, 4.541064518000418104, -2.621784821874998173 ) ) ;
#20481 = CARTESIAN_POINT ( 'NONE',  ( 13.15312500061451750, 0.000000000000000000, 5.243569643749999010 ) ) ;
#20482 = CARTESIAN_POINT ( 'NONE',  ( 22.50000000122903288, -2.886751345948129988, 4.999999999999997335 ) ) ;
#20483 = CARTESIAN_POINT ( 'NONE',  ( 22.69687500061451857, -3.027376345333614438, 5.243569643749998122 ) ) ;
#20484 = CARTESIAN_POINT ( 'NONE',  ( 3.586992791275801729, 3.483314903268937446, -3.919380039434936513 ) ) ;
#20485 = CARTESIAN_POINT ( 'NONE',  ( 6.337500001229033231, -4.330127018922194537, 2.499999999999995559 ) ) ;
#20486 = CARTESIAN_POINT ( 'NONE',  ( 6.459375000614518747, 0.000000000000000000, 5.243569643749999010 ) ) ;
#20487 = CARTESIAN_POINT ( 'NONE',  ( 22.54687500061451999, 6.054752690667223547, 3.707466751127219781E-16 ) ) ;
#20488 = CARTESIAN_POINT ( 'NONE',  ( -5.000000000000000000, 39.99999999999999289, 30.00000000000000000 ) ) ;
#20489 = CARTESIAN_POINT ( 'NONE',  ( 17.76562500061451644, -6.054752690667223547, -1.112240025338166033E-15 ) ) ;
#20490 = CARTESIAN_POINT ( 'NONE',  ( 24.79687500061451999, 6.054752690667223547, 3.707466751127219781E-16 ) ) ;
#20491 = CARTESIAN_POINT ( 'NONE',  ( 3.756430356250000102, 19.50312499938548072, 30.00000000000000000 ) ) ;
#20492 = CARTESIAN_POINT ( 'NONE',  ( 45.00000000000000000, -2.499999999999999556, 3.499999999999999556 ) ) ;
#20493 = CARTESIAN_POINT ( 'NONE',  ( 10.93125000122903501, 6.123233995736764310E-16, -4.999999999999998224 ) ) ;
#20494 = CARTESIAN_POINT ( 'NONE',  ( 5.109375000614518214, 0.000000000000000000, 5.243569643749999010 ) ) ;
#20495 = CARTESIAN_POINT ( 'NONE',  ( 14.57812500061451644, -4.541064518000419881, 2.621784821874995952 ) ) ;
#20496 = CARTESIAN_POINT ( 'NONE',  ( 13.43437500061451750, 6.421520780324663323E-16, -5.243569643749999010 ) ) ;
#20497 = VERTEX_POINT ( 'NONE', #56850 ) ;
#20498 = CARTESIAN_POINT ( 'NONE',  ( 4.000000000000000000, 12.69687499938548392, 30.00000000000000000 ) ) ;
#20499 = CARTESIAN_POINT ( 'NONE',  ( 24.25312500061451715, 4.541064518000418104, -2.621784821874998173 ) ) ;
#20500 = CARTESIAN_POINT ( 'NONE',  ( 26.96250000122903145, 0.000000000000000000, 4.999999999999998224 ) ) ;
#20501 = CARTESIAN_POINT ( 'NONE',  ( -1.999999999999999112, 20.29999999999999716, 26.53589838486224650 ) ) ;
#20502 = CARTESIAN_POINT ( 'NONE',  ( 13.50000000000000178, -4.330127018922190985, -2.500000000000001332 ) ) ;
#20503 = CARTESIAN_POINT ( 'NONE',  ( 23.47500000122903430, -5.773502691896255534, -1.060575238724906372E-15 ) ) ;
#20504 = CARTESIAN_POINT ( 'NONE',  ( 19.34062500061451573, 6.054752690667223547, 3.707466751127219781E-16 ) ) ;
#20505 = ORIENTED_EDGE ( 'NONE', *, *, #30054, .T. ) ;
#20506 = CARTESIAN_POINT ( 'NONE',  ( 22.76249999999999574, 2.886751345948126879, 4.999999999999999112 ) ) ;
#20507 = CARTESIAN_POINT ( 'NONE',  ( 23.82187500061451502, 3.027376345333613106, -5.243569643749998122 ) ) ;
#20508 = VERTEX_POINT ( 'NONE', #29156 ) ;
#20509 = FACE_OUTER_BOUND ( 'NONE', #46973, .T. ) ;
#20510 = CARTESIAN_POINT ( 'NONE',  ( 9.665625000614515017, -6.054752690667223547, -1.112240025338166033E-15 ) ) ;
#20511 = CARTESIAN_POINT ( 'NONE',  ( 3.665625000614517681, 3.027376345333611329, 5.243569643749999010 ) ) ;
#20512 = CARTESIAN_POINT ( 'NONE',  ( 14.10937500061451644, -5.492252693125287522, -1.008910452111647106E-15 ) ) ;
#20513 = CARTESIAN_POINT ( 'NONE',  ( 27.70312500061451289, -4.541064518000417216, -2.621784821875001281 ) ) ;
#20514 = CARTESIAN_POINT ( 'NONE',  ( 18.33749999999999858, -2.886751345948129988, 4.999999999999997335 ) ) ;
#20515 = CARTESIAN_POINT ( 'NONE',  ( 27.33750000000000213, -2.886751345948129988, 4.999999999999997335 ) ) ;
#20516 = CARTESIAN_POINT ( 'NONE',  ( 3.089506346739232967, 3.931278485869285522, -3.469880700456108968 ) ) ;
#20517 = CARTESIAN_POINT ( 'NONE',  ( 6.609375000614519102, -4.541064518000417216, -2.621784821875001281 ) ) ;
#20518 = CARTESIAN_POINT ( 'NONE',  ( 17.33437500061451431, -4.541064518000419881, 2.621784821874995952 ) ) ;
#20519 = CARTESIAN_POINT ( 'NONE',  ( 19.83750000122903145, -4.330127018922194537, 2.499999999999995559 ) ) ;
#20520 = EDGE_LOOP ( 'NONE', ( #69993, #70575, #41880, #11576 ) ) ;
#20521 = CARTESIAN_POINT ( 'NONE',  ( 27.36562500061451786, 3.027376345333613106, -5.243569643749998122 ) ) ;
#20522 = CARTESIAN_POINT ( 'NONE',  ( 28.69687500061451502, -3.027376345333610441, -5.243569643749999898 ) ) ;
#20523 = CARTESIAN_POINT ( 'NONE',  ( 12.75000000000000178, 4.330127018922192761, -2.499999999999997780 ) ) ;
#20524 = CARTESIAN_POINT ( 'NONE',  ( 11.24062500061451608, 6.054752690667223547, 3.707466751127219781E-16 ) ) ;
#20525 = LINE ( 'NONE', #42717, #13594 ) ;
#20526 = CARTESIAN_POINT ( 'NONE',  ( 9.693750001229032520, 5.773502691896255534, 3.535250795749688401E-16 ) ) ;
#20527 = CARTESIAN_POINT ( 'NONE',  ( 27.74062500061451431, -3.027376345333610441, -5.243569643749999898 ) ) ;
#20528 = CARTESIAN_POINT ( 'NONE',  ( 18.56250000122903288, -4.330127018922190985, -2.500000000000001332 ) ) ;
#20529 = CARTESIAN_POINT ( 'NONE',  ( 8.681250001229031454, 6.123233995736764310E-16, -4.999999999999998224 ) ) ;
#20530 = CARTESIAN_POINT ( 'NONE',  ( 16.69687500061451502, 5.492252693125287522, 3.363034840372157021E-16 ) ) ;
#20531 = CARTESIAN_POINT ( 'NONE',  ( 5.840625000614516615, 6.054752690667223547, 3.707466751127219781E-16 ) ) ;
#20532 = CARTESIAN_POINT ( 'NONE',  ( 21.19687500061451502, 6.054752690667223547, 3.707466751127219781E-16 ) ) ;
#20534 = CARTESIAN_POINT ( 'NONE',  ( 4.243569643749999898, 17.34687500061451715, 32.45002607614398471 ) ) ;
#20533 =( BOUNDED_CURVE ( )  B_SPLINE_CURVE ( 2, ( #63286, #7143, #29673, #24121, #25493, #18569, #46670 ),
 .UNSPECIFIED., .F., .F. ) 
 B_SPLINE_CURVE_WITH_KNOTS ( ( 3, 2, 2, 3 ),
 ( 0.02999999999999993991, 0.03333333333333331899, 0.03666666666666669461, 0.04000000000000007022 ),
 .UNSPECIFIED. ) 
 CURVE ( )  GEOMETRIC_REPRESENTATION_ITEM ( )  RATIONAL_B_SPLINE_CURVE ( ( 1.000000000000002442, 0.8660254037844364872, 1.000000000000000000, 0.8660254037844387076, 1.000000000000000000, 0.8660254037844359321, 1.000000000000002887 ) ) 
 REPRESENTATION_ITEM ( '' )  );
#20535 = CARTESIAN_POINT ( 'NONE',  ( 23.85937500061451644, 4.541064518000418104, -2.621784821874998173 ) ) ;
#20536 = CARTESIAN_POINT ( 'NONE',  ( 5.100000000000000533, 4.330127018922192761, -2.499999999999997780 ) ) ;
#20537 = CARTESIAN_POINT ( 'NONE',  ( 1.999999999999998668, 11.41250000122903430, 26.53589838486224650 ) ) ;
#20538 = CARTESIAN_POINT ( 'NONE',  ( 13.19062500061451537, -3.027376345333614438, 5.243569643749998122 ) ) ;
#20539 = CARTESIAN_POINT ( 'NONE',  ( 3.187500001229033764, -4.330127018922194537, 2.499999999999995559 ) ) ;
#20540 = CARTESIAN_POINT ( 'NONE',  ( 9.796875000614519990, -3.027376345333610441, -5.243569643749999898 ) ) ;
#20541 = FACE_OUTER_BOUND ( 'NONE', #66466, .T. ) ;
#20542 = CARTESIAN_POINT ( 'NONE',  ( 11.05312500061451608, -4.541064518000417216, -2.621784821875001281 ) ) ;
#20543 = CARTESIAN_POINT ( 'NONE',  ( 15.42187500061451821, 3.027376345333611329, 5.243569643749999010 ) ) ;
#20544 = DIRECTION ( 'NONE',  ( -0.000000000000000000, -1.000000000000000000, -0.000000000000000000 ) ) ;
#20545 = CARTESIAN_POINT ( 'NONE',  ( 20.62500000122903288, 2.886751345948126879, 4.999999999999999112 ) ) ;
#20546 = CARTESIAN_POINT ( 'NONE',  ( 11.14687500061451608, -3.027376345333610441, -5.243569643749999898 ) ) ;
#20547 = CARTESIAN_POINT ( 'NONE',  ( 12.44062500061451537, -3.027376345333610441, -5.243569643749999898 ) ) ;
#20548 = ADVANCED_FACE ( 'NONE', ( #22514 ), #45787, .F. ) ;
#20549 = CARTESIAN_POINT ( 'NONE',  ( 29.04375000122903216, 5.773502691896255534, 3.535250795749688894E-16 ) ) ;
#20550 = CARTESIAN_POINT ( 'NONE',  ( 22.09687500061451715, 6.054752690667223547, 3.707466751127219781E-16 ) ) ;
#20551 = DIRECTION ( 'NONE',  ( -1.000000000000000000, -0.000000000000000000, -0.000000000000000000 ) ) ;
#20552 = CARTESIAN_POINT ( 'NONE',  ( -0.1380872570243143471, 5.000000000000001776, 34.00000000000000000 ) ) ;
#20553 = CARTESIAN_POINT ( 'NONE',  ( 3.211615563433569243, 3.832169812614073745, -3.409004327678504698 ) ) ;
#20554 = CARTESIAN_POINT ( 'NONE',  ( 2.121784821875001281, 13.70937500061451786, -26.32496088578401938 ) ) ;
#20555 = CARTESIAN_POINT ( 'NONE',  ( 15.52500000122903323, 2.886751345948129099, -4.999999999999998224 ) ) ;
#20556 = CARTESIAN_POINT ( 'NONE',  ( 9.496875000614517504, 6.054752690667223547, 3.707466751127219781E-16 ) ) ;
#20557 = CARTESIAN_POINT ( 'NONE',  ( -3.000416591977282496E-16, 17.89062500061451644, -34.90005215228797653 ) ) ;
#20558 = CARTESIAN_POINT ( 'NONE',  ( 17.28750000122903430, 6.123233995736764310E-16, -4.999999999999998224 ) ) ;
#20559 = CARTESIAN_POINT ( 'NONE',  ( 10.11562500061451608, -6.054752690667223547, -1.112240025338166033E-15 ) ) ;
#20560 = VECTOR ( 'NONE', #2752, 1000.000000000000000 ) ;
#20561 = ORIENTED_EDGE ( 'NONE', *, *, #42309, .T. ) ;
#20562 = CARTESIAN_POINT ( 'NONE',  ( 15.41250000000000142, 2.886751345948129099, -4.999999999999998224 ) ) ;
#20563 = CARTESIAN_POINT ( 'NONE',  ( 10.53750000122903252, 6.123233995736764310E-16, -4.999999999999998224 ) ) ;
#20564 = CARTESIAN_POINT ( 'NONE',  ( 10.39687500061451786, 6.054752690667223547, 3.707466751127219781E-16 ) ) ;
#20565 = CARTESIAN_POINT ( 'NONE',  ( -2.000000000000000000, 14.18750000122903288, 26.53589838486224650 ) ) ;
#20566 = CARTESIAN_POINT ( 'NONE',  ( 10.53750000122903252, 6.123233995736764310E-16, -4.999999999999998224 ) ) ;
#20567 = CARTESIAN_POINT ( 'NONE',  ( 18.78750000122903430, 4.330127018922191873, 2.499999999999999556 ) ) ;
#20568 = VECTOR ( 'NONE', #48416, 1000.000000000000000 ) ;
#20569 = CARTESIAN_POINT ( 'NONE',  ( 14.12812500061451715, -4.541064518000419881, 2.621784821874995952 ) ) ;
#20570 = CARTESIAN_POINT ( 'NONE',  ( 20.35312500061451502, 0.000000000000000000, 5.243569643749999010 ) ) ;
#20571 = CARTESIAN_POINT ( 'NONE',  ( 27.60000000122903430, -2.886751345948125991, -5.000000000000000000 ) ) ;
#20572 = AXIS2_PLACEMENT_3D ( 'NONE', #63324, #58129, #69603 ) ;
#20573 = CARTESIAN_POINT ( 'NONE',  ( 2.953125000614516438, -4.541064518000417216, -2.621784821875001281 ) ) ;
#20574 = CARTESIAN_POINT ( 'NONE',  ( 24.41250000000000142, 2.886751345948129099, -4.999999999999998224 ) ) ;
#20575 = CARTESIAN_POINT ( 'NONE',  ( 28.38749999999999929, -2.886751345948130432, -4.999999999999991118 ) ) ;
#20576 = VECTOR ( 'NONE', #71302, 1000.000000000000000 ) ;
#20577 = CARTESIAN_POINT ( 'NONE',  ( 26.92499999999999716, -4.330127018922194537, 2.499999999999995559 ) ) ;
#20578 = CARTESIAN_POINT ( 'NONE',  ( 29.22187500061451715, 3.027376345333613106, -5.243569643749998122 ) ) ;
#20579 = CARTESIAN_POINT ( 'NONE',  ( -1.071796769724496556, 16.04240381056766651, 33.99999999999998579 ) ) ;
#20580 = CARTESIAN_POINT ( 'NONE',  ( 12.41250000122903430, 4.330127018922192761, -2.499999999999997780 ) ) ;
#20581 = CARTESIAN_POINT ( 'NONE',  ( 4.087500000000001243, -2.886751345948125991, -5.000000000000000000 ) ) ;
#20582 =( BOUNDED_CURVE ( )  B_SPLINE_CURVE ( 2, ( #21429, #38434, #61683, #67609, #16974, #39900, #12166 ),
 .UNSPECIFIED., .F., .F. ) 
 B_SPLINE_CURVE_WITH_KNOTS ( ( 3, 2, 2, 3 ),
 ( 0.3900000000000000133, 0.3933333333333333126, 0.3966666666666667229, 0.4000000000000000777 ),
 .UNSPECIFIED. ) 
 CURVE ( )  GEOMETRIC_REPRESENTATION_ITEM ( )  RATIONAL_B_SPLINE_CURVE ( ( 1.000000000000000000, 0.8660254037844387076, 1.000000000000000000, 0.8660254037844387076, 1.000000000000000000, 0.8660254037844364872, 1.000000000000002220 ) ) 
 REPRESENTATION_ITEM ( '' )  );
#20583 = CARTESIAN_POINT ( 'NONE',  ( 12.59999999999999964, -4.330127018922190985, -2.500000000000001332 ) ) ;
#20584 = CARTESIAN_POINT ( 'NONE',  ( 7.809375000614519280, 0.000000000000000000, 5.243569643749999010 ) ) ;
#20585 = CARTESIAN_POINT ( 'NONE',  ( 25.30312500061451431, 0.000000000000000000, 5.243569643749999010 ) ) ;
#20586 = CARTESIAN_POINT ( 'NONE',  ( -3.756430356250000990, 13.46562499938548285, 32.16877607737301048 ) ) ;
#20587 = CARTESIAN_POINT ( 'NONE',  ( 65.00000000000000000, 0.000000000000000000, 0.000000000000000000 ) ) ;
#20588 = CARTESIAN_POINT ( 'NONE',  ( 3.737800990869664552, -3.321044174263025006, 4.023844142270481150 ) ) ;
#20589 = CARTESIAN_POINT ( 'NONE',  ( 4.996875000614516615, 6.054752690667223547, 3.707466751127219781E-16 ) ) ;
#20590 = CARTESIAN_POINT ( 'NONE',  ( 7.996875000614519280, -3.027376345333610441, -5.243569643749999898 ) ) ;
#20591 = CARTESIAN_POINT ( 'NONE',  ( 29.85937500061451644, 0.000000000000000000, 5.243569643749999010 ) ) ;
#20592 = CARTESIAN_POINT ( 'NONE',  ( 9.001249775931846008E-16, 13.16562500061459673, 34.90005215228797653 ) ) ;
#20593 = CARTESIAN_POINT ( 'NONE',  ( 22.83749999999999858, -2.886751345948129988, 4.999999999999997335 ) ) ;
#20594 = CARTESIAN_POINT ( 'NONE',  ( 29.21249999999999858, -5.773502691896255534, -1.060575238724906372E-15 ) ) ;
#20595 = CARTESIAN_POINT ( 'NONE',  ( 3.637500000000001954, -2.886751345948125991, -5.000000000000000000 ) ) ;
#20596 = ADVANCED_FACE ( 'NONE', ( #68322 ), #50602, .T. ) ;
#20597 = CARTESIAN_POINT ( 'NONE',  ( 13.80937500061451395, 2.746126346562645981, -4.756430356249997438 ) ) ;
#20598 = ORIENTED_EDGE ( 'NONE', *, *, #25778, .T. ) ;
#20599 = CARTESIAN_POINT ( 'NONE',  ( 18.32812500061451644, 6.421520780324663323E-16, -5.243569643749999010 ) ) ;
#20600 = CARTESIAN_POINT ( 'NONE',  ( 9.590625000614517504, -3.027376345333614438, 5.243569643749998122 ) ) ;
#20601 = CARTESIAN_POINT ( 'NONE',  ( 24.00937500061451502, -5.492252693125287522, -1.008910452111647106E-15 ) ) ;
#20602 = CARTESIAN_POINT ( 'NONE',  ( 7.471875000614519813, -6.054752690667223547, -1.112240025338166033E-15 ) ) ;
#20603 = CARTESIAN_POINT ( 'NONE',  ( 23.96249999999999858, 2.886751345948129099, -4.999999999999998224 ) ) ;
#20604 = CARTESIAN_POINT ( 'NONE',  ( 20.77500000122903145, -5.773502691896255534, -1.060575238724906372E-15 ) ) ;
#20606 = CARTESIAN_POINT ( 'NONE',  ( 28.52812500061451573, -4.541064518000419881, 2.621784821874995952 ) ) ;
#20605 = VECTOR ( 'NONE', #57741, 1000.000000000000000 ) ;
#20607 = CARTESIAN_POINT ( 'NONE',  ( 3.999999999999999112, 10.88750000122903394, 30.00000000000000000 ) ) ;
#20608 = CARTESIAN_POINT ( 'NONE',  ( 8.334375000614516082, -4.541064518000419881, 2.621784821874995952 ) ) ;
#20609 = CARTESIAN_POINT ( 'NONE',  ( 14.07187500061451679, 3.027376345333611329, 5.243569643749999010 ) ) ;
#20610 = CARTESIAN_POINT ( 'NONE',  ( 25.05937500061451573, -4.541064518000417216, -2.621784821875001281 ) ) ;
#20611 = CYLINDRICAL_SURFACE ( 'NONE', #620, 1.500000000000000444 ) ;
#20612 = CARTESIAN_POINT ( 'NONE',  ( 12.82499999999999929, 4.330127018922191873, 2.499999999999999556 ) ) ;
#20613 = CARTESIAN_POINT ( 'NONE',  ( 18.34687500061451715, -3.027376345333610441, -5.243569643749999898 ) ) ;
#20614 = AXIS2_PLACEMENT_3D ( 'NONE', #11552, #39996, #1199 ) ;
#20615 = CARTESIAN_POINT ( 'NONE',  ( 10.62187500061451928, -6.054752690667223547, -1.112240025338166033E-15 ) ) ;
#20616 = CARTESIAN_POINT ( 'NONE',  ( -1.878215178124999163, 13.24062499938548321, 26.74683588394047007 ) ) ;
#20617 = CARTESIAN_POINT ( 'NONE',  ( 23.21250000000000213, 2.886751345948126879, 4.999999999999999112 ) ) ;
#20618 = CARTESIAN_POINT ( 'NONE',  ( 3.999999999999998668, 14.26250000000000107, 32.30940107675850470 ) ) ;
#20619 = CARTESIAN_POINT ( 'NONE',  ( 29.96249999999999858, 2.886751345948126879, 4.999999999999998224 ) ) ;
#20620 = CARTESIAN_POINT ( 'NONE',  ( 24.42187500061451999, 2.746126346562643317, 4.756430356249998326 ) ) ;
#20621 = CARTESIAN_POINT ( 'NONE',  ( 11.42812500061451608, -4.541064518000419881, 2.621784821874995952 ) ) ;
#20622 = CARTESIAN_POINT ( 'NONE',  ( 29.29687500061451644, 6.054752690667223547, 3.707466751127219781E-16 ) ) ;
#20623 = CARTESIAN_POINT ( 'NONE',  ( 3.999999999999998668, 10.02500000122903323, -32.30940107675850470 ) ) ;
#20624 = CARTESIAN_POINT ( 'NONE',  ( 12.03749999999999964, -2.886751345948129988, 4.999999999999997335 ) ) ;
#20625 = CARTESIAN_POINT ( 'NONE',  ( 2.000000000000001332, 18.46250000122903501, 33.46410161513774995 ) ) ;
#20626 = CARTESIAN_POINT ( 'NONE',  ( 12.71250000122903145, -4.330127018922190985, -2.500000000000001332 ) ) ;
#20627 = CARTESIAN_POINT ( 'NONE',  ( 21.57187500061451502, 3.027376345333613106, -5.243569643749998122 ) ) ;
#20628 = CARTESIAN_POINT ( 'NONE',  ( 17.10937500061451999, 4.541064518000418104, -2.621784821874998173 ) ) ;
#20629 = FACE_BOUND ( 'NONE', #22442, .T. ) ;
#20630 = VERTEX_POINT ( 'NONE', #72770 ) ;
#20631 = CARTESIAN_POINT ( 'NONE',  ( 16.86562500061451786, -6.054752690667223547, -1.112240025338166033E-15 ) ) ;
#20632 = AXIS2_PLACEMENT_3D ( 'NONE', #65611, #64878, #53436 ) ;
#20633 = CARTESIAN_POINT ( 'NONE',  ( 28.12500000122902932, 2.886751345948129099, -4.999999999999998224 ) ) ;
#20634 = CARTESIAN_POINT ( 'NONE',  ( 18.15937500061451715, 0.000000000000000000, 5.243569643749999010 ) ) ;
#20635 = CARTESIAN_POINT ( 'NONE',  ( 29.10937500061451644, -4.541064518000417216, -2.621784821875001281 ) ) ;
#20636 = CARTESIAN_POINT ( 'NONE',  ( 4.115625000614516082, 3.027376345333611329, 5.243569643749999010 ) ) ;
#20637 = CARTESIAN_POINT ( 'NONE',  ( 19.49062500061451431, -3.027376345333614438, 5.243569643749998122 ) ) ;
#20638 = CARTESIAN_POINT ( 'NONE',  ( 27.94687500061451502, 6.054752690667223547, 3.707466751127219781E-16 ) ) ;
#20639 = CARTESIAN_POINT ( 'NONE',  ( 4.243569643749999010, 13.31562500061451537, 27.54997392385601174 ) ) ;
#20640 = CARTESIAN_POINT ( 'NONE',  ( 17.40000000122903145, 5.773502691896255534, 3.535250795749688894E-16 ) ) ;
#20641 = CARTESIAN_POINT ( 'NONE',  ( 10.88437500061451679, 4.119189519843966529, 2.378215178124999607 ) ) ;
#20642 = CARTESIAN_POINT ( 'NONE',  ( 7.753125000614518036, 0.000000000000000000, 5.243569643749999010 ) ) ;
#20643 = CARTESIAN_POINT ( 'NONE',  ( 26.84062500061451573, -3.027376345333610441, -5.243569643749999898 ) ) ;
#20644 = CARTESIAN_POINT ( 'NONE',  ( 2.393811435568372112E-14, 18.63124999877096855, 34.00000000000000000 ) ) ;
#20645 = CARTESIAN_POINT ( 'NONE',  ( 23.82187500061451502, 3.027376345333613106, -5.243569643749998122 ) ) ;
#20646 = CARTESIAN_POINT ( 'NONE',  ( 23.40000000122903145, -2.886751345948129988, 4.999999999999997335 ) ) ;
#20647 = CARTESIAN_POINT ( 'NONE',  ( 22.75312500061451360, -4.541064518000417216, -2.621784821875001281 ) ) ;
#20648 = CARTESIAN_POINT ( 'NONE',  ( 17.22187500061451715, 3.027376345333611329, 5.243569643749999010 ) ) ;
#20649 = CARTESIAN_POINT ( 'NONE',  ( 13.30312500061451786, -4.541064518000417216, -2.621784821875001281 ) ) ;
#20650 = CARTESIAN_POINT ( 'NONE',  ( 9.001249775931846008E-16, 14.12187500061451750, 34.90005215228797653 ) ) ;
#20651 = CARTESIAN_POINT ( 'NONE',  ( 19.11562500061451431, -6.054752690667223547, -1.112240025338166033E-15 ) ) ;
#20652 = CARTESIAN_POINT ( 'NONE',  ( 29.54062500061451502, -3.027376345333610441, -5.243569643749999898 ) ) ;
#20653 = VERTEX_POINT ( 'NONE', #61672 ) ;
#20654 = CARTESIAN_POINT ( 'NONE',  ( 23.66250000000000142, 2.886751345948126879, 4.999999999999999112 ) ) ;
#20655 = CARTESIAN_POINT ( 'NONE',  ( -3.000416591977282496E-16, 18.84687500061452070, -34.90005215228797653 ) ) ;
#20656 = CARTESIAN_POINT ( 'NONE',  ( 1.915124944151129771, -4.721073491456853510, 1.915124944151129771 ) ) ;
#20657 = CARTESIAN_POINT ( 'NONE',  ( 26.01562500061451289, 3.027376345333613106, -5.243569643749998122 ) ) ;
#20658 = CARTESIAN_POINT ( 'NONE',  ( 4.378125000614518925, 6.421520780324663323E-16, -5.243569643749999010 ) ) ;
#20659 = MANIFOLD_SOLID_BREP ( 'Thread1', #48907 ) ;
#20660 = CARTESIAN_POINT ( 'NONE',  ( 18.75000000122903288, 5.773502691896255534, 3.535250795749688894E-16 ) ) ;
#20661 = ADVANCED_FACE ( 'NONE', ( #57213 ), #11800, .T. ) ;
#20662 = CARTESIAN_POINT ( 'NONE',  ( 25.94062500061451715, -3.027376345333610441, -5.243569643749999898 ) ) ;
#20663 = CARTESIAN_POINT ( 'NONE',  ( 22.91249999999999432, -5.773502691896255534, -1.060575238724906372E-15 ) ) ;
#20664 = CARTESIAN_POINT ( 'NONE',  ( 27.36562500061451786, 3.027376345333613106, -5.243569643749998122 ) ) ;
#20665 = CARTESIAN_POINT ( 'NONE',  ( 7.565625000614518036, 3.027376345333613106, -5.243569643749998122 ) ) ;
#20666 = EDGE_LOOP ( 'NONE', ( #33083, #22259, #69325, #19629, #7407, #33543, #69321, #28131, #50552, #68749, #28455, #3337, #39344, #24424, #24054, #38166, #51564, #1544, #56528 ) ) ;
#20667 = CARTESIAN_POINT ( 'NONE',  ( 24.17812500061451786, 6.421520780324663323E-16, -5.243569643749999010 ) ) ;
#20668 = CARTESIAN_POINT ( 'NONE',  ( 5.240625000614516971, -3.027376345333610441, -5.243569643749999898 ) ) ;
#20669 = CARTESIAN_POINT ( 'NONE',  ( 14.67187500061451821, -5.492252693125287522, -1.008910452111647106E-15 ) ) ;
#20670 = CARTESIAN_POINT ( 'NONE',  ( 3.065625000614517592, 3.027376345333613106, -5.243569643749998122 ) ) ;
#20671 = CARTESIAN_POINT ( 'NONE',  ( 2.000000000000001332, 13.06250000122903465, -26.53589838486224650 ) ) ;
#20672 = CARTESIAN_POINT ( 'NONE',  ( -1.071796769724488563, 13.79240381056766829, -26.00000000000000000 ) ) ;
#20673 = AXIS2_PLACEMENT_3D ( 'NONE', #27458, #10098, #15989 ) ;
#20674 = CARTESIAN_POINT ( 'NONE',  ( 9.674999999999998934, 4.330127018922191873, 2.499999999999999556 ) ) ;
#20675 = CARTESIAN_POINT ( 'NONE',  ( 10.99687500061451750, -3.027376345333614438, 5.243569643749998122 ) ) ;
#20676 = CARTESIAN_POINT ( 'NONE',  ( 6.225000001229036073, 2.886751345948126879, 4.999999999999999112 ) ) ;
#20677 = CARTESIAN_POINT ( 'NONE',  ( 13.54687500061451999, 6.054752690667223547, 3.707466751127219781E-16 ) ) ;
#20678 = CARTESIAN_POINT ( 'NONE',  ( 15.37500000000000000, 6.123233995736764310E-16, -4.999999999999998224 ) ) ;
#20679 = CARTESIAN_POINT ( 'NONE',  ( 6.159375000614517148, -4.541064518000417216, -2.621784821875001281 ) ) ;
#20680 = FACE_OUTER_BOUND ( 'NONE', #59290, .T. ) ;
#20681 = CARTESIAN_POINT ( 'NONE',  ( 13.20937500061451786, 0.000000000000000000, 5.243569643749999010 ) ) ;
#20682 = DIRECTION ( 'NONE',  ( 0.000000000000000000, 0.000000000000000000, -1.000000000000000000 ) ) ;
#20683 = CARTESIAN_POINT ( 'NONE',  ( 21.06562500061451715, 3.027376345333613106, -5.243569643749998122 ) ) ;
#20684 = CARTESIAN_POINT ( 'NONE',  ( 30.00000000000000000, 6.123233995736764310E-16, -4.999999999999998224 ) ) ;
#20685 = CARTESIAN_POINT ( 'NONE',  ( 1.626862140677534273E-15, 16.51249999999999929, 34.00000000000000000 ) ) ;
#20686 = CARTESIAN_POINT ( 'NONE',  ( 23.89687500061451786, 6.054752690667223547, 3.707466751127219781E-16 ) ) ;
#20687 = CARTESIAN_POINT ( 'NONE',  ( 1.626862140677534273E-15, 13.92500000122903181, -26.00000000000000355 ) ) ;
#20688 = CARTESIAN_POINT ( 'NONE',  ( 4.640625000614518214, -3.027376345333614438, 5.243569643749998122 ) ) ;
#20689 = CARTESIAN_POINT ( 'NONE',  ( 23.22187500061451360, 5.824947211148865298E-16, -4.756430356249998326 ) ) ;
#20690 = CARTESIAN_POINT ( 'NONE',  ( 18.47812500061451857, 4.541064518000418104, 2.621784821874999949 ) ) ;
#20691 = CARTESIAN_POINT ( 'NONE',  ( 15.42187500061451821, 3.027376345333611329, 5.243569643749999010 ) ) ;
#20692 = CARTESIAN_POINT ( 'NONE',  ( 29.81250000000000000, 2.886751345948129099, -4.999999999999998224 ) ) ;
#20693 = CARTESIAN_POINT ( 'NONE',  ( 26.21250000122903501, -4.330127018922190985, -2.500000000000001332 ) ) ;
#20694 = CARTESIAN_POINT ( 'NONE',  ( 6.496875000614517504, -3.027376345333614438, 5.243569643749998122 ) ) ;
#20695 = CARTESIAN_POINT ( 'NONE',  ( 16.28437500061452070, 4.541064518000418104, 2.621784821874999949 ) ) ;
#20696 = FACE_OUTER_BOUND ( 'NONE', #19058, .T. ) ;
#20697 = CARTESIAN_POINT ( 'NONE',  ( 24.48749999999999716, 5.773502691896255534, 3.535250795749688894E-16 ) ) ;
#20698 = CARTESIAN_POINT ( 'NONE',  ( 3.225000001229033408, -5.773502691896255534, -1.060575238724906372E-15 ) ) ;
#20699 = CARTESIAN_POINT ( 'NONE',  ( 27.15937500061451360, 0.000000000000000000, 5.243569643749999010 ) ) ;
#20700 = CARTESIAN_POINT ( 'NONE',  ( 17.33437500061451431, -4.541064518000419881, 2.621784821874995952 ) ) ;
#20701 = CARTESIAN_POINT ( 'NONE',  ( 1.878215178125000495, 13.27812499938548285, 26.74683588394047007 ) ) ;
#20702 = CARTESIAN_POINT ( 'NONE',  ( 30.00000000000000000, 0.000000000000000000, 4.999999999999998224 ) ) ;
#20703 = CARTESIAN_POINT ( 'NONE',  ( 8.250000000000000000, 4.330127018922192761, -2.499999999999997780 ) ) ;
#20704 = CARTESIAN_POINT ( 'NONE',  ( 9.346875000614517148, 4.119189519843966529, -2.378215178124998275 ) ) ;
#20705 = CARTESIAN_POINT ( 'NONE',  ( 20.20312500061451644, 4.541064518000418104, -2.621784821874998173 ) ) ;
#20706 = CARTESIAN_POINT ( 'NONE',  ( 8.287499999999999645, 5.773502691896255534, 3.535250795749688894E-16 ) ) ;
#20707 = EDGE_CURVE ( 'NONE', #3090, #2356, #773, .T. ) ;
#20708 = CARTESIAN_POINT ( 'NONE',  ( 4.528125000614516615, 4.541064518000418104, 2.621784821874999949 ) ) ;
#20709 = CARTESIAN_POINT ( 'NONE',  ( 18.52499999999999858, 6.123233995736764310E-16, -4.999999999999998224 ) ) ;
#20710 = CARTESIAN_POINT ( 'NONE',  ( 17.54062500061451502, 6.054752690667223547, 3.707466751127219781E-16 ) ) ;
#20711 = CARTESIAN_POINT ( 'NONE',  ( 22.95000000122903216, -2.886751345948129988, 4.999999999999997335 ) ) ;
#20712 = CARTESIAN_POINT ( 'NONE',  ( 6.000084452983056593, 7.999936660264885369, 29.59830633522030396 ) ) ;
#20713 = CARTESIAN_POINT ( 'NONE',  ( 29.63437500061451502, 6.421520780324663323E-16, -5.243569643749999010 ) ) ;
#20714 = CIRCLE ( 'NONE', #62022, 1.500000000000000666 ) ;
#20715 = VERTEX_POINT ( 'NONE', #62402 ) ;
#20716 = CARTESIAN_POINT ( 'NONE',  ( 16.94062500061451715, -3.027376345333610441, -5.243569643749999898 ) ) ;
#20717 = CARTESIAN_POINT ( 'NONE',  ( 24.85312500061451502, 0.000000000000000000, 5.243569643749999010 ) ) ;
#20718 = CARTESIAN_POINT ( 'NONE',  ( 25.20937500061451431, 4.541064518000418104, -2.621784821874998173 ) ) ;
#20719 = CARTESIAN_POINT ( 'NONE',  ( 8.362500000000002487, 2.886751345948126879, 4.999999999999999112 ) ) ;
#20720 = CARTESIAN_POINT ( 'NONE',  ( 11.05312500061451608, -4.541064518000417216, -2.621784821875001281 ) ) ;
#20721 = CARTESIAN_POINT ( 'NONE',  ( 26.05312500061451431, 4.541064518000418104, -2.621784821874998173 ) ) ;
#20722 = CARTESIAN_POINT ( 'NONE',  ( 16.88437500061451502, -4.541064518000419881, 2.621784821874995952 ) ) ;
#20723 = CARTESIAN_POINT ( 'NONE',  ( 9.478125000614515017, 4.541064518000418104, 2.621784821874999949 ) ) ;
#20724 = CARTESIAN_POINT ( 'NONE',  ( 7.087500001229034119, 4.330127018922191873, 2.499999999999999556 ) ) ;
#20725 = CARTESIAN_POINT ( 'NONE',  ( -2.121784821874999949, 19.72812500061451857, 26.32496088578401938 ) ) ;
#20726 = CARTESIAN_POINT ( 'NONE',  ( 23.36250000122903359, 0.000000000000000000, 4.999999999999998224 ) ) ;
#20727 = CARTESIAN_POINT ( 'NONE',  ( 16.05937500061451573, -4.119189519843965641, -2.378215178125001383 ) ) ;
#20728 = CARTESIAN_POINT ( 'NONE',  ( 14.87812500061451537, 4.541064518000418104, 2.621784821874999949 ) ) ;
#20729 = CARTESIAN_POINT ( 'NONE',  ( 8.559375000614515727, 4.541064518000418104, -2.621784821874998173 ) ) ;
#20730 = CARTESIAN_POINT ( 'NONE',  ( 6.046875000614519102, -3.027376345333614438, 5.243569643749998122 ) ) ;
#20731 = ORIENTED_EDGE ( 'NONE', *, *, #41134, .T. ) ;
#20732 = CARTESIAN_POINT ( 'NONE',  ( 3.999999999999999112, 13.47500000000000142, 30.00000000000000000 ) ) ;
#20733 = CARTESIAN_POINT ( 'NONE',  ( 18.36562500061451431, 3.027376345333613106, -5.243569643749998122 ) ) ;
#20734 = AXIS2_PLACEMENT_3D ( 'NONE', #3081, #25609, #52594 ) ;
#20735 = CARTESIAN_POINT ( 'NONE',  ( 15.60937500061451644, -4.541064518000417216, -2.621784821875001281 ) ) ;
#20736 = CARTESIAN_POINT ( 'NONE',  ( 19.22812500061451502, 6.421520780324663323E-16, -5.243569643749999010 ) ) ;
#20737 = CARTESIAN_POINT ( 'NONE',  ( 2.000000000000001332, 12.95000000000000107, 33.46410161513774995 ) ) ;
#20738 = CARTESIAN_POINT ( 'NONE',  ( 27.89062500061451289, 6.054752690667223547, 3.707466751127219781E-16 ) ) ;
#20739 = CARTESIAN_POINT ( 'NONE',  ( 6.937500001229033764, 6.123233995736764310E-16, -4.999999999999998224 ) ) ;
#20740 = AXIS2_PLACEMENT_3D ( 'NONE', #22253, #5266, #38525 ) ;
#20741 = ORIENTED_EDGE ( 'NONE', *, *, #24238, .T. ) ;
#20742 = CARTESIAN_POINT ( 'NONE',  ( 2.700000001229035718, -2.886751345948129988, 4.999999999999997335 ) ) ;
#20743 = CARTESIAN_POINT ( 'NONE',  ( -1.999999999999997113, 17.37500000000000000, -26.53589838486224295 ) ) ;
#20744 = CARTESIAN_POINT ( 'NONE',  ( 21.82500000122903572, 2.886751345948129099, -4.999999999999998224 ) ) ;
#20745 = CARTESIAN_POINT ( 'NONE',  ( -3.756430356250001434, 14.36562499938548143, 32.16877607737301048 ) ) ;
#20746 = CARTESIAN_POINT ( 'NONE',  ( 6.459375000614518747, 0.000000000000000000, 5.243569643749999010 ) ) ;
#20747 = CARTESIAN_POINT ( 'NONE',  ( 1.071796769724484344, 15.18259618943233669, 34.00000000000000000 ) ) ;
#20748 = CARTESIAN_POINT ( 'NONE',  ( 12.62812500061451537, 4.541064518000418104, 2.621784821874999949 ) ) ;
#20749 = CARTESIAN_POINT ( 'NONE',  ( 7.584375000614516082, 6.421520780324663323E-16, -5.243569643749999010 ) ) ;
#20750 = CARTESIAN_POINT ( 'NONE',  ( 27.07500000122903216, -5.773502691896255534, -1.060575238724906372E-15 ) ) ;
#20751 = CARTESIAN_POINT ( 'NONE',  ( 18.42187500061451999, 3.027376345333612662, -5.243569643749998122 ) ) ;
#20752 = CARTESIAN_POINT ( 'NONE',  ( 4.321875000614517681, -6.054752690667223547, -1.112240025338166033E-15 ) ) ;
#20753 = CARTESIAN_POINT ( 'NONE',  ( -3.999999999999999112, 11.00000000000000178, 30.00000000000000000 ) ) ;
#20754 = CARTESIAN_POINT ( 'NONE',  ( 6.028125000614517504, -4.541064518000419881, 2.621784821874995952 ) ) ;
#20755 = CARTESIAN_POINT ( 'NONE',  ( 14.80312500061451608, 4.541064518000418104, -2.621784821874998173 ) ) ;
#20756 = VERTEX_POINT ( 'NONE', #35051 ) ;
#20757 = CARTESIAN_POINT ( 'NONE',  ( 12.10312500061451857, 4.541064518000418104, -2.621784821874998173 ) ) ;
#20758 = CARTESIAN_POINT ( 'NONE',  ( 5.737500001229033586, 4.330127018922191873, 2.499999999999999556 ) ) ;
#20759 = CARTESIAN_POINT ( 'NONE',  ( 8.165625000614516793, 3.027376345333611329, 5.243569643749999010 ) ) ;
#20760 = CARTESIAN_POINT ( 'NONE',  ( 21.53437500061451715, 5.824947211148865298E-16, -4.756430356249998326 ) ) ;
#20761 = CARTESIAN_POINT ( 'NONE',  ( 9.262499999999999289, 2.886751345948126879, 4.999999999999999112 ) ) ;
#20762 = EDGE_CURVE ( 'NONE', #47145, #28470, #5172, .T. ) ;
#20763 = CARTESIAN_POINT ( 'NONE',  ( 5.100000001229034297, -2.886751345948125991, -5.000000000000000000 ) ) ;
#20764 = CARTESIAN_POINT ( 'NONE',  ( 16.87500000000000000, 4.330127018922191873, 2.499999999999999556 ) ) ;
#20765 = CARTESIAN_POINT ( 'NONE',  ( 17.33437500061451431, -4.541064518000419881, 2.621784821874995952 ) ) ;
#20766 = CARTESIAN_POINT ( 'NONE',  ( 14.62500000122903288, 2.886751345948129099, -4.999999999999998224 ) ) ;
#20767 = CARTESIAN_POINT ( 'NONE',  ( 23.17500000000000071, 4.330127018922191873, 2.499999999999999556 ) ) ;
#20768 = CIRCLE ( 'NONE', #24308, 4.000000000000000000 ) ;
#20769 = CARTESIAN_POINT ( 'NONE',  ( -2.121784821874999949, 16.12812500061451715, -33.67503911421598417 ) ) ;
#20770 = CARTESIAN_POINT ( 'NONE',  ( -1.626862140677534273E-15, 20.03749999999999787, 34.00000000000000000 ) ) ;
#20771 = CARTESIAN_POINT ( 'NONE',  ( -1.071796769724491671, 13.47634618820330132, 26.00000000000000355 ) ) ;
#20772 = CARTESIAN_POINT ( 'NONE',  ( 18.95625000122903003, -4.330127018922190985, -2.500000000000001332 ) ) ;
#20773 = DIRECTION ( 'NONE',  ( -1.000000000000000000, -0.000000000000000000, -0.000000000000000000 ) ) ;
#20774 = DIRECTION ( 'NONE',  ( 0.000000000000000000, 0.000000000000000000, 1.000000000000000000 ) ) ;
#20775 = CARTESIAN_POINT ( 'NONE',  ( 16.58437500061451786, 6.421520780324663323E-16, -5.243569643749999010 ) ) ;
#20776 = CARTESIAN_POINT ( 'NONE',  ( 26.66250000000000142, 2.886751345948129099, -4.999999999999998224 ) ) ;
#20777 = CARTESIAN_POINT ( 'NONE',  ( 12.74062500061451786, -3.027376345333614438, 5.243569643749998122 ) ) ;
#20778 = CARTESIAN_POINT ( 'NONE',  ( 8.081250001229031810, -4.330127018922194537, 2.499999999999995559 ) ) ;
#20779 = PRODUCT_DEFINITION_SHAPE ( 'NONE', 'NONE',  #73123 ) ;
#20780 = CARTESIAN_POINT ( 'NONE',  ( 22.28437500061451715, -4.541064518000419881, 2.621784821874995952 ) ) ;
#20781 = CARTESIAN_POINT ( 'NONE',  ( 13.28437500061451537, -2.746126346562641984, -4.756430356249999214 ) ) ;
#20782 = CARTESIAN_POINT ( 'NONE',  ( 8.465625000614515727, 3.027376345333613106, -5.243569643749998122 ) ) ;
#20783 = CARTESIAN_POINT ( 'NONE',  ( 13.69687500061451679, -3.027376345333614438, 5.243569643749998122 ) ) ;
#20784 = ORIENTED_EDGE ( 'NONE', *, *, #420, .T. ) ;
#20785 = CARTESIAN_POINT ( 'NONE',  ( 23.37187500061451573, 3.027376345333613106, -5.243569643749998122 ) ) ;
#20786 = CARTESIAN_POINT ( 'NONE',  ( 27.02812500061451573, 4.541064518000418104, 2.621784821874999949 ) ) ;
#20787 = LINE ( 'NONE', #43344, #71482 ) ;
#20788 =( BOUNDED_CURVE ( )  B_SPLINE_CURVE ( 3, ( #47573, #8777, #64560, #31312 ),
 .UNSPECIFIED., .F., .F. ) 
 B_SPLINE_CURVE_WITH_KNOTS ( ( 4, 4 ),
 ( 3.141592653589793116, 4.712388980384689674 ),
 .UNSPECIFIED. ) 
 CURVE ( )  GEOMETRIC_REPRESENTATION_ITEM ( )  RATIONAL_B_SPLINE_CURVE ( ( 1.000000000000000000, 0.8047378541243649375, 0.8047378541243649375, 1.000000000000000000 ) ) 
 REPRESENTATION_ITEM ( '' )  );
#20789 = CARTESIAN_POINT ( 'NONE',  ( 8.212500000000000355, 2.886751345948129099, -4.999999999999998224 ) ) ;
#20790 = CARTESIAN_POINT ( 'NONE',  ( 17.47500000122903430, 2.886751345948126879, 4.999999999999999112 ) ) ;
#20791 = CARTESIAN_POINT ( 'NONE',  ( -3.999999999999999112, 19.83124999877096784, 27.69059892324149530 ) ) ;
#20792 = CARTESIAN_POINT ( 'NONE',  ( 8.896875000614517859, 4.119189519843966529, -2.378215178124998275 ) ) ;
#20793 = ORIENTED_EDGE ( 'NONE', *, *, #28153, .F. ) ;
#20794 = EDGE_CURVE ( 'NONE', #72010, #31518, #57579, .T. ) ;
#20795 = CARTESIAN_POINT ( 'NONE',  ( 15.63749999999999751, -2.886751345948129988, 4.999999999999997335 ) ) ;
#20796 = CARTESIAN_POINT ( 'NONE',  ( 17.92500000000000071, -4.330127018922194537, 2.499999999999995559 ) ) ;
#20797 = CARTESIAN_POINT ( 'NONE',  ( 10.45312500061451644, 0.000000000000000000, 5.243569643749999010 ) ) ;
#20798 = ORIENTED_EDGE ( 'NONE', *, *, #21398, .T. ) ;
#20799 = FACE_OUTER_BOUND ( 'NONE', #45469, .T. ) ;
#20800 = CARTESIAN_POINT ( 'NONE',  ( 4.243569643749999898, 16.93437500061451573, -30.00000000000000000 ) ) ;
#20801 = CARTESIAN_POINT ( 'NONE',  ( 2.990625000614519191, -3.027376345333610441, -5.243569643749999898 ) ) ;
#20802 = CARTESIAN_POINT ( 'NONE',  ( -4.000000000000000000, 14.07500000000000107, 30.00000000000000000 ) ) ;
#20803 = CARTESIAN_POINT ( 'NONE',  ( 9.637499999999999289, 5.773502691896255534, 3.535250795749688894E-16 ) ) ;
#20804 = FACE_OUTER_BOUND ( 'NONE', #2453, .T. ) ;
#20805 = ORIENTED_EDGE ( 'NONE', *, *, #26971, .F. ) ;
#20806 = CARTESIAN_POINT ( 'NONE',  ( -2.121784821874999949, 13.42812500061451786, 26.32496088578401938 ) ) ;
#20807 = CARTESIAN_POINT ( 'NONE',  ( 25.75312500061451715, 0.000000000000000000, 5.243569643749999010 ) ) ;
#20808 = AXIS2_PLACEMENT_3D ( 'NONE', #22983, #63866, #58684 ) ;
#20809 = CARTESIAN_POINT ( 'NONE',  ( 30.00000000000000000, 0.000000000000000000, 0.000000000000000000 ) ) ;
#20810 = CARTESIAN_POINT ( 'NONE',  ( 20.22187500061451715, 3.027376345333613106, -5.243569643749998122 ) ) ;
#20811 = CARTESIAN_POINT ( 'NONE',  ( 19.97812500061451502, -4.541064518000419881, 2.621784821874995952 ) ) ;
#20812 = CARTESIAN_POINT ( 'NONE',  ( -4.243569643749999898, 13.91562500061459495, -32.45002607614398471 ) ) ;
#20813 = CARTESIAN_POINT ( 'NONE',  ( 22.31250000122903288, 4.330127018922192761, -2.499999999999997780 ) ) ;
#20814 = CARTESIAN_POINT ( 'NONE',  ( 5.165625000614518569, -6.054752690667223547, -1.112240025338166033E-15 ) ) ;
#20815 = CARTESIAN_POINT ( 'NONE',  ( 23.74687500061451573, -2.746126346562641984, -4.756430356249999214 ) ) ;
#20816 = CARTESIAN_POINT ( 'NONE',  ( 21.17812500061451431, 4.541064518000418104, 2.621784821874999949 ) ) ;
#20817 = DIRECTION ( 'NONE',  ( 0.000000000000000000, 0.000000000000000000, 1.000000000000000000 ) ) ;
#20818 = CARTESIAN_POINT ( 'NONE',  ( -7.967954043666661671E-16, 16.57812499938548356, 34.33755215474603517 ) ) ;
#20819 = CARTESIAN_POINT ( 'NONE',  ( 15.38437500061451679, 4.541064518000418104, 2.621784821874999949 ) ) ;
#20820 = CARTESIAN_POINT ( 'NONE',  ( 14.18437500061451750, -4.541064518000419881, 2.621784821874995952 ) ) ;
#20821 = CARTESIAN_POINT ( 'NONE',  ( 24.19687500061451857, -3.027376345333610441, -5.243569643749999898 ) ) ;
#20822 = CARTESIAN_POINT ( 'NONE',  ( -4.243569643749998122, 12.24687500061451750, 32.45002607614398471 ) ) ;
#20823 = CARTESIAN_POINT ( 'NONE',  ( 4.340625000614515727, -3.027376345333610441, -5.243569643749999898 ) ) ;
#20824 = CARTESIAN_POINT ( 'NONE',  ( 28.45312500061451289, 0.000000000000000000, 5.243569643749999010 ) ) ;
#20825 =( BOUNDED_CURVE ( )  B_SPLINE_CURVE ( 2, ( #48628, #71528, #65979, #15359, #60419, #52075, #2459 ),
 .UNSPECIFIED., .F., .F. ) 
 B_SPLINE_CURVE_WITH_KNOTS ( ( 3, 2, 2, 3 ),
 ( 0.8900000000000000133, 0.8933333333333333126, 0.8966666666666666119, 0.9000000000000000222 ),
 .UNSPECIFIED. ) 
 CURVE ( )  GEOMETRIC_REPRESENTATION_ITEM ( )  RATIONAL_B_SPLINE_CURVE ( ( 1.000000000000000000, 0.8660254037844387076, 1.000000000000000000, 0.8660254037844387076, 1.000000000000000000, 0.8660254037844387076, 1.000000000000000000 ) ) 
 REPRESENTATION_ITEM ( '' )  );
#20826 = CARTESIAN_POINT ( 'NONE',  ( 29.16562500061451502, 3.027376345333613106, -5.243569643749998122 ) ) ;
#20827 = CARTESIAN_POINT ( 'NONE',  ( -1.243387493232115393E-14, 15.31250000000000000, 26.00000000000000000 ) ) ;
#20828 = CARTESIAN_POINT ( 'NONE',  ( -2.828200636599751609E-16, 18.08750000000000213, 25.38119784648299770 ) ) ;
#20829 = AXIS2_PLACEMENT_3D ( 'NONE', #55856, #51396, #5965 ) ;
#20830 = CARTESIAN_POINT ( 'NONE',  ( 8.109375000614518214, 4.541064518000418104, -2.621784821874998173 ) ) ;
#20831 = APPLICATION_PROTOCOL_DEFINITION ( 'draft international standard', 'automotive_design', 1998, #4977 ) ;
#20832 = CARTESIAN_POINT ( 'NONE',  ( 13.87500000122903465, 2.886751345948126879, 4.999999999999999112 ) ) ;
#20833 = CARTESIAN_POINT ( 'NONE',  ( 9.225000001229034297, 2.886751345948129099, -4.999999999999998224 ) ) ;
#20834 = CARTESIAN_POINT ( 'NONE',  ( 5.878125000614517148, 4.541064518000418104, 2.621784821874999949 ) ) ;
#20835 = CARTESIAN_POINT ( 'NONE',  ( 2.828200636599751609E-16, 17.05624999877096570, 25.38119784648299415 ) ) ;
#20836 = CARTESIAN_POINT ( 'NONE',  ( 18.54375000122902861, -2.886751345948125991, -5.000000000000000000 ) ) ;
#20837 = CARTESIAN_POINT ( 'NONE',  ( 14.55937500061451573, 0.000000000000000000, 5.243569643749999010 ) ) ;
#20838 = CARTESIAN_POINT ( 'NONE',  ( 4.000000000000000000, 17.60000000122903430, 32.30940107675849760 ) ) ;
#20839 = ORIENTED_EDGE ( 'NONE', *, *, #44780, .T. ) ;
#20840 = CARTESIAN_POINT ( 'NONE',  ( 21.25312500061451715, 0.000000000000000000, 5.243569643749999010 ) ) ;
#20841 = CARTESIAN_POINT ( 'NONE',  ( 6.853125000614516793, 0.000000000000000000, 5.243569643749999010 ) ) ;
#20842 = CARTESIAN_POINT ( 'NONE',  ( 25.20937500061451431, 4.541064518000418104, -2.621784821874998173 ) ) ;
#20843 = CARTESIAN_POINT ( 'NONE',  ( 7.828125000614517326, -4.541064518000419881, 2.621784821874995952 ) ) ;
#20844 = CARTESIAN_POINT ( 'NONE',  ( 20.99999999999999645, 0.000000000000000000, 4.999999999999998224 ) ) ;
#20845 = CARTESIAN_POINT ( 'NONE',  ( 8.925000001229033586, 2.886751345948126879, 4.999999999999999112 ) ) ;
#20846 = CARTESIAN_POINT ( 'NONE',  ( 22.79062500061451502, -3.027376345333610441, -5.243569643749999898 ) ) ;
#20847 = CARTESIAN_POINT ( 'NONE',  ( 3.999999999999998668, 19.02500000122903501, -32.30940107675850470 ) ) ;
#20848 = CARTESIAN_POINT ( 'NONE',  ( 11.40000000122903501, -2.886751345948125991, -5.000000000000000000 ) ) ;
#20849 =( BOUNDED_CURVE ( )  B_SPLINE_CURVE ( 1, ( #30562, #25378 ),
 .UNSPECIFIED., .F., .F. ) 
 B_SPLINE_CURVE_WITH_KNOTS ( ( 2, 2 ),
 ( 0.000000000000000000, 1.000000000000000000 ),
 .UNSPECIFIED. ) 
 CURVE ( )  GEOMETRIC_REPRESENTATION_ITEM ( )  RATIONAL_B_SPLINE_CURVE ( ( 0.9401542295230078672, 0.9401542295230078672 ) ) 
 REPRESENTATION_ITEM ( '' )  );
#20850 = CARTESIAN_POINT ( 'NONE',  ( 19.64062500061451644, -3.027376345333610441, -5.243569643749999898 ) ) ;
#20851 = CARTESIAN_POINT ( 'NONE',  ( 16.37812500061451715, -4.541064518000419881, 2.621784821874995952 ) ) ;
#20852 = CARTESIAN_POINT ( 'NONE',  ( 29.25937500061451502, 4.119189519843966529, -2.378215178124998275 ) ) ;
#20853 = CARTESIAN_POINT ( 'NONE',  ( 16.68750000000000000, -2.886751345948125991, -5.000000000000000000 ) ) ;
#20854 = CARTESIAN_POINT ( 'NONE',  ( 10.46250000122903323, -4.330127018922190985, -2.500000000000001332 ) ) ;
#20855 = CARTESIAN_POINT ( 'NONE',  ( 7.415625000614516793, -6.054752690667223547, -1.112240025338166033E-15 ) ) ;
#20856 = CARTESIAN_POINT ( 'NONE',  ( 11.16562500061451679, 3.027376345333613106, -5.243569643749998122 ) ) ;
#20857 = EDGE_CURVE ( 'NONE', #44824, #18463, #50224, .T. ) ;
#20858 = CARTESIAN_POINT ( 'NONE',  ( 24.45000000122903572, -2.886751345948125991, -5.000000000000000000 ) ) ;
#20859 = CARTESIAN_POINT ( 'NONE',  ( 19.28437500061451360, 6.421520780324663323E-16, -5.243569643749999010 ) ) ;
#20860 = CARTESIAN_POINT ( 'NONE',  ( 22.18125000122903145, 6.123233995736764310E-16, -4.999999999999998224 ) ) ;
#20861 = AXIS2_PLACEMENT_3D ( 'NONE', #7674, #36114, #47205 ) ;
#20862 = AXIS2_PLACEMENT_3D ( 'NONE', #64200, #1445, #52040 ) ;
#20863 = CARTESIAN_POINT ( 'NONE',  ( 4.237500001229036251, 6.123233995736764310E-16, -4.999999999999998224 ) ) ;
#20864 = CARTESIAN_POINT ( 'NONE',  ( 4.584375000614516971, 4.541064518000418104, 2.621784821874999949 ) ) ;
#20865 = CARTESIAN_POINT ( 'NONE',  ( 22.39687500061451075, -3.027376345333610441, -5.243569643749999898 ) ) ;
#20866 = CARTESIAN_POINT ( 'NONE',  ( 10.53750000000000320, 5.773502691896255534, 3.535250795749688401E-16 ) ) ;
#20867 = CARTESIAN_POINT ( 'NONE',  ( 19.07812500061451644, -4.541064518000419881, 2.621784821874995952 ) ) ;
#20868 = CARTESIAN_POINT ( 'NONE',  ( 23.93437500061451573, 4.541064518000418104, 2.621784821874999949 ) ) ;
#20869 = CARTESIAN_POINT ( 'NONE',  ( -0.6941636114358130660, 20.72676549290719450, 33.93677660682192965 ) ) ;
#20870 = CARTESIAN_POINT ( 'NONE',  ( -1.071796769724490339, 14.43259618943233313, 26.00000000000000000 ) ) ;
#20871 = CARTESIAN_POINT ( 'NONE',  ( 27.83437500061451786, 6.421520780324663323E-16, -5.243569643749999010 ) ) ;
#20872 = CARTESIAN_POINT ( 'NONE',  ( 6.534375000614517148, -4.541064518000419881, 2.621784821874995952 ) ) ;
#20873 = CARTESIAN_POINT ( 'NONE',  ( 15.74062500061451608, 6.054752690667223547, 3.707466751127219781E-16 ) ) ;
#20874 = CARTESIAN_POINT ( 'NONE',  ( 12.49687500061451573, -3.027376345333610441, -5.243569643749999898 ) ) ;
#20875 = ORIENTED_EDGE ( 'NONE', *, *, #15762, .F. ) ;
#20876 = DIRECTION ( 'NONE',  ( -1.000000000000000000, -0.000000000000000000, -0.000000000000000000 ) ) ;
#20877 = CARTESIAN_POINT ( 'NONE',  ( 25.86562500061451431, -6.054752690667223547, -1.112240025338166033E-15 ) ) ;
#20878 = CARTESIAN_POINT ( 'NONE',  ( 9.356250001229033941, 0.000000000000000000, 4.999999999999998224 ) ) ;
#20879 = CARTESIAN_POINT ( 'NONE',  ( 14.13750000000000107, 5.773502691896255534, 3.535250795749688894E-16 ) ) ;
#20880 = CARTESIAN_POINT ( 'NONE',  ( 24.11250000122903359, 4.330127018922192761, -2.499999999999997780 ) ) ;
#20881 = CARTESIAN_POINT ( 'NONE',  ( 18.32812500061451644, 6.421520780324663323E-16, -5.243569643749999010 ) ) ;
#20882 = ORIENTED_EDGE ( 'NONE', *, *, #32902, .F. ) ;
#20883 = CARTESIAN_POINT ( 'NONE',  ( 22.64999999999999858, 4.330127018922192761, -2.499999999999997780 ) ) ;
#20884 = CARTESIAN_POINT ( 'NONE',  ( 25.02187500061451431, -6.054752690667223547, -1.112240025338166033E-15 ) ) ;
#20885 = EDGE_CURVE ( 'NONE', #62607, #60454, #11550, .T. ) ;
#20886 = VERTEX_POINT ( 'NONE', #53128 ) ;
#20887 = CARTESIAN_POINT ( 'NONE',  ( 10.64062500061451644, -3.027376345333610441, -5.243569643749999898 ) ) ;
#20888 = CARTESIAN_POINT ( 'NONE',  ( 4.078125000614517326, 4.541064518000418104, 2.621784821874999949 ) ) ;
#20889 = CARTESIAN_POINT ( 'NONE',  ( 13.24687500061451750, -4.119189519843965641, -2.378215178125001383 ) ) ;
#20890 = CARTESIAN_POINT ( 'NONE',  ( 26.42812500061451431, 6.421520780324663323E-16, -5.243569643749999010 ) ) ;
#20891 = CARTESIAN_POINT ( 'NONE',  ( 17.25000000000000000, 4.330127018922192761, -2.499999999999997780 ) ) ;
#20892 = CARTESIAN_POINT ( 'NONE',  ( 25.46249999999999858, 2.886751345948126879, 4.999999999999999112 ) ) ;
#20893 = CARTESIAN_POINT ( 'NONE',  ( -3.000416591977282496E-16, 19.69062500061451360, 25.09994784771203058 ) ) ;
#20894 = CARTESIAN_POINT ( 'NONE',  ( 7.584375000614516082, 6.421520780324663323E-16, -5.243569643749999010 ) ) ;
#20895 = CARTESIAN_POINT ( 'NONE',  ( 16.73437500061451644, 4.541064518000418104, 2.621784821874999949 ) ) ;
#20896 = CARTESIAN_POINT ( 'NONE',  ( 28.69687500061451502, -3.027376345333610441, -5.243569643749999898 ) ) ;
#20897 = ORIENTED_EDGE ( 'NONE', *, *, #9282, .T. ) ;
#20898 = CARTESIAN_POINT ( 'NONE',  ( 26.05312500061451431, 4.541064518000418104, -2.621784821874998173 ) ) ;
#20899 = CARTESIAN_POINT ( 'NONE',  ( 28.02187500061451431, 3.027376345333611329, 5.243569643749999010 ) ) ;
#20900 = CARTESIAN_POINT ( 'NONE',  ( 0.000000000000000000, 20.00000000000000000, -30.00000000000000000 ) ) ;
#20901 = CARTESIAN_POINT ( 'NONE',  ( 14.10000000000000142, 4.330127018922192761, -2.499999999999997780 ) ) ;
#20902 = CARTESIAN_POINT ( 'NONE',  ( 10.26562500061451644, 3.027376345333613106, -5.243569643749998122 ) ) ;
#20903 = CARTESIAN_POINT ( 'NONE',  ( 15.28125000122903288, -4.330127018922194537, 2.499999999999995559 ) ) ;
#20904 = LINE ( 'NONE', #19803, #19468 ) ;
#20905 = CARTESIAN_POINT ( 'NONE',  ( 29.31562500061451715, 3.027376345333611329, 5.243569643749999010 ) ) ;
#20906 = CARTESIAN_POINT ( 'NONE',  ( 15.52500000122903323, 2.886751345948129099, -4.999999999999998224 ) ) ;
#20907 = DIRECTION ( 'NONE',  ( -0.000000000000000000, -1.000000000000000000, -0.000000000000000000 ) ) ;
#20908 = CARTESIAN_POINT ( 'NONE',  ( 15.83437500061451608, 4.119189519843966529, 2.378215178124999607 ) ) ;
#20909 = CARTESIAN_POINT ( 'NONE',  ( 5.203125000614518214, -4.541064518000417216, -2.621784821875001281 ) ) ;
#20910 = CARTESIAN_POINT ( 'NONE',  ( 20.82187500061451857, 3.027376345333611329, 5.243569643749999010 ) ) ;
#20911 = CARTESIAN_POINT ( 'NONE',  ( -4.243569643749999898, 17.57187500061451502, 27.54997392385601529 ) ) ;
#20912 = CARTESIAN_POINT ( 'NONE',  ( 20.78437500061451715, 4.541064518000418104, 2.621784821874999949 ) ) ;
#20913 = CARTESIAN_POINT ( 'NONE',  ( 4.200000000000001954, 4.330127018922192761, -2.499999999999997780 ) ) ;
#20914 = CARTESIAN_POINT ( 'NONE',  ( -3.999999999999997335, 9.800000001229033586, 32.30940107675850470 ) ) ;
#20915 = CARTESIAN_POINT ( 'NONE',  ( 12.10312500061451857, 4.541064518000418104, -2.621784821874998173 ) ) ;
#20916 = CARTESIAN_POINT ( 'NONE',  ( 4.612500001229032698, -4.330127018922190985, -2.500000000000001332 ) ) ;
#20917 = CARTESIAN_POINT ( 'NONE',  ( 9.496875000614517504, 6.054752690667223547, 3.707466751127219781E-16 ) ) ;
#20918 = CARTESIAN_POINT ( 'NONE',  ( 12.95625000122903359, 0.000000000000000000, 4.999999999999998224 ) ) ;
#20919 = CARTESIAN_POINT ( 'NONE',  ( 9.103125000614515017, 0.000000000000000000, 5.243569643749999010 ) ) ;
#20920 = CARTESIAN_POINT ( 'NONE',  ( 14.52187500061451608, 3.027376345333611329, 5.243569643749999010 ) ) ;
#20921 = CARTESIAN_POINT ( 'NONE',  ( 21.73125000122903216, 6.123233995736764310E-16, -4.999999999999998224 ) ) ;
#20922 = CARTESIAN_POINT ( 'NONE',  ( 20.88750000122903572, 6.123233995736764310E-16, -4.999999999999998224 ) ) ;
#20923 = CARTESIAN_POINT ( 'NONE',  ( 9.871875000614517504, 3.027376345333613106, -5.243569643749998122 ) ) ;
#20924 = CARTESIAN_POINT ( 'NONE',  ( 13.11562500061451786, 3.027376345333611329, 5.243569643749999010 ) ) ;
#20925 = CARTESIAN_POINT ( 'NONE',  ( 26.53125000122902932, -4.330127018922194537, 2.499999999999995559 ) ) ;
#20926 = CARTESIAN_POINT ( 'NONE',  ( 22.69687500061451857, -3.027376345333614438, 5.243569643749998122 ) ) ;
#20927 = DIRECTION ( 'NONE',  ( -1.000000000000000000, -0.000000000000000000, -0.000000000000000000 ) ) ;
#20928 = CARTESIAN_POINT ( 'NONE',  ( -3.581514519956692677, 3.492045901024761534, 28.20070727566179869 ) ) ;
#20929 = VECTOR ( 'NONE', #6429, 1000.000000000000000 ) ;
#20930 = CARTESIAN_POINT ( 'NONE',  ( 8.175000000000002487, 6.123233995736764310E-16, -4.999999999999998224 ) ) ;
#20931 = CARTESIAN_POINT ( 'NONE',  ( -4.243569643749998122, 12.24687500061451750, -27.54997392385601174 ) ) ;
#20932 = CARTESIAN_POINT ( 'NONE',  ( 15.03750000122903252, 6.123233995736764310E-16, -4.999999999999998224 ) ) ;
#20933 = CARTESIAN_POINT ( 'NONE',  ( 8.859375000614518214, -4.541064518000417216, -2.621784821875001281 ) ) ;
#20934 = CARTESIAN_POINT ( 'NONE',  ( -4.243569643749999898, 18.41562500061451857, -32.45002607614398471 ) ) ;
#20935 = CARTESIAN_POINT ( 'NONE',  ( 17.66250000122903430, -4.330127018922190985, -2.500000000000001332 ) ) ;
#20936 = CARTESIAN_POINT ( 'NONE',  ( 9.515625000614518214, 3.027376345333611329, 5.243569643749999010 ) ) ;
#20937 = VERTEX_POINT ( 'NONE', #69762 ) ;
#20938 = CARTESIAN_POINT ( 'NONE',  ( 15.52500000000000036, 4.330127018922191873, 2.499999999999999556 ) ) ;
#20939 = CARTESIAN_POINT ( 'NONE',  ( -1.999999999999997113, 17.48750000122903359, -26.53589838486224295 ) ) ;
#20940 = CARTESIAN_POINT ( 'NONE',  ( 11.10937500061451644, -4.541064518000417216, -2.621784821875001281 ) ) ;
#20941 = CARTESIAN_POINT ( 'NONE',  ( 1.626862140677534273E-15, 13.47500000122903252, 34.00000000000000000 ) ) ;
#20942 = CARTESIAN_POINT ( 'NONE',  ( 10.61250000122903536, 4.330127018922192761, -2.499999999999997780 ) ) ;
#20943 = CARTESIAN_POINT ( 'NONE',  ( 19.16250000122903430, 4.330127018922192761, -2.499999999999997780 ) ) ;
#20944 = CARTESIAN_POINT ( 'NONE',  ( 15.81562500061451537, 3.027376345333611329, 5.243569643749999010 ) ) ;
#20945 = CARTESIAN_POINT ( 'NONE',  ( 18.36562500061451431, 3.027376345333613106, -5.243569643749998122 ) ) ;
#20946 = CARTESIAN_POINT ( 'NONE',  ( 26.66250000122903430, -4.330127018922190985, -2.500000000000001332 ) ) ;
#20947 = CARTESIAN_POINT ( 'NONE',  ( 29.58750000122903501, 4.330127018922191873, 2.499999999999999556 ) ) ;
#20948 = CARTESIAN_POINT ( 'NONE',  ( 25.42500000000000071, 4.330127018922191873, 2.499999999999999556 ) ) ;
#20949 = CARTESIAN_POINT ( 'NONE',  ( -3.756430356250001434, 14.25312499938548250, 32.16877607737301048 ) ) ;
#20950 = CARTESIAN_POINT ( 'NONE',  ( 26.70937500061451431, 0.000000000000000000, 5.243569643749999010 ) ) ;
#20951 = CARTESIAN_POINT ( 'NONE',  ( 3.999999999999998668, 17.56250000000000000, 27.69059892324149530 ) ) ;
#20952 = CARTESIAN_POINT ( 'NONE',  ( 12.56250000122903465, 0.000000000000000000, 4.999999999999998224 ) ) ;
#20953 = CARTESIAN_POINT ( 'NONE',  ( 4.162499999999999645, 2.886751345948129099, -4.999999999999998224 ) ) ;
#20954 = CARTESIAN_POINT ( 'NONE',  ( -2.672702088255949472E-15, 13.51250000000000107, 26.00000000000000000 ) ) ;
#20955 = CARTESIAN_POINT ( 'NONE',  ( 7.884375000614517681, -4.541064518000419881, 2.621784821874995952 ) ) ;
#20956 = CARTESIAN_POINT ( 'NONE',  ( 25.52812500061451573, 6.421520780324663323E-16, -5.243569643749999010 ) ) ;
#20957 = FACE_OUTER_BOUND ( 'NONE', #43211, .T. ) ;
#20958 = FACE_OUTER_BOUND ( 'NONE', #36572, .T. ) ;
#20959 = CARTESIAN_POINT ( 'NONE',  ( 30.00000000000000000, 6.123233995736764310E-16, -4.999999999999998224 ) ) ;
#20960 = CARTESIAN_POINT ( 'NONE',  ( 5.109375000614518214, 0.000000000000000000, 5.243569643749999010 ) ) ;
#20961 = CARTESIAN_POINT ( 'NONE',  ( 8.709375000614517859, 0.000000000000000000, 5.243569643749999010 ) ) ;
#20962 = CARTESIAN_POINT ( 'NONE',  ( 28.88437500061451502, 4.541064518000418104, 2.621784821874999949 ) ) ;
#20963 = AXIS2_PLACEMENT_3D ( 'NONE', #40203, #16922, #67558 ) ;
#20964 = CARTESIAN_POINT ( 'NONE',  ( 4.243569643749999010, 11.51562500061459460, 27.54997392385601174 ) ) ;
#20965 = CARTESIAN_POINT ( 'NONE',  ( 22.16250000000000142, 2.886751345948129099, -4.999999999999998224 ) ) ;
#20966 = CARTESIAN_POINT ( 'NONE',  ( 28.87499999999999645, 6.123233995736764310E-16, -4.999999999999998224 ) ) ;
#20967 =( BOUNDED_CURVE ( )  B_SPLINE_CURVE ( 2, ( #12927, #63894, #19182, #59815, #54650, #37292, #30651 ),
 .UNSPECIFIED., .F., .F. ) 
 B_SPLINE_CURVE_WITH_KNOTS ( ( 3, 2, 2, 3 ),
 ( 0.2700000000000000733, 0.2733333333333333726, 0.2766666666666666718, 0.2800000000000000266 ),
 .UNSPECIFIED. ) 
 CURVE ( )  GEOMETRIC_REPRESENTATION_ITEM ( )  RATIONAL_B_SPLINE_CURVE ( ( 0.9999999999999977796, 0.8660254037844409281, 1.000000000000000000, 0.8660254037844387076, 1.000000000000000000, 0.8660254037844387076, 1.000000000000000000 ) ) 
 REPRESENTATION_ITEM ( '' )  );
#20968 = CARTESIAN_POINT ( 'NONE',  ( 4.687500000000000000, 5.773502691896255534, 3.535250795749688894E-16 ) ) ;
#20969 = EDGE_CURVE ( 'NONE', #4055, #9071, #21469, .T. ) ;
#20970 = EDGE_LOOP ( 'NONE', ( #40765, #21203, #14367, #32067 ) ) ;
#20971 = CARTESIAN_POINT ( 'NONE',  ( 19.00312500061451715, 0.000000000000000000, 5.243569643749999010 ) ) ;
#20972 = CARTESIAN_POINT ( 'NONE',  ( 10.71562500061451928, 3.027376345333613106, -5.243569643749998122 ) ) ;
#20973 = CARTESIAN_POINT ( 'NONE',  ( 21.12187500061451217, 4.119189519843966529, 2.378215178124999607 ) ) ;
#20974 = CARTESIAN_POINT ( 'NONE',  ( 8.034375000614518925, 6.421520780324663323E-16, -5.243569643749999010 ) ) ;
#20975 = CARTESIAN_POINT ( 'NONE',  ( 24.26249999999999929, -5.773502691896255534, -1.060575238724906372E-15 ) ) ;
#20976 = CARTESIAN_POINT ( 'NONE',  ( 19.65000000122902790, 5.773502691896255534, 3.535250795749688894E-16 ) ) ;
#20977 = CARTESIAN_POINT ( 'NONE',  ( 13.85625000122903216, 0.000000000000000000, 4.999999999999998224 ) ) ;
#20978 = CARTESIAN_POINT ( 'NONE',  ( 10.24687500061451750, -3.027376345333610441, -5.243569643749999898 ) ) ;
#20979 = CARTESIAN_POINT ( 'NONE',  ( 13.50937500061451679, 4.541064518000418104, -2.621784821874998173 ) ) ;
#20980 = CARTESIAN_POINT ( 'NONE',  ( 23.89687500061451786, 6.054752690667223547, 3.707466751127219781E-16 ) ) ;
#20981 = CARTESIAN_POINT ( 'NONE',  ( 23.36250000000000071, -5.773502691896255534, -1.060575238724906372E-15 ) ) ;
#20982 = ORIENTED_EDGE ( 'NONE', *, *, #721, .F. ) ;
#20983 = CARTESIAN_POINT ( 'NONE',  ( 14.10000000000000142, 4.330127018922192761, -2.499999999999997780 ) ) ;
#20984 = CARTESIAN_POINT ( 'NONE',  ( 17.03437500061451715, 6.421520780324663323E-16, -5.243569643749999010 ) ) ;
#20985 = CARTESIAN_POINT ( 'NONE',  ( 9.496875000614517504, 6.054752690667223547, 3.707466751127219781E-16 ) ) ;
#20986 = CARTESIAN_POINT ( 'NONE',  ( -1.878215178124999163, 19.65312499938548285, 26.74683588394047007 ) ) ;
#20987 = CARTESIAN_POINT ( 'NONE',  ( 21.37499999999999645, 4.330127018922191873, 2.499999999999999556 ) ) ;
#20988 = CARTESIAN_POINT ( 'NONE',  ( -3.999999999999999556, 14.93750000000000000, 27.69059892324149175 ) ) ;
#20989 = CARTESIAN_POINT ( 'NONE',  ( 29.77499999999999858, 6.123233995736764310E-16, -4.999999999999998224 ) ) ;
#20990 = CARTESIAN_POINT ( 'NONE',  ( 22.24687500061451217, -2.746126346562646425, 4.756430356249996549 ) ) ;
#20991 = CARTESIAN_POINT ( 'NONE',  ( 11.99062500061451608, -3.027376345333610441, -5.243569643749999898 ) ) ;
#20992 = CARTESIAN_POINT ( 'NONE',  ( 28.39687500061452141, 6.054752690667223547, 3.707466751127219781E-16 ) ) ;
#20993 = LINE ( 'NONE', #15087, #57263 ) ;
#20994 = CARTESIAN_POINT ( 'NONE',  ( -4.243569643749999898, 19.83125000061451715, -30.00000000000000000 ) ) ;
#20995 = CARTESIAN_POINT ( 'NONE',  ( 13.42499999999999893, -4.330127018922194537, 2.499999999999995559 ) ) ;
#20996 = CARTESIAN_POINT ( 'NONE',  ( 4.000000000000000000, 17.15000000122903145, 32.30940107675849049 ) ) ;
#20997 = CARTESIAN_POINT ( 'NONE',  ( 12.22500000122903430, -5.773502691896255534, -1.060575238724906372E-15 ) ) ;
#20998 = CARTESIAN_POINT ( 'NONE',  ( 22.99687500061451573, 6.054752690667223547, 3.707466751127219781E-16 ) ) ;
#20999 = CARTESIAN_POINT ( 'NONE',  ( 16.35937500061451644, 0.000000000000000000, 5.243569643749999010 ) ) ;
#21000 = CARTESIAN_POINT ( 'NONE',  ( -1.071796769724491005, 12.25759618943233775, 26.00000000000000355 ) ) ;
#21001 = ORIENTED_EDGE ( 'NONE', *, *, #10344, .F. ) ;
#21002 = CARTESIAN_POINT ( 'NONE',  ( 17.42812500061451786, 6.421520780324663323E-16, -5.243569643749999010 ) ) ;
#21003 = CARTESIAN_POINT ( 'NONE',  ( 27.78750000122903074, 4.330127018922191873, 2.499999999999999556 ) ) ;
#21004 = CARTESIAN_POINT ( 'NONE',  ( 17.48437500061451999, 6.421520780324663323E-16, -5.243569643749999010 ) ) ;
#21005 = CARTESIAN_POINT ( 'NONE',  ( 5.728125000614515905, 6.421520780324663323E-16, -5.243569643749999010 ) ) ;
#21006 = CARTESIAN_POINT ( 'NONE',  ( 19.79062500061451502, 6.054752690667223547, 3.707466751127219781E-16 ) ) ;
#21007 = CARTESIAN_POINT ( 'NONE',  ( 2.000000000000001332, 18.35000000000000142, -26.53589838486224650 ) ) ;
#21008 = CARTESIAN_POINT ( 'NONE',  ( 27.68437500061451573, -4.541064518000419881, 2.621784821874995952 ) ) ;
#21009 = CARTESIAN_POINT ( 'NONE',  ( 4.243569643749999010, 12.86562500061451608, 27.54997392385601174 ) ) ;
#21010 = CARTESIAN_POINT ( 'NONE',  ( 16.65937500061452070, 4.541064518000418104, -2.621784821874998173 ) ) ;
#21011 = CARTESIAN_POINT ( 'NONE',  ( 15.75000000122902932, -2.886751345948129988, 4.999999999999997335 ) ) ;
#21012 = CARTESIAN_POINT ( 'NONE',  ( 9.834375000614517859, 5.824947211148865298E-16, -4.756430356249998326 ) ) ;
#21013 = CARTESIAN_POINT ( 'NONE',  ( -1.999999999999997113, 9.837500001229035007, 33.46410161513775705 ) ) ;
#21014 = CARTESIAN_POINT ( 'NONE',  ( 20.67187500061451289, 3.027376345333613106, -5.243569643749998122 ) ) ;
#21015 = CARTESIAN_POINT ( 'NONE',  ( 21.56250000122903288, 0.000000000000000000, 4.999999999999998224 ) ) ;
#21016 = CARTESIAN_POINT ( 'NONE',  ( 24.14062500061451289, -3.027376345333610441, -5.243569643749999898 ) ) ;
#21017 = CARTESIAN_POINT ( 'NONE',  ( 16.39687500061451786, -3.027376345333614438, 5.243569643749998122 ) ) ;
#21018 = CARTESIAN_POINT ( 'NONE',  ( 11.99062500061451608, -3.027376345333610441, -5.243569643749999898 ) ) ;
#21019 = CARTESIAN_POINT ( 'NONE',  ( 4.243569643749999898, 13.78437500061451715, 30.00000000000000000 ) ) ;
#21020 = CARTESIAN_POINT ( 'NONE',  ( 16.75312500061451715, 0.000000000000000000, 5.243569643749999010 ) ) ;
#21021 = CARTESIAN_POINT ( 'NONE',  ( 28.22812500061451502, 6.421520780324663323E-16, -5.243569643749999010 ) ) ;
#21022 = ORIENTED_EDGE ( 'NONE', *, *, #43507, .F. ) ;
#21023 = ORIENTED_EDGE ( 'NONE', *, *, #42304, .F. ) ;
#21024 = CARTESIAN_POINT ( 'NONE',  ( 22.23750000000000071, 5.773502691896255534, 3.535250795749688894E-16 ) ) ;
#21025 = CARTESIAN_POINT ( 'NONE',  ( -2.121784821874999949, 18.88437500061451857, -33.67503911421598417 ) ) ;
#21026 = CARTESIAN_POINT ( 'NONE',  ( 30.00000000000000000, 0.000000000000000000, 0.000000000000000000 ) ) ;
#21027 = CARTESIAN_POINT ( 'NONE',  ( 23.84062500061451928, 6.054752690667223547, 3.707466751127219781E-16 ) ) ;
#21028 = CARTESIAN_POINT ( 'NONE',  ( 5.428125000614517859, 4.541064518000418104, 2.621784821874999949 ) ) ;
#21029 = CARTESIAN_POINT ( 'NONE',  ( 17.43750000122903288, 4.330127018922191873, 2.499999999999999556 ) ) ;
#21030 = CARTESIAN_POINT ( 'NONE',  ( 21.89062500061451289, -3.027376345333610441, -5.243569643749999898 ) ) ;
#21031 = CARTESIAN_POINT ( 'NONE',  ( 23.73749999999999716, -2.886751345948129988, 4.999999999999997335 ) ) ;
#21032 = CARTESIAN_POINT ( 'NONE',  ( 26.39062500061451644, -3.027376345333610441, -5.243569643749999898 ) ) ;
#21033 = CARTESIAN_POINT ( 'NONE',  ( 7.003125000614518036, -4.541064518000417216, -2.621784821875001281 ) ) ;
#21034 =( BOUNDED_CURVE ( )  B_SPLINE_CURVE ( 2, ( #2181, #12886, #41341, #12529, #1462, #6992, #69771, #19139, #40983 ),
 .UNSPECIFIED., .F., .F. ) 
 B_SPLINE_CURVE_WITH_KNOTS ( ( 3, 2, 2, 2, 3 ),
 ( 0.1195652173913043514, 0.1231884057971014551, 0.1304347826086956486, 0.1376811594202898559, 0.1413043478260869734 ),
 .UNSPECIFIED. ) 
 CURVE ( )  GEOMETRIC_REPRESENTATION_ITEM ( )  RATIONAL_B_SPLINE_CURVE ( ( 0.9330127018922194093, 0.9330127018922194093, 1.000000000000000000, 0.8660254037844387076, 1.000000000000000000, 0.8660254037844387076, 1.000000000000000000, 0.9330127018922190762, 0.9330127018922194093 ) ) 
 REPRESENTATION_ITEM ( '' )  );
#21035 = ORIENTED_EDGE ( 'NONE', *, *, #14417, .F. ) ;
#21036 = EDGE_CURVE ( 'NONE', #18562, #49631, #8308, .T. ) ;
#21037 = CARTESIAN_POINT ( 'NONE',  ( 22.97812500061451857, 4.541064518000418104, 2.621784821874999949 ) ) ;
#21038 = CARTESIAN_POINT ( 'NONE',  ( 3.028125000614518392, 6.421520780324663323E-16, -5.243569643749999010 ) ) ;
#21039 = CARTESIAN_POINT ( 'NONE',  ( 11.97187500061451892, -5.492252693125287522, -1.008910452111647106E-15 ) ) ;
#21040 = CARTESIAN_POINT ( 'NONE',  ( -3.137519842735245283E-14, 11.22500000122903430, 34.00000000000000000 ) ) ;
#21041 = CARTESIAN_POINT ( 'NONE',  ( -1.999999999999997113, 12.98750000122903359, -26.53589838486224295 ) ) ;
#21042 = CARTESIAN_POINT ( 'NONE',  ( 13.48125000122903394, -4.330127018922194537, 2.499999999999995559 ) ) ;
#21043 = CARTESIAN_POINT ( 'NONE',  ( 10.20000000000000107, 0.000000000000000000, 4.999999999999998224 ) ) ;
#21044 = CARTESIAN_POINT ( 'NONE',  ( 10.58437500061451964, -4.541064518000419881, 2.621784821874995952 ) ) ;
#21045 = CARTESIAN_POINT ( 'NONE',  ( 5.362500001229033586, 0.000000000000000000, 4.999999999999998224 ) ) ;
#21046 = CARTESIAN_POINT ( 'NONE',  ( 14.03437500061451715, 4.541064518000418104, 2.621784821874999949 ) ) ;
#21047 = CARTESIAN_POINT ( 'NONE',  ( 4.846875000614519813, -3.027376345333610441, -5.243569643749999898 ) ) ;
#21048 = CYLINDRICAL_SURFACE ( 'NONE', #60910, 4.999999999999998224 ) ;
#21049 = CARTESIAN_POINT ( 'NONE',  ( -3.999999999999999112, 10.66250000122903430, 30.00000000000000000 ) ) ;
#21050 = EDGE_CURVE ( 'NONE', #14259, #72082, #54051, .T. ) ;
#21051 = CARTESIAN_POINT ( 'NONE',  ( 11.44687500061451857, -3.027376345333614438, 5.243569643749998122 ) ) ;
#21052 = CARTESIAN_POINT ( 'NONE',  ( 21.78750000122903074, 6.123233995736764310E-16, -4.999999999999998224 ) ) ;
#21053 = CARTESIAN_POINT ( 'NONE',  ( 22.34062500061451573, -3.027376345333610441, -5.243569643749999898 ) ) ;
#21054 = CARTESIAN_POINT ( 'NONE',  ( -4.243569643749999898, 10.85937500061451821, 30.00000000000000000 ) ) ;
#21055 = CARTESIAN_POINT ( 'NONE',  ( -4.243569643749999898, 18.45312500061459104, 30.00000000000000000 ) ) ;
#21056 = CARTESIAN_POINT ( 'NONE',  ( 22.99687500061451573, 6.054752690667223547, 3.707466751127219781E-16 ) ) ;
#21057 = DIRECTION ( 'NONE',  ( 0.000000000000000000, 0.000000000000000000, 1.000000000000000000 ) ) ;
#21058 = CARTESIAN_POINT ( 'NONE',  ( 29.25000000122903288, -2.886751345948129988, 4.999999999999997335 ) ) ;
#21059 = CARTESIAN_POINT ( 'NONE',  ( 19.65937500061451360, 2.746126346562645981, -4.756430356249997438 ) ) ;
#21060 = CARTESIAN_POINT ( 'NONE',  ( 24.51562500061451289, -6.054752690667223547, -1.112240025338166033E-15 ) ) ;
#21061 = CARTESIAN_POINT ( 'NONE',  ( 17.50312500061451715, 4.541064518000418104, -2.621784821874998173 ) ) ;
#21062 = CARTESIAN_POINT ( 'NONE',  ( 14.34375000122903465, -2.886751345948129988, 4.999999999999997335 ) ) ;
#21063 = CARTESIAN_POINT ( 'NONE',  ( 15.04687500061451644, -3.027376345333614438, 5.243569643749998122 ) ) ;
#21064 = CARTESIAN_POINT ( 'NONE',  ( 7.546875000614516438, 4.119189519843966529, -2.378215178124998275 ) ) ;
#21065 = CARTESIAN_POINT ( 'NONE',  ( 27.37500000122903288, 2.886751345948126879, 4.999999999999999112 ) ) ;
#21066 = CARTESIAN_POINT ( 'NONE',  ( 5.896875000614518747, 6.054752690667223547, 3.707466751127219781E-16 ) ) ;
#21067 = CARTESIAN_POINT ( 'NONE',  ( 16.20937500061451786, 4.541064518000418104, -2.621784821874998173 ) ) ;
#21068 = CYLINDRICAL_SURFACE ( 'NONE', #58471, 4.000000000000000000 ) ;
#21069 = CARTESIAN_POINT ( 'NONE',  ( 23.25000000000000000, 0.000000000000000000, 4.999999999999998224 ) ) ;
#21070 = CARTESIAN_POINT ( 'NONE',  ( 4.612500001229032698, -4.330127018922190985, -2.500000000000001332 ) ) ;
#21071 = CARTESIAN_POINT ( 'NONE',  ( 24.00937500061451502, 0.000000000000000000, 5.243569643749999010 ) ) ;
#21072 = CARTESIAN_POINT ( 'NONE',  ( 16.92187500061451999, -6.054752690667223547, -1.112240025338166033E-15 ) ) ;
#21073 = CARTESIAN_POINT ( 'NONE',  ( 1.878215178124997609, 13.12812499938548427, 33.25316411605952993 ) ) ;
#21074 = CARTESIAN_POINT ( 'NONE',  ( 29.06250000000000000, 2.886751345948126879, 4.999999999999999112 ) ) ;
#21075 = CARTESIAN_POINT ( 'NONE',  ( 5.287500000000000533, -2.886751345948129988, 4.999999999999997335 ) ) ;
#21076 = CARTESIAN_POINT ( 'NONE',  ( 9.384375000614516793, 5.492252693125287522, 3.363034840372157021E-16 ) ) ;
#21077 = CARTESIAN_POINT ( 'NONE',  ( 18.47812500061451857, 4.541064518000418104, 2.621784821874999949 ) ) ;
#21078 = CARTESIAN_POINT ( 'NONE',  ( 9.299999999999998934, 0.000000000000000000, 4.999999999999998224 ) ) ;
#21079 = EDGE_CURVE ( 'NONE', #32666, #32497, #66789, .T. ) ;
#21080 = CARTESIAN_POINT ( 'NONE',  ( 4.640625000614518214, -3.027376345333614438, 5.243569643749998122 ) ) ;
#21081 = CARTESIAN_POINT ( 'NONE',  ( 18.37500000000000355, -4.330127018922194537, 2.499999999999995559 ) ) ;
#21082 = CARTESIAN_POINT ( 'NONE',  ( 23.32500000122903572, 2.886751345948126879, 4.999999999999999112 ) ) ;
#21083 = CARTESIAN_POINT ( 'NONE',  ( 1.391695283777658831, 9.904653401742692154, 35.83979371019399451 ) ) ;
#21084 = CARTESIAN_POINT ( 'NONE',  ( 28.47187500061451715, 3.027376345333611329, 5.243569643749999010 ) ) ;
#21085 = ORIENTED_EDGE ( 'NONE', *, *, #62697, .F. ) ;
#21086 = CARTESIAN_POINT ( 'NONE',  ( 17.09062500061451573, 6.054752690667223547, 3.707466751127219781E-16 ) ) ;
#21087 = CARTESIAN_POINT ( 'NONE',  ( 23.54062500061451146, -3.027376345333614438, 5.243569643749998122 ) ) ;
#21088 = CARTESIAN_POINT ( 'NONE',  ( 24.60937500061451644, -4.541064518000417216, -2.621784821875001281 ) ) ;
#21089 = CARTESIAN_POINT ( 'NONE',  ( 9.375000000000001776, -4.330127018922194537, 2.499999999999995559 ) ) ;
#21090 = CARTESIAN_POINT ( 'NONE',  ( 13.00312500061451537, 4.541064518000418104, -2.621784821874998173 ) ) ;
#21091 = CARTESIAN_POINT ( 'NONE',  ( 27.21562500061451928, -6.054752690667223547, -1.112240025338166033E-15 ) ) ;
#21092 = CARTESIAN_POINT ( 'NONE',  ( 13.77187500061451786, -6.054752690667223547, -1.112240025338166033E-15 ) ) ;
#21093 = CARTESIAN_POINT ( 'NONE',  ( 19.35937500061451644, 4.541064518000418104, -2.621784821874998173 ) ) ;
#21094 = CYLINDRICAL_SURFACE ( 'NONE', #56899, 4.999999999999998224 ) ;
#21095 = CARTESIAN_POINT ( 'NONE',  ( 2.121784821875001281, 11.00937500061451857, 33.67503911421598417 ) ) ;
#21096 = CARTESIAN_POINT ( 'NONE',  ( 22.68750000122903288, 6.123233995736764310E-16, -4.999999999999998224 ) ) ;
#21097 = CARTESIAN_POINT ( 'NONE',  ( 17.29687500061451999, -2.746126346562646425, 4.756430356249996549 ) ) ;
#21098 = CARTESIAN_POINT ( 'NONE',  ( 14.61562500061451786, -6.054752690667223547, -1.112240025338166033E-15 ) ) ;
#21099 = CARTESIAN_POINT ( 'NONE',  ( 7.021875000614518747, -6.054752690667223547, -1.112240025338166033E-15 ) ) ;
#21100 = CARTESIAN_POINT ( 'NONE',  ( 7.321875000614516793, 3.027376345333611329, 5.243569643749999010 ) ) ;
#21101 = ORIENTED_EDGE ( 'NONE', *, *, #11164, .T. ) ;
#21102 = CARTESIAN_POINT ( 'NONE',  ( 26.70937500061451431, 0.000000000000000000, 5.243569643749999010 ) ) ;
#21103 = CARTESIAN_POINT ( 'NONE',  ( 19.56562500061451715, -6.054752690667223547, -1.112240025338166033E-15 ) ) ;
#21104 = CARTESIAN_POINT ( 'NONE',  ( 4.246875000614519280, -3.027376345333614438, 5.243569643749998122 ) ) ;
#21105 = CARTESIAN_POINT ( 'NONE',  ( 25.32187500061451857, 3.027376345333611329, 5.243569643749999010 ) ) ;
#21106 = CARTESIAN_POINT ( 'NONE',  ( 19.97812500061451502, -4.541064518000419881, 2.621784821874995952 ) ) ;
#21107 = CARTESIAN_POINT ( 'NONE',  ( -2.828200636599751609E-16, 11.33750000000000036, 25.38119784648299770 ) ) ;
#21108 = CARTESIAN_POINT ( 'NONE',  ( 24.96562500061451573, -6.054752690667223547, -1.112240025338166033E-15 ) ) ;
#21109 = CARTESIAN_POINT ( 'NONE',  ( 6.900000001229035007, -2.886751345948125991, -5.000000000000000000 ) ) ;
#21110 = ORIENTED_EDGE ( 'NONE', *, *, #4806, .T. ) ;
#21111 = CARTESIAN_POINT ( 'NONE',  ( 65.00000000000000000, 7.332543590861157590, 5.218601775200033543 ) ) ;
#21112 = CARTESIAN_POINT ( 'NONE',  ( 2.000000000000001332, 16.55000000000000071, -26.53589838486224650 ) ) ;
#21113 = CARTESIAN_POINT ( 'NONE',  ( 22.12500000122903288, -5.773502691896255534, -1.060575238724906372E-15 ) ) ;
#21114 = CARTESIAN_POINT ( 'NONE',  ( -1.878215178125001827, 13.95312499938548356, 33.25316411605952283 ) ) ;
#21115 = CARTESIAN_POINT ( 'NONE',  ( 3.646875000614520079, 6.054752690667223547, 3.707466751127219781E-16 ) ) ;
#21116 = CARTESIAN_POINT ( 'NONE',  ( 1.071796769724497445, 15.36740381056766758, 26.00000000000000355 ) ) ;
#21117 = CARTESIAN_POINT ( 'NONE',  ( 13.49062500061451608, 6.054752690667223547, 3.707466751127219781E-16 ) ) ;
#21118 = CARTESIAN_POINT ( 'NONE',  ( 8.934375000614517504, 6.421520780324663323E-16, -5.243569643749999010 ) ) ;
#21119 = CARTESIAN_POINT ( 'NONE',  ( 24.75000000122902932, -2.886751345948129988, 4.999999999999997335 ) ) ;
#21120 = CARTESIAN_POINT ( 'NONE',  ( 14.40937500061451715, 4.541064518000418104, -2.621784821874998173 ) ) ;
#21121 = CARTESIAN_POINT ( 'NONE',  ( 29.31562500061451715, 3.027376345333611329, 5.243569643749999010 ) ) ;
#21122 = CARTESIAN_POINT ( 'NONE',  ( 29.36250000000000071, 2.886751345948129099, -4.999999999999998224 ) ) ;
#21123 = CARTESIAN_POINT ( 'NONE',  ( 5.990625000614517859, -3.027376345333614438, 5.243569643749998122 ) ) ;
#21124 = CARTESIAN_POINT ( 'NONE',  ( 15.47812500061451679, -4.541064518000419881, 2.621784821874995952 ) ) ;
#21125 = ORIENTED_EDGE ( 'NONE', *, *, #3997, .T. ) ;
#21126 = CARTESIAN_POINT ( 'NONE',  ( 12.32812500061451821, -4.541064518000419881, 2.621784821874995952 ) ) ;
#21127 = CARTESIAN_POINT ( 'NONE',  ( 8.428125000614517859, 6.421520780324663323E-16, -5.243569643749999010 ) ) ;
#21128 = CARTESIAN_POINT ( 'NONE',  ( 19.39687500061451786, 5.492252693125287522, 3.363034840372157021E-16 ) ) ;
#21129 = CARTESIAN_POINT ( 'NONE',  ( 7.837499999999999467, 5.773502691896255534, 3.535250795749688894E-16 ) ) ;
#21130 = CARTESIAN_POINT ( 'NONE',  ( 4.425000001229032698, 2.886751345948126879, 4.999999999999999112 ) ) ;
#21131 = CARTESIAN_POINT ( 'NONE',  ( 18.89999999999999858, -4.330127018922190985, -2.500000000000001332 ) ) ;
#21132 = ADVANCED_FACE ( 'NONE', ( #9531 ), #15853, .T. ) ;
#21133 = CARTESIAN_POINT ( 'NONE',  ( 19.13437500061451857, -4.541064518000419881, 2.621784821874995952 ) ) ;
#21134 = CARTESIAN_POINT ( 'NONE',  ( 14.25000000122903465, 5.773502691896255534, 3.535250795749688894E-16 ) ) ;
#21135 = CARTESIAN_POINT ( 'NONE',  ( 21.89999999999999858, 0.000000000000000000, 4.999999999999998224 ) ) ;
#21136 = CARTESIAN_POINT ( 'NONE',  ( 4.243569643749999898, 17.29062500061451502, -27.54997392385601529 ) ) ;
#21137 = CARTESIAN_POINT ( 'NONE',  ( 20.62499999999999645, -4.330127018922194537, 2.499999999999995559 ) ) ;
#21138 = CARTESIAN_POINT ( 'NONE',  ( 18.58125000122903003, 6.123233995736764310E-16, -4.999999999999998224 ) ) ;
#21139 = FACE_OUTER_BOUND ( 'NONE', #31759, .T. ) ;
#21140 = CARTESIAN_POINT ( 'NONE',  ( 0.000000000000000000, 0.000000000000000000, -50.00000000000000000 ) ) ;
#21141 = CARTESIAN_POINT ( 'NONE',  ( 1.592000809091587073E-14, 16.28750000000000142, -34.00000000000000000 ) ) ;
#21142 = CARTESIAN_POINT ( 'NONE',  ( 14.25937500061451679, -4.541064518000417216, -2.621784821875001281 ) ) ;
#21143 = CARTESIAN_POINT ( 'NONE',  ( 26.88749999999999574, -2.886751345948129988, 4.999999999999997335 ) ) ;
#21144 = CARTESIAN_POINT ( 'NONE',  ( 10.52812500061451750, -4.541064518000419881, 2.621784821874995952 ) ) ;
#21145 = CARTESIAN_POINT ( 'NONE',  ( 27.72187500061451715, 5.824947211148865298E-16, -4.756430356249998326 ) ) ;
#21146 = CARTESIAN_POINT ( 'NONE',  ( 22.43437500061451573, 6.421520780324663323E-16, -5.243569643749999010 ) ) ;
#21147 = CARTESIAN_POINT ( 'NONE',  ( 13.20937500061451431, -5.492252693125287522, -1.008910452111647106E-15 ) ) ;
#21148 = CARTESIAN_POINT ( 'NONE',  ( 8.428125000614517859, 6.421520780324663323E-16, -5.243569643749999010 ) ) ;
#21149 = CARTESIAN_POINT ( 'NONE',  ( 13.99687500061451928, 6.054752690667223547, 3.707466751127219781E-16 ) ) ;
#21150 = ORIENTED_EDGE ( 'NONE', *, *, #14141, .T. ) ;
#21151 = CARTESIAN_POINT ( 'NONE',  ( 23.40937500061451715, 4.541064518000418104, -2.621784821874998173 ) ) ;
#21152 = CARTESIAN_POINT ( 'NONE',  ( 3.458282317606260037, 3.615826433065251422, -32.02515933644849611 ) ) ;
#21153 = FACE_OUTER_BOUND ( 'NONE', #2322, .T. ) ;
#21155 = ADVANCED_FACE ( 'NONE', ( #51499 ), #24128, .T. ) ;
#21154 = CARTESIAN_POINT ( 'NONE',  ( 5.100000000000000533, 4.330127018922192761, -2.499999999999997780 ) ) ;
#21156 = CARTESIAN_POINT ( 'NONE',  ( 17.06250000122903288, 0.000000000000000000, 4.999999999999998224 ) ) ;
#21157 = CARTESIAN_POINT ( 'NONE',  ( 16.74375000122903145, -2.886751345948181946, -4.999999999999904077 ) ) ;
#21158 = CARTESIAN_POINT ( 'NONE',  ( 7.884375000614518569, -2.746126346562642428, -4.756430356249999214 ) ) ;
#21159 = EDGE_LOOP ( 'NONE', ( #42976, #47050, #51122, #6538 ) ) ;
#21160 = CARTESIAN_POINT ( 'NONE',  ( 15.52500000000000036, 4.330127018922191873, 2.499999999999999556 ) ) ;
#21161 = CARTESIAN_POINT ( 'NONE',  ( 16.61250000000000426, -5.773502691896255534, -1.060575238724906372E-15 ) ) ;
#21162 = CARTESIAN_POINT ( 'NONE',  ( 12.06562500061451537, 3.027376345333613106, -5.243569643749998122 ) ) ;
#21163 = VERTEX_POINT ( 'NONE', #45601 ) ;
#21164 = CARTESIAN_POINT ( 'NONE',  ( 26.28750000000000142, 5.773502691896255534, 3.535250795749688401E-16 ) ) ;
#21165 = CARTESIAN_POINT ( 'NONE',  ( -3.000416591977282496E-16, 16.14687500061451431, -34.90005215228797653 ) ) ;
#21166 = CARTESIAN_POINT ( 'NONE',  ( 3.515625000614516882, 3.027376345333613106, -5.243569643749998122 ) ) ;
#21167 = CARTESIAN_POINT ( 'NONE',  ( -3.756430356250000990, 15.60312499938548392, 32.16877607737301048 ) ) ;
#21168 = CARTESIAN_POINT ( 'NONE',  ( 10.65000000000000036, 0.000000000000000000, 4.999999999999998224 ) ) ;
#21169 = CYLINDRICAL_SURFACE ( 'NONE', #70382, 3.999999999999996447 ) ;
#21170 = ORIENTED_EDGE ( 'NONE', *, *, #46759, .T. ) ;
#21171 = CARTESIAN_POINT ( 'NONE',  ( 24.55312500061451786, -4.541064518000417216, -2.621784821875001281 ) ) ;
#21172 = CARTESIAN_POINT ( 'NONE',  ( 25.59375000122903643, -2.886751345948157965, 4.999999999999948486 ) ) ;
#21173 = CARTESIAN_POINT ( 'NONE',  ( 3.756430356250000102, 18.94062499938548427, 30.00000000000000000 ) ) ;
#21174 = CARTESIAN_POINT ( 'NONE',  ( 20.37187500061451573, 3.027376345333611329, 5.243569643749999010 ) ) ;
#21175 = CARTESIAN_POINT ( 'NONE',  ( 19.64062500061451644, -3.027376345333610441, -5.243569643749999898 ) ) ;
#21176 = EDGE_CURVE ( 'NONE', #63910, #17100, #13917, .T. ) ;
#21177 = CARTESIAN_POINT ( 'NONE',  ( -3.000416591977282496E-16, 13.84062500061459744, -34.90005215228797653 ) ) ;
#21178 = CARTESIAN_POINT ( 'NONE',  ( 22.83750000122903501, 4.330127018922191873, 2.499999999999999556 ) ) ;
#21179 = CARTESIAN_POINT ( 'NONE',  ( 4.415625000614518569, 3.027376345333613106, -5.243569643749998122 ) ) ;
#21180 = CARTESIAN_POINT ( 'NONE',  ( 24.98437500061451644, -4.119189519843968306, 2.378215178124996054 ) ) ;
#21181 = CARTESIAN_POINT ( 'NONE',  ( 20.72812500061451502, 4.541064518000418104, 2.621784821874999949 ) ) ;
#21182 = CARTESIAN_POINT ( 'NONE',  ( 8.596875000614518925, 5.492252693125287522, 3.363034840372157021E-16 ) ) ;
#21183 = CARTESIAN_POINT ( 'NONE',  ( -3.756430356249999214, 17.77812499938548285, 27.83122392262697531 ) ) ;
#21184 =( BOUNDED_CURVE ( )  B_SPLINE_CURVE ( 2, ( #72632, #5033, #5396, #60801, #67102, #27570, #72994 ),
 .UNSPECIFIED., .F., .F. ) 
 B_SPLINE_CURVE_WITH_KNOTS ( ( 3, 2, 2, 3 ),
 ( 0.8600000000000002087, 0.8633333333333333970, 0.8666666666666668073, 0.8699999999999999956 ),
 .UNSPECIFIED. ) 
 CURVE ( )  GEOMETRIC_REPRESENTATION_ITEM ( )  RATIONAL_B_SPLINE_CURVE ( ( 0.9999999999999911182, 0.8660254037844475894, 1.000000000000000000, 0.8660254037844387076, 1.000000000000000000, 0.8660254037844387076, 1.000000000000000000 ) ) 
 REPRESENTATION_ITEM ( '' )  );
#21185 = CARTESIAN_POINT ( 'NONE',  ( 16.20937500061451786, 4.541064518000418104, -2.621784821874998173 ) ) ;
#21186 = CARTESIAN_POINT ( 'NONE',  ( 14.07187500061451679, 3.027376345333611329, 5.243569643749999010 ) ) ;
#21187 = CARTESIAN_POINT ( 'NONE',  ( 22.92187500061451644, 3.027376345333613106, -5.243569643749998122 ) ) ;
#21188 = ORIENTED_EDGE ( 'NONE', *, *, #58553, .T. ) ;
#21189 = CARTESIAN_POINT ( 'NONE',  ( -2.121784821874999949, 12.58437500061451786, 26.32496088578401938 ) ) ;
#21190 = CARTESIAN_POINT ( 'NONE',  ( 3.853125000614517681, -4.541064518000417216, -2.621784821875001281 ) ) ;
#21191 = CARTESIAN_POINT ( 'NONE',  ( 27.36562500061451786, 3.027376345333613106, -5.243569643749998122 ) ) ;
#21192 = CARTESIAN_POINT ( 'NONE',  ( 27.89062500061451289, 6.054752690667223547, 3.707466751127219781E-16 ) ) ;
#21193 = CARTESIAN_POINT ( 'NONE',  ( 8.231250001229033941, 6.123233995736764310E-16, -4.999999999999998224 ) ) ;
#21194 = CARTESIAN_POINT ( 'NONE',  ( 3.999999999999998668, 18.01249999999999929, 27.69059892324149175 ) ) ;
#21195 = CARTESIAN_POINT ( 'NONE',  ( 6.946875000614517681, -3.027376345333614438, 5.243569643749998122 ) ) ;
#21196 = CARTESIAN_POINT ( 'NONE',  ( 15.18750000122903465, 4.330127018922191873, 2.499999999999999556 ) ) ;
#21197 = CARTESIAN_POINT ( 'NONE',  ( 10.23750000122903359, 4.330127018922191873, 2.499999999999999556 ) ) ;
#21198 = CARTESIAN_POINT ( 'NONE',  ( 29.51250000122903216, 4.330127018922192761, -2.499999999999997780 ) ) ;
#21199 = CARTESIAN_POINT ( 'NONE',  ( -8.484601909799255319E-16, 16.83124999877096784, 34.61880215351700940 ) ) ;
#21200 = CARTESIAN_POINT ( 'NONE',  ( 17.83125000122903003, 4.330127018922191873, 2.499999999999999556 ) ) ;
#21201 = CARTESIAN_POINT ( 'NONE',  ( 11.82187500061451679, 3.027376345333611329, 5.243569643749999010 ) ) ;
#21202 = DIRECTION ( 'NONE',  ( 0.000000000000000000, 0.000000000000000000, -1.000000000000000000 ) ) ;
#21203 = ORIENTED_EDGE ( 'NONE', *, *, #64083, .F. ) ;
#21204 = CARTESIAN_POINT ( 'NONE',  ( 19.67812500061451786, 6.421520780324663323E-16, -5.243569643749999010 ) ) ;
#21205 = CARTESIAN_POINT ( 'NONE',  ( 7.340625000614518392, -3.027376345333614438, 5.243569643749998122 ) ) ;
#21206 = CARTESIAN_POINT ( 'NONE',  ( 22.80937500061451573, -4.541064518000417216, -2.621784821875001281 ) ) ;
#21207 = EDGE_CURVE ( 'NONE', #4525, #26188, #61585, .T. ) ;
#21208 = CARTESIAN_POINT ( 'NONE',  ( 4.940625000614515372, 6.054752690667223547, 3.707466751127219781E-16 ) ) ;
#21209 = CARTESIAN_POINT ( 'NONE',  ( 30.00000000000000000, 0.000000000000000000, 0.000000000000000000 ) ) ;
#21210 = CARTESIAN_POINT ( 'NONE',  ( 7.950000001229033053, 5.773502691896255534, 3.535250795749688894E-16 ) ) ;
#21211 = CARTESIAN_POINT ( 'NONE',  ( 23.01562500061451644, 3.027376345333611329, 5.243569643749999010 ) ) ;
#21212 = CARTESIAN_POINT ( 'NONE',  ( 3.999999999999999112, 17.18750000122903288, -30.00000000000000000 ) ) ;
#21213 = CARTESIAN_POINT ( 'NONE',  ( 7.762500001229033053, -4.330127018922190985, -2.500000000000001332 ) ) ;
#21214 = CARTESIAN_POINT ( 'NONE',  ( 18.62812500061451715, -4.541064518000419881, 2.621784821874995952 ) ) ;
#21215 = CARTESIAN_POINT ( 'NONE',  ( 14.91562500061451679, 3.027376345333611329, 5.243569643749999010 ) ) ;
#21216 = CARTESIAN_POINT ( 'NONE',  ( 29.37187500061451928, 2.746126346562643317, 4.756430356249998326 ) ) ;
#21217 = CARTESIAN_POINT ( 'NONE',  ( 15.29999999999999893, -4.330127018922190985, -2.500000000000001332 ) ) ;
#21218 = CARTESIAN_POINT ( 'NONE',  ( 11.47500000122903252, 2.886751345948129099, -4.999999999999998224 ) ) ;
#21219 = EDGE_CURVE ( 'NONE', #8626, #5506, #51675, .T. ) ;
#21220 = CARTESIAN_POINT ( 'NONE',  ( 8.578125000614518214, 4.541064518000418104, 2.621784821874999949 ) ) ;
#21221 = CARTESIAN_POINT ( 'NONE',  ( 11.57812500061451644, 6.421520780324663323E-16, -5.243569643749999010 ) ) ;
#21222 = CARTESIAN_POINT ( 'NONE',  ( 21.07500000122903572, 2.886751345948126879, 4.999999999999999112 ) ) ;
#21223 = CARTESIAN_POINT ( 'NONE',  ( -4.243569643749999898, 13.97187500061451715, -32.45002607614398471 ) ) ;
#21224 = CARTESIAN_POINT ( 'NONE',  ( 18.30937500061451928, -4.541064518000417216, -2.621784821875001281 ) ) ;
#21225 = CARTESIAN_POINT ( 'NONE',  ( 6.187500001229032875, 4.330127018922191873, 2.499999999999999556 ) ) ;
#21226 =( BOUNDED_CURVE ( )  B_SPLINE_CURVE ( 2, ( #19949, #53578, #30677, #19578, #53209, #14414, #25126 ),
 .UNSPECIFIED., .F., .F. ) 
 B_SPLINE_CURVE_WITH_KNOTS ( ( 3, 2, 2, 3 ),
 ( 0.3583333333333333925, 0.3611111111111111605, 0.3638888888888888729, 0.3666666666666666408 ),
 .UNSPECIFIED. ) 
 CURVE ( )  GEOMETRIC_REPRESENTATION_ITEM ( )  RATIONAL_B_SPLINE_CURVE ( ( 0.9999999999999973355, 0.8660254037844413721, 1.000000000000000000, 0.8660254037844387076, 1.000000000000000000, 0.8660254037844387076, 1.000000000000000000 ) ) 
 REPRESENTATION_ITEM ( '' )  );
#21227 = CARTESIAN_POINT ( 'NONE',  ( 3.871875000614519280, -6.054752690667223547, -1.112240025338166033E-15 ) ) ;
#21228 = CARTESIAN_POINT ( 'NONE',  ( 23.78437500061451360, 6.421520780324663323E-16, -5.243569643749999010 ) ) ;
#21229 = CARTESIAN_POINT ( 'NONE',  ( 7.837500001229035007, 6.123233995736764310E-16, -4.999999999999998224 ) ) ;
#21230 = CARTESIAN_POINT ( 'NONE',  ( 20.05312500061451431, -4.541064518000417216, -2.621784821875001281 ) ) ;
#21231 = CARTESIAN_POINT ( 'NONE',  ( 11.00625000122903252, 4.330127018922192761, -2.499999999999997780 ) ) ;
#21232 = CARTESIAN_POINT ( 'NONE',  ( 1.878215178124997609, 19.42812499938548143, 33.25316411605952993 ) ) ;
#21233 = LINE ( 'NONE', #44884, #53577 ) ;
#21234 = CARTESIAN_POINT ( 'NONE',  ( 28.62187500061451573, -6.054752690667223547, -1.112240025338166033E-15 ) ) ;
#21235 = CARTESIAN_POINT ( 'NONE',  ( 20.55937500061451217, 2.746126346562645981, -4.756430356249997438 ) ) ;
#21236 = CARTESIAN_POINT ( 'NONE',  ( 13.90312500061451750, 4.541064518000418104, -2.621784821874998173 ) ) ;
#21237 = CARTESIAN_POINT ( 'NONE',  ( 13.50937500061451679, 4.541064518000418104, -2.621784821874998173 ) ) ;
#21238 = ORIENTED_EDGE ( 'NONE', *, *, #11885, .F. ) ;
#21239 = CARTESIAN_POINT ( 'NONE',  ( 1.592000809091587073E-14, 17.18750000000000355, -34.00000000000000000 ) ) ;
#21240 = CARTESIAN_POINT ( 'NONE',  ( 23.50312500061451360, 0.000000000000000000, 5.243569643749999010 ) ) ;
#21241 = FACE_OUTER_BOUND ( 'NONE', #56338, .T. ) ;
#21242 = CARTESIAN_POINT ( 'NONE',  ( 28.65000000122903145, 5.773502691896255534, 3.535250795749688401E-16 ) ) ;
#21243 = CARTESIAN_POINT ( 'NONE',  ( 12.26249999999999929, 2.886751345948129099, -4.999999999999998224 ) ) ;
#21244 = CARTESIAN_POINT ( 'NONE',  ( 25.16250000122903074, 0.000000000000000000, 4.999999999999998224 ) ) ;
#21245 = CARTESIAN_POINT ( 'NONE',  ( 18.10312500061451502, 0.000000000000000000, 5.243569643749999010 ) ) ;
#21246 = ORIENTED_EDGE ( 'NONE', *, *, #10213, .T. ) ;
#21247 = CARTESIAN_POINT ( 'NONE',  ( 22.91249999999999432, -5.773502691896255534, -1.060575238724906372E-15 ) ) ;
#21248 = CARTESIAN_POINT ( 'NONE',  ( 23.03437500061451715, 4.541064518000418104, 2.621784821874999949 ) ) ;
#21249 =( BOUNDED_CURVE ( )  B_SPLINE_CURVE ( 2, ( #67353, #16716, #9364, #31897, #54433, #3832, #26353, #48892, #71422 ),
 .UNSPECIFIED., .F., .F. ) 
 B_SPLINE_CURVE_WITH_KNOTS ( ( 3, 2, 2, 2, 3 ),
 ( 0.8586956521739130821, 0.8623188405797101996, 0.8695652173913043237, 0.8768115942028985588, 0.8804347826086956763 ),
 .UNSPECIFIED. ) 
 CURVE ( )  GEOMETRIC_REPRESENTATION_ITEM ( )  RATIONAL_B_SPLINE_CURVE ( ( 0.9330127018922194093, 0.9330127018922194093, 1.000000000000000000, 0.8660254037844387076, 1.000000000000000000, 0.8660254037844387076, 1.000000000000000000, 0.9330127018922194093, 0.9330127018922194093 ) ) 
 REPRESENTATION_ITEM ( '' )  );
#21250 = ORIENTED_EDGE ( 'NONE', *, *, #35651, .F. ) ;
#21251 = CARTESIAN_POINT ( 'NONE',  ( 4.000000000000000000, 19.28749999999999787, 27.69059892324149885 ) ) ;
#21252 = CARTESIAN_POINT ( 'NONE',  ( 11.65312500061451573, 4.541064518000418104, -2.621784821874998173 ) ) ;
#21253 = CARTESIAN_POINT ( 'NONE',  ( 11.06250000000000178, 2.886751345948126879, 4.999999999999998224 ) ) ;
#21254 = CARTESIAN_POINT ( 'NONE',  ( 15.27187500061451608, 4.119189519843966529, 2.378215178124999607 ) ) ;
#21255 = CARTESIAN_POINT ( 'NONE',  ( 16.16250000000000142, -5.773502691896255534, -1.060575238724906372E-15 ) ) ;
#21256 = CARTESIAN_POINT ( 'NONE',  ( 25.23749999999999716, -2.886751345948125991, -5.000000000000000000 ) ) ;
#21257 = CARTESIAN_POINT ( 'NONE',  ( 9.001249775931846008E-16, 19.46562500061451573, 34.90005215228797653 ) ) ;
#21258 = CARTESIAN_POINT ( 'NONE',  ( 4.734375000614518214, -4.541064518000419881, 2.621784821874995952 ) ) ;
#21259 = CARTESIAN_POINT ( 'NONE',  ( 16.47187500061452070, -6.054752690667223547, -1.112240025338166033E-15 ) ) ;
#21260 = CARTESIAN_POINT ( 'NONE',  ( 27.94687500061451502, 6.054752690667223547, 3.707466751127219781E-16 ) ) ;
#21261 = EDGE_LOOP ( 'NONE', ( #17008, #59671, #12436, #14523 ) ) ;
#21262 = CARTESIAN_POINT ( 'NONE',  ( 25.45312500061451644, -4.541064518000417216, -2.621784821875001281 ) ) ;
#21263 = CARTESIAN_POINT ( 'NONE',  ( 27.30937500061451573, -4.541064518000417216, -2.621784821875001281 ) ) ;
#21264 = CARTESIAN_POINT ( 'NONE',  ( 16.85625000122903572, 4.330127018922192761, -2.499999999999997780 ) ) ;
#21265 = CARTESIAN_POINT ( 'NONE',  ( 14.47499999999999964, 6.123233995736764310E-16, -4.999999999999998224 ) ) ;
#21266 = CARTESIAN_POINT ( 'NONE',  ( 11.01562500061451821, -6.054752690667223547, -1.112240025338166033E-15 ) ) ;
#21267 = CARTESIAN_POINT ( 'NONE',  ( -3.999999999999999112, 20.00000000000000000, 30.00000000000000000 ) ) ;
#21268 = CARTESIAN_POINT ( 'NONE',  ( 17.10000000000000142, -4.330127018922190985, -2.500000000000001332 ) ) ;
#21269 = CARTESIAN_POINT ( 'NONE',  ( 28.26562500061450933, 3.027376345333612662, -5.243569643749998122 ) ) ;
#21270 = CARTESIAN_POINT ( 'NONE',  ( 16.12500000122903288, 2.886751345948126879, 4.999999999999999112 ) ) ;
#21271 = DIRECTION ( 'NONE',  ( -1.000000000000000000, -0.000000000000000000, -0.000000000000000000 ) ) ;
#21272 = CARTESIAN_POINT ( 'NONE',  ( 14.25937500061451679, -4.119189519843965641, -2.378215178125001383 ) ) ;
#21273 = CARTESIAN_POINT ( 'NONE',  ( 5.878125000614517148, 4.541064518000418104, 2.621784821874999949 ) ) ;
#21274 = CARTESIAN_POINT ( 'NONE',  ( 21.94687500061451857, -3.027376345333610441, -5.243569643749999898 ) ) ;
#21275 = CARTESIAN_POINT ( 'NONE',  ( 4.243569643749999898, 16.03437500061451715, 30.00000000000000000 ) ) ;
#21276 = CARTESIAN_POINT ( 'NONE',  ( 20.48437500061451289, -4.541064518000419881, 2.621784821874995952 ) ) ;
#21277 = CARTESIAN_POINT ( 'NONE',  ( 3.750000000000000000, 4.330127018922192761, -2.499999999999997780 ) ) ;
#21278 = CARTESIAN_POINT ( 'NONE',  ( 2.121784821874999061, 18.35937500061451644, 26.32496088578401583 ) ) ;
#21279 = CARTESIAN_POINT ( 'NONE',  ( 12.40312500061451573, -4.541064518000417216, -2.621784821875001281 ) ) ;
#21280 = CARTESIAN_POINT ( 'NONE',  ( 3.000000001229032875, 5.773502691896255534, 3.535250795749688894E-16 ) ) ;
#21281 = CARTESIAN_POINT ( 'NONE',  ( 7.659375000614518036, 4.541064518000418104, -2.621784821874998173 ) ) ;
#21282 = CARTESIAN_POINT ( 'NONE',  ( 12.97499999999999964, -4.330127018922194537, 2.499999999999995559 ) ) ;
#21283 =( BOUNDED_CURVE ( )  B_SPLINE_CURVE ( 2, ( #54023, #31481, #65088, #26680, #42929, #70273, #42200 ),
 .UNSPECIFIED., .F., .F. ) 
 B_SPLINE_CURVE_WITH_KNOTS ( ( 3, 2, 2, 3 ),
 ( 0.2416666666666666963, 0.2444444444444444642, 0.2472222222222222321, 0.2500000000000000000 ),
 .UNSPECIFIED. ) 
 CURVE ( )  GEOMETRIC_REPRESENTATION_ITEM ( )  RATIONAL_B_SPLINE_CURVE ( ( 0.9999999999999986677, 0.8660254037844400399, 1.000000000000000000, 0.8660254037844387076, 1.000000000000000000, 0.8660254037844387076, 1.000000000000000000 ) ) 
 REPRESENTATION_ITEM ( '' )  );
#21284 = CARTESIAN_POINT ( 'NONE',  ( 9.328125000614518214, 6.421520780324663323E-16, -5.243569643749999010 ) ) ;
#21285 = CARTESIAN_POINT ( 'NONE',  ( 13.43437500061451750, 6.421520780324663323E-16, -5.243569643749999010 ) ) ;
#21286 = CARTESIAN_POINT ( 'NONE',  ( 21.58125000122903359, -4.330127018922194537, 2.499999999999995559 ) ) ;
#21287 = CARTESIAN_POINT ( 'NONE',  ( 21.86250000122903003, 4.330127018922192761, -2.499999999999997780 ) ) ;
#21288 = CARTESIAN_POINT ( 'NONE',  ( 8.521875000614516082, 3.027376345333613106, -5.243569643749998122 ) ) ;
#21289 = CARTESIAN_POINT ( 'NONE',  ( 9.140625000614518214, -3.027376345333614438, 5.243569643749998122 ) ) ;
#21290 = CARTESIAN_POINT ( 'NONE',  ( 25.40625000122903288, 4.330127018922192761, -2.499999999999997780 ) ) ;
#21291 = ADVANCED_FACE ( 'NONE', ( #33775 ), #17498, .T. ) ;
#21292 = CARTESIAN_POINT ( 'NONE',  ( 21.34687500061451715, -3.027376345333614438, 5.243569643749998122 ) ) ;
#21293 = LINE ( 'NONE', #59344, #58458 ) ;
#21294 = CARTESIAN_POINT ( 'NONE',  ( -3.992949912593974471, 3.009468837316803480, 29.72536534029088884 ) ) ;
#21295 = DIRECTION ( 'NONE',  ( 0.000000000000000000, 0.000000000000000000, -1.000000000000000000 ) ) ;
#21296 = CARTESIAN_POINT ( 'NONE',  ( 9.001249775931846008E-16, 12.32187500061451857, -25.09994784771203058 ) ) ;
#21297 = CARTESIAN_POINT ( 'NONE',  ( 14.36250000122903359, 0.000000000000000000, 4.999999999999998224 ) ) ;
#21298 = CARTESIAN_POINT ( 'NONE',  ( 4.243569643749999898, 15.07812500061451644, -30.00000000000000000 ) ) ;
#21299 = CARTESIAN_POINT ( 'NONE',  ( 18.30000000122903359, 5.773502691896255534, 3.535250795749688894E-16 ) ) ;
#21300 = CARTESIAN_POINT ( 'NONE',  ( 10.37812500061451715, 4.541064518000418104, 2.621784821874999949 ) ) ;
#21301 = ORIENTED_EDGE ( 'NONE', *, *, #9426, .F. ) ;
#21302 = CARTESIAN_POINT ( 'NONE',  ( 14.21249999999999858, 2.886751345948126879, 4.999999999999999112 ) ) ;
#21303 = CARTESIAN_POINT ( 'NONE',  ( 10.33125000122903359, -4.330127018922194537, 2.499999999999995559 ) ) ;
#21304 = CARTESIAN_POINT ( 'NONE',  ( 22.41562500061451502, 3.027376345333613106, -5.243569643749998122 ) ) ;
#21305 = CARTESIAN_POINT ( 'NONE',  ( 10.99687500061451928, -3.027376345333614438, 5.243569643749998122 ) ) ;
#21306 = CARTESIAN_POINT ( 'NONE',  ( -3.999999999999999112, 14.26250000122903572, 30.00000000000000000 ) ) ;
#21307 = CARTESIAN_POINT ( 'NONE',  ( 9.112500001229033586, -4.330127018922190985, -2.500000000000001332 ) ) ;
#21308 = EDGE_CURVE ( 'NONE', #29028, #64526, #6065, .T. ) ;
#21309 = CARTESIAN_POINT ( 'NONE',  ( 18.60000000122903430, -2.886751345948125991, -5.000000000000000000 ) ) ;
#21310 = CARTESIAN_POINT ( 'NONE',  ( 15.85312500061451857, 0.000000000000000000, 5.243569643749999010 ) ) ;
#21311 = CARTESIAN_POINT ( 'NONE',  ( 18.02812500061451573, 4.541064518000418104, 2.621784821874999949 ) ) ;
#21312 = CARTESIAN_POINT ( 'NONE',  ( 25.12500000122903288, 2.886751345948126879, 4.999999999999999112 ) ) ;
#21313 = EDGE_CURVE ( 'NONE', #29801, #16672, #30946, .T. ) ;
#21314 = CARTESIAN_POINT ( 'NONE',  ( 27.71250000122903145, 4.330127018922192761, -2.499999999999997780 ) ) ;
#21315 = CARTESIAN_POINT ( 'NONE',  ( 22.38749999999999929, -2.886751345948129988, 4.999999999999997335 ) ) ;
#21316 = CARTESIAN_POINT ( 'NONE',  ( -3.756430356250000102, 14.21562499938548285, 30.00000000000000000 ) ) ;
#21317 = CARTESIAN_POINT ( 'NONE',  ( 24.94687500061451502, -3.027376345333614438, 5.243569643749998122 ) ) ;
#21318 = CARTESIAN_POINT ( 'NONE',  ( 7.320879633048903241E-15, 17.63749999999999218, 26.00000000000000355 ) ) ;
#21319 = CARTESIAN_POINT ( 'NONE',  ( 12.33750000122903145, 6.123233995736764310E-16, -4.999999999999998224 ) ) ;
#21320 = CARTESIAN_POINT ( 'NONE',  ( 29.48437500061451644, -4.541064518000419881, 2.621784821874995952 ) ) ;
#21321 = LINE ( 'NONE', #66032, #44378 ) ;
#21322 = CARTESIAN_POINT ( 'NONE',  ( 4.021875000614516082, 3.027376345333613106, -5.243569643749998122 ) ) ;
#21323 = CARTESIAN_POINT ( 'NONE',  ( 25.86562500061451431, -6.054752690667223547, -1.112240025338166033E-15 ) ) ;
#21324 = CARTESIAN_POINT ( 'NONE',  ( -1.878215178124999163, 12.90312499938548463, 26.74683588394047007 ) ) ;
#21325 = CARTESIAN_POINT ( 'NONE',  ( 11.51250000122903216, 4.330127018922192761, -2.499999999999997780 ) ) ;
#21326 = CARTESIAN_POINT ( 'NONE',  ( 10.35937500061451644, 4.541064518000418104, -2.621784821874998173 ) ) ;
#21327 = CARTESIAN_POINT ( 'NONE',  ( 3.617702362022032325, -3.451409801779584452, 3.617702362022032325 ) ) ;
#21328 = CARTESIAN_POINT ( 'NONE',  ( 28.86562500061451786, 3.027376345333611329, 5.243569643749999010 ) ) ;
#21329 = CARTESIAN_POINT ( 'NONE',  ( 8.071875000614518569, 3.027376345333613106, -5.243569643749998122 ) ) ;
#21330 = CARTESIAN_POINT ( 'NONE',  ( 29.03437500061451715, -4.541064518000419881, 2.621784821874995952 ) ) ;
#21331 = CARTESIAN_POINT ( 'NONE',  ( -3.000416591977282496E-16, 12.49062500061459602, 25.09994784771203058 ) ) ;
#21332 = CARTESIAN_POINT ( 'NONE',  ( 22.87500000000000000, -4.330127018922194537, 2.499999999999995559 ) ) ;
#21333 = EDGE_LOOP ( 'NONE', ( #69115, #21730, #19398, #58061 ) ) ;
#21334 = CARTESIAN_POINT ( 'NONE',  ( -1.071796769724487453, 17.65759618943233633, -34.00000000000000000 ) ) ;
#21335 = CARTESIAN_POINT ( 'NONE',  ( 4.200000000000001954, 4.330127018922192761, -2.499999999999997780 ) ) ;
#21336 = ORIENTED_EDGE ( 'NONE', *, *, #25207, .T. ) ;
#21337 = CARTESIAN_POINT ( 'NONE',  ( 18.51562500061451289, 3.027376345333611329, 5.243569643749999010 ) ) ;
#21338 = CARTESIAN_POINT ( 'NONE',  ( 11.69062500061451360, 6.054752690667223547, 3.707466751127219781E-16 ) ) ;
#21339 = CARTESIAN_POINT ( 'NONE',  ( 21.98437500061451644, 5.492252693125287522, 3.363034840372157021E-16 ) ) ;
#21340 = CARTESIAN_POINT ( 'NONE',  ( 6.759375000614516793, 4.541064518000418104, -2.621784821874998173 ) ) ;
#21341 = CARTESIAN_POINT ( 'NONE',  ( 20.13750000122903216, 4.330127018922191873, 2.499999999999999556 ) ) ;
#21342 = CARTESIAN_POINT ( 'NONE',  ( -1.626862140677534273E-15, 19.58750000000000213, 34.00000000000000000 ) ) ;
#21343 = CARTESIAN_POINT ( 'NONE',  ( 7.171875000614517326, 3.027376345333613106, -5.243569643749998122 ) ) ;
#21344 = CARTESIAN_POINT ( 'NONE',  ( 14.22187500061451537, -6.054752690667223547, -1.112240025338166033E-15 ) ) ;
#21345 = CARTESIAN_POINT ( 'NONE',  ( 23.22187500061451715, -6.054752690667223547, -1.112240025338166033E-15 ) ) ;
#21346 = VERTEX_POINT ( 'NONE', #12322 ) ;
#21347 = CARTESIAN_POINT ( 'NONE',  ( 12.15000000000000036, -4.330127018922190985, -2.500000000000001332 ) ) ;
#21348 = CARTESIAN_POINT ( 'NONE',  ( 17.74687500061451928, -3.027376345333614438, 5.243569643749998122 ) ) ;
#21349 = CARTESIAN_POINT ( 'NONE',  ( 9.796875000614519990, -3.027376345333610441, -5.243569643749999898 ) ) ;
#21350 = CARTESIAN_POINT ( 'NONE',  ( -7.967954043666661671E-16, 14.77812499938548463, 34.33755215474603517 ) ) ;
#21351 = CARTESIAN_POINT ( 'NONE',  ( 21.41250000000000497, 2.886751345948126879, 4.999999999999999112 ) ) ;
#21352 = CARTESIAN_POINT ( 'NONE',  ( -3.999999999999999556, 18.08750000000000213, 27.69059892324149175 ) ) ;
#21353 = CARTESIAN_POINT ( 'NONE',  ( -3.000416591977282496E-16, 10.29687500061451644, -34.90005215228797653 ) ) ;
#21354 = CARTESIAN_POINT ( 'NONE',  ( 23.29687500061451644, -2.746126346562642428, -4.756430356249999214 ) ) ;
#21355 = CARTESIAN_POINT ( 'NONE',  ( 12.70312500061451821, 0.000000000000000000, 5.243569643749999010 ) ) ;
#21356 = CARTESIAN_POINT ( 'NONE',  ( 3.225000000000002309, 6.123233995736764310E-16, -4.999999999999998224 ) ) ;
#21357 = AXIS2_PLACEMENT_3D ( 'NONE', #18417, #40613, #29165 ) ;
#21358 = LINE ( 'NONE', #31358, #37227 ) ;
#21359 = CARTESIAN_POINT ( 'NONE',  ( 27.68437500061451573, -4.541064518000419881, 2.621784821874995952 ) ) ;
#21360 = CARTESIAN_POINT ( 'NONE',  ( 13.31250000000000178, 2.886751345948126879, 4.999999999999999112 ) ) ;
#21361 = CARTESIAN_POINT ( 'NONE',  ( 3.999999999999999112, 15.83750000122903501, 30.00000000000000000 ) ) ;
#21362 = CARTESIAN_POINT ( 'NONE',  ( 11.13750000122903216, 4.330127018922191873, 2.499999999999999556 ) ) ;
#21363 = CARTESIAN_POINT ( 'NONE',  ( 22.62187500061451573, 3.027376345333611329, 5.243569643749999010 ) ) ;
#21364 = CARTESIAN_POINT ( 'NONE',  ( 13.92187500061451644, 3.027376345333613106, -5.243569643749998122 ) ) ;
#21365 = CARTESIAN_POINT ( 'NONE',  ( 3.972658874145789110, 3.036112888163414514, -4.275165627105516286 ) ) ;
#21366 = ORIENTED_EDGE ( 'NONE', *, *, #38881, .T. ) ;
#21367 = CARTESIAN_POINT ( 'NONE',  ( 18.29062500061451502, -3.027376345333610441, -5.243569643749999898 ) ) ;
#21368 = CARTESIAN_POINT ( 'NONE',  ( 29.06250000122903288, 4.330127018922192761, -2.499999999999997780 ) ) ;
#21369 = CARTESIAN_POINT ( 'NONE',  ( 14.29687500061451821, -3.027376345333610441, -5.243569643749999898 ) ) ;
#21370 = CARTESIAN_POINT ( 'NONE',  ( 7.285825834671762338E-16, 10.00000000000000000, -24.00000000000000000 ) ) ;
#21371 = CARTESIAN_POINT ( 'NONE',  ( 19.86562500061451786, 3.027376345333611329, 5.243569643749999010 ) ) ;
#21372 = CARTESIAN_POINT ( 'NONE',  ( 1.592000809091587073E-14, 16.73750000000000071, -34.00000000000000000 ) ) ;
#21373 = CARTESIAN_POINT ( 'NONE',  ( 29.82187500061451502, 3.027376345333611329, 5.243569643749999010 ) ) ;
#21374 = CARTESIAN_POINT ( 'NONE',  ( -4.243569643749997233, 13.09062500061451750, 32.45002607614398471 ) ) ;
#21375 = CARTESIAN_POINT ( 'NONE',  ( 16.88437500061451502, -4.541064518000419881, 2.621784821874995952 ) ) ;
#21376 = CARTESIAN_POINT ( 'NONE',  ( 13.53750000122903430, -4.330127018922194537, 2.499999999999995559 ) ) ;
#21377 = CARTESIAN_POINT ( 'NONE',  ( 10.69687500061451679, -2.746126346562641984, -4.756430356249999214 ) ) ;
#21378 = CARTESIAN_POINT ( 'NONE',  ( 2.121784821874999061, 18.35937500061451644, -33.67503911421598417 ) ) ;
#21379 = CARTESIAN_POINT ( 'NONE',  ( 20.85937500061451644, 0.000000000000000000, 5.243569643749999010 ) ) ;
#21380 = CARTESIAN_POINT ( 'NONE',  ( 23.47500000122903430, -5.773502691896255534, -1.060575238724906372E-15 ) ) ;
#21381 = CARTESIAN_POINT ( 'NONE',  ( 16.20937500061451786, 4.541064518000418104, -2.621784821874998173 ) ) ;
#21382 = CARTESIAN_POINT ( 'NONE',  ( 12.55312500061451786, 4.541064518000418104, -2.621784821874998173 ) ) ;
#21383 = CARTESIAN_POINT ( 'NONE',  ( -4.243569643749997233, 12.24687500061451928, 32.45002607614398471 ) ) ;
#21384 = CARTESIAN_POINT ( 'NONE',  ( 17.57812500061451644, 4.541064518000418104, 2.621784821874999949 ) ) ;
#21385 = ORIENTED_EDGE ( 'NONE', *, *, #31048, .F. ) ;
#21386 = ORIENTED_EDGE ( 'NONE', *, *, #33660, .F. ) ;
#21387 = CARTESIAN_POINT ( 'NONE',  ( 22.68750000000000000, 5.773502691896255534, 3.535250795749688894E-16 ) ) ;
#21388 = CARTESIAN_POINT ( 'NONE',  ( 2.121784821874999061, 18.35937500061451644, -33.67503911421598417 ) ) ;
#21389 = LINE ( 'NONE', #16214, #5529 ) ;
#21390 = CARTESIAN_POINT ( 'NONE',  ( 23.50312500061451360, 0.000000000000000000, 5.243569643749999010 ) ) ;
#21391 = CARTESIAN_POINT ( 'NONE',  ( 6.253125000614517148, 4.541064518000418104, -2.621784821874998173 ) ) ;
#21392 = CARTESIAN_POINT ( 'NONE',  ( 17.77500000122903145, 2.886751345948129099, -4.999999999999998224 ) ) ;
#21393 = CARTESIAN_POINT ( 'NONE',  ( 23.57812500061451289, -4.541064518000419881, 2.621784821874995952 ) ) ;
#21394 = CARTESIAN_POINT ( 'NONE',  ( 24.11249999999999716, 2.886751345948126879, 4.999999999999999112 ) ) ;
#21395 = CARTESIAN_POINT ( 'NONE',  ( 25.15312500061451217, 4.541064518000418104, -2.621784821874998173 ) ) ;
#21396 = CARTESIAN_POINT ( 'NONE',  ( 6.740625000614516082, 6.054752690667223547, 3.707466751127219781E-16 ) ) ;
#21397 = ORIENTED_EDGE ( 'NONE', *, *, #15860, .F. ) ;
#21398 = EDGE_CURVE ( 'NONE', #24437, #10170, #3581, .T. ) ;
#21399 = CARTESIAN_POINT ( 'NONE',  ( 24.21562500061451573, 3.027376345333613106, -5.243569643749998122 ) ) ;
#21400 = CARTESIAN_POINT ( 'NONE',  ( -1.999999999999999112, 13.04374999877096641, 26.53589838486224650 ) ) ;
#21401 = CARTESIAN_POINT ( 'NONE',  ( 10.65937500061451715, -4.119189519843965641, -2.378215178125001383 ) ) ;
#21402 = CYLINDRICAL_SURFACE ( 'NONE', #40612, 4.999999999999998224 ) ;
#21403 = CARTESIAN_POINT ( 'NONE',  ( 2.000000000000001332, 14.86250000122903536, -26.53589838486224650 ) ) ;
#21404 = CARTESIAN_POINT ( 'NONE',  ( -2.121784821874999949, 19.78437500061451715, -33.67503911421598417 ) ) ;
#21405 = CARTESIAN_POINT ( 'NONE',  ( 11.28749999999999787, -2.886751345948125991, -5.000000000000000000 ) ) ;
#21406 = CARTESIAN_POINT ( 'NONE',  ( 11.82187500061451679, 3.027376345333611329, 5.243569643749999010 ) ) ;
#21407 = CARTESIAN_POINT ( 'NONE',  ( 6.787500001229032520, -4.330127018922194537, 2.499999999999995559 ) ) ;
#21408 = CARTESIAN_POINT ( 'NONE',  ( 15.45937500061451608, 0.000000000000000000, 5.243569643749999010 ) ) ;
#21409 = CARTESIAN_POINT ( 'NONE',  ( 6.271875000614517859, 3.027376345333613106, -5.243569643749998122 ) ) ;
#21410 = CYLINDRICAL_SURFACE ( 'NONE', #24353, 4.999999999999998224 ) ;
#21411 = FACE_OUTER_BOUND ( 'NONE', #65876, .T. ) ;
#21412 = CARTESIAN_POINT ( 'NONE',  ( 12.53437500061451537, 6.421520780324663323E-16, -5.243569643749999010 ) ) ;
#21413 = CARTESIAN_POINT ( 'NONE',  ( 13.12500000000000178, 6.123233995736764310E-16, -4.999999999999998224 ) ) ;
#21414 = CARTESIAN_POINT ( 'NONE',  ( 22.49062500061451431, 6.054752690667223547, 3.707466751127219781E-16 ) ) ;
#21415 = CARTESIAN_POINT ( 'NONE',  ( 5.810221930991193690E-16, 17.95624999877096428, 26.00000000000000000 ) ) ;
#21416 = CARTESIAN_POINT ( 'NONE',  ( -5.810221930991193690E-16, 10.43750000000000000, -34.00000000000000000 ) ) ;
#21417 = CARTESIAN_POINT ( 'NONE',  ( 24.15937500061451715, -4.541064518000417216, -2.621784821875001281 ) ) ;
#21418 = DIRECTION ( 'NONE',  ( -0.000000000000000000, -1.000000000000000000, -0.000000000000000000 ) ) ;
#21419 = CARTESIAN_POINT ( 'NONE',  ( 29.06250000122903288, 4.330127018922192761, -2.499999999999997780 ) ) ;
#21420 = CARTESIAN_POINT ( 'NONE',  ( 20.37187500061451217, -4.119189519843968306, 2.378215178124996054 ) ) ;
#21421 = CARTESIAN_POINT ( 'NONE',  ( 24.21562500061451573, 3.027376345333613106, -5.243569643749998122 ) ) ;
#21422 = CARTESIAN_POINT ( 'NONE',  ( 18.25312500061451715, -4.541064518000417216, -2.621784821875001281 ) ) ;
#21423 = CARTESIAN_POINT ( 'NONE',  ( 13.96875000122903465, -5.773502691896255534, -1.060575238724906372E-15 ) ) ;
#21424 = CARTESIAN_POINT ( 'NONE',  ( 14.03437500061451715, 4.541064518000418104, 2.621784821874999949 ) ) ;
#21425 = FACE_OUTER_BOUND ( 'NONE', #25476, .T. ) ;
#21426 = CARTESIAN_POINT ( 'NONE',  ( 27.15000000122902790, -2.886751345948125991, -5.000000000000000000 ) ) ;
#21427 = CARTESIAN_POINT ( 'NONE',  ( 2.896875000614518747, -3.027376345333614438, 5.243569643749998122 ) ) ;
#21428 = CARTESIAN_POINT ( 'NONE',  ( 13.65937500061451715, 0.000000000000000000, 5.243569643749999010 ) ) ;
#21429 = CARTESIAN_POINT ( 'NONE',  ( 21.22500000000000142, 6.123233995736764310E-16, -4.999999999999998224 ) ) ;
#21430 = CARTESIAN_POINT ( 'NONE',  ( -3.999999999999999112, 11.45000000000000107, 30.00000000000000000 ) ) ;
#21431 = CARTESIAN_POINT ( 'NONE',  ( 4.650000001229035895, -2.886751345948125991, -5.000000000000000000 ) ) ;
#21432 = CARTESIAN_POINT ( 'NONE',  ( 24.45937500061451786, 0.000000000000000000, 5.243569643749999010 ) ) ;
#21433 = CARTESIAN_POINT ( 'NONE',  ( 16.73437500061451644, 4.541064518000418104, 2.621784821874999949 ) ) ;
#21434 = CARTESIAN_POINT ( 'NONE',  ( 3.756430356250000546, 15.94062499938548427, 27.83122392262697886 ) ) ;
#21435 = CARTESIAN_POINT ( 'NONE',  ( 28.01249999999999574, 2.886751345948129099, -4.999999999999998224 ) ) ;
#21436 = CARTESIAN_POINT ( 'NONE',  ( 6.524999999999999467, 4.330127018922191873, 2.499999999999999556 ) ) ;
#21437 = CARTESIAN_POINT ( 'NONE',  ( 8.071875000614515017, 4.119189519843966529, 2.378215178124999607 ) ) ;
#21438 = CARTESIAN_POINT ( 'NONE',  ( 19.60312500061451502, -4.541064518000417216, -2.621784821875001281 ) ) ;
#21439 = CARTESIAN_POINT ( 'NONE',  ( 10.08749999999999858, 5.773502691896255534, 3.535250795749688894E-16 ) ) ;
#21440 = CARTESIAN_POINT ( 'NONE',  ( 4.790625000614518569, -3.027376345333610441, -5.243569643749999898 ) ) ;
#21441 = CARTESIAN_POINT ( 'NONE',  ( 19.34999999999999787, -4.330127018922190985, -2.500000000000001332 ) ) ;
#21442 = EDGE_CURVE ( 'NONE', #59726, #55474, #11121, .T. ) ;
#21443 = CARTESIAN_POINT ( 'NONE',  ( 1.071796769724485232, 16.58615380933862937, 25.99999999999999645 ) ) ;
#21444 = CARTESIAN_POINT ( 'NONE',  ( 22.38750000122903216, 4.330127018922191873, 2.499999999999999556 ) ) ;
#21445 = CARTESIAN_POINT ( 'NONE',  ( 5.681944431425976383, 8.230953001180113304, 28.03323168659990117 ) ) ;
#21446 = CARTESIAN_POINT ( 'NONE',  ( 28.88437500061451502, 4.541064518000418104, 2.621784821874999949 ) ) ;
#21447 = ORIENTED_EDGE ( 'NONE', *, *, #721, .T. ) ;
#21448 = CARTESIAN_POINT ( 'NONE',  ( 16.75312500061451715, 0.000000000000000000, 5.243569643749999010 ) ) ;
#21449 = CARTESIAN_POINT ( 'NONE',  ( 24.21562500061451573, 3.027376345333613106, -5.243569643749998122 ) ) ;
#21450 = CARTESIAN_POINT ( 'NONE',  ( 25.73437500061451644, 4.541064518000418104, 2.621784821874999949 ) ) ;
#21451 = B_SPLINE_CURVE_WITH_KNOTS ( 'NONE', 1,
 ( #724, #50598 ),
 .UNSPECIFIED., .F., .F.,
 ( 2, 2 ),
 ( 0.000000000000000000, 1.000000000000000000 ),
 .UNSPECIFIED. ) ;
#21452 = CARTESIAN_POINT ( 'NONE',  ( 5.775000000000002132, -4.330127018922194537, 2.499999999999995559 ) ) ;
#21453 = CARTESIAN_POINT ( 'NONE',  ( 9.928125000614517859, 4.541064518000418104, 2.621784821874999949 ) ) ;
#21454 = CARTESIAN_POINT ( 'NONE',  ( 25.56562500061452070, 3.027376345333613106, -5.243569643749998122 ) ) ;
#21455 = CARTESIAN_POINT ( 'NONE',  ( 14.59687500061452070, -3.027376345333614438, 5.243569643749998122 ) ) ;
#21456 = CARTESIAN_POINT ( 'NONE',  ( 18.60937500061451644, 0.000000000000000000, 5.243569643749999010 ) ) ;
#21457 = CARTESIAN_POINT ( 'NONE',  ( 4.437233173123817487, 2.304579454652033732, -4.709995530123128660 ) ) ;
#21458 = CARTESIAN_POINT ( 'NONE',  ( -2.121784821874999949, 10.78437500061451715, 26.32496088578401938 ) ) ;
#21459 = CARTESIAN_POINT ( 'NONE',  ( 21.52500000122903145, 2.886751345948126879, 4.999999999999999112 ) ) ;
#21460 = CARTESIAN_POINT ( 'NONE',  ( 18.08437500061451431, 4.119189519843966529, 2.378215178124999607 ) ) ;
#21461 = CARTESIAN_POINT ( 'NONE',  ( 13.11562500061451786, 3.027376345333611329, 5.243569643749999010 ) ) ;
#21462 = APPLICATION_CONTEXT ( 'automotive_design' ) ;
#21463 = CARTESIAN_POINT ( 'NONE',  ( 7.509375000614517681, -4.541064518000417216, -2.621784821875001281 ) ) ;
#21464 = CARTESIAN_POINT ( 'NONE',  ( 7.921875000614517326, -6.054752690667223547, -1.112240025338166033E-15 ) ) ;
#21465 = ORIENTED_EDGE ( 'NONE', *, *, #30679, .T. ) ;
#21466 = CARTESIAN_POINT ( 'NONE',  ( 27.90937500061451715, 4.541064518000418104, -2.621784821874998173 ) ) ;
#21467 = CARTESIAN_POINT ( 'NONE',  ( 18.66562500061451146, -6.054752690667223547, -1.112240025338166033E-15 ) ) ;
#21468 = CARTESIAN_POINT ( 'NONE',  ( 3.965625000614515727, 3.027376345333613106, -5.243569643749998122 ) ) ;
#21469 =( BOUNDED_CURVE ( )  B_SPLINE_CURVE ( 2, ( #47591, #41684, #18407, #40973, #24323, #18766, #46872 ),
 .UNSPECIFIED., .F., .F. ) 
 B_SPLINE_CURVE_WITH_KNOTS ( ( 3, 2, 2, 3 ),
 ( 0.9249999999999999334, 0.9277777777777777013, 0.9305555555555555802, 0.9326049216113281304 ),
 .UNSPECIFIED. ) 
 CURVE ( )  GEOMETRIC_REPRESENTATION_ITEM ( )  RATIONAL_B_SPLINE_CURVE ( ( 1.000000000000005329, 0.8660254037844333785, 1.000000000000000000, 0.8660254037844387076, 1.000000000000000000, 0.9011573236647978380, 0.9481613218646109953 ) ) 
 REPRESENTATION_ITEM ( '' )  );
#21470 = CARTESIAN_POINT ( 'NONE',  ( 4.321875000614517681, -6.054752690667223547, -1.112240025338166033E-15 ) ) ;
#21471 = VECTOR ( 'NONE', #53281, 1000.000000000000000 ) ;
#21472 = CARTESIAN_POINT ( 'NONE',  ( 24.98437500061451644, -4.541064518000419881, 2.621784821874995952 ) ) ;
#21473 = CARTESIAN_POINT ( 'NONE',  ( 18.74062500061451431, -3.027376345333610441, -5.243569643749999898 ) ) ;
#21474 = CARTESIAN_POINT ( 'NONE',  ( -3.999999999999999112, 12.34999999999999964, 30.00000000000000000 ) ) ;
#21475 = CARTESIAN_POINT ( 'NONE',  ( 24.02812500061451573, -4.541064518000419881, 2.621784821874995952 ) ) ;
#21476 = CARTESIAN_POINT ( 'NONE',  ( 5.100000001229034297, -2.886751345948125991, -5.000000000000000000 ) ) ;
#21477 = VERTEX_POINT ( 'NONE', #54048 ) ;
#21478 = CARTESIAN_POINT ( 'NONE',  ( 29.32499999999999929, 6.123233995736764310E-16, -4.999999999999998224 ) ) ;
#21479 = CARTESIAN_POINT ( 'NONE',  ( 1.999999999999998668, 15.35000000000000142, -33.46410161513775705 ) ) ;
#21480 = CARTESIAN_POINT ( 'NONE',  ( 2.655984681222220721E-16, 16.01562499938548356, 25.66244784525396483 ) ) ;
#21481 = EDGE_CURVE ( 'NONE', #58840, #50518, #49318, .T. ) ;
#21482 = CARTESIAN_POINT ( 'NONE',  ( 5.221875000614519813, -6.054752690667223547, -1.112240025338166033E-15 ) ) ;
#21483 = CARTESIAN_POINT ( 'NONE',  ( 29.76562500061451644, 3.027376345333611329, 5.243569643749999010 ) ) ;
#21484 = CARTESIAN_POINT ( 'NONE',  ( 12.21562500061451573, 3.027376345333611329, 5.243569643749999010 ) ) ;
#21485 = CARTESIAN_POINT ( 'NONE',  ( 5.634375000614519458, -4.541064518000419881, 2.621784821874995952 ) ) ;
#21486 = CARTESIAN_POINT ( 'NONE',  ( 25.76250000122903216, -4.330127018922190985, -2.500000000000001332 ) ) ;
#21487 = CARTESIAN_POINT ( 'NONE',  ( 15.68437500061451573, 6.421520780324663323E-16, -5.243569643749999010 ) ) ;
#21488 = CARTESIAN_POINT ( 'NONE',  ( 28.71562500061451573, 3.027376345333613106, -5.243569643749998122 ) ) ;
#21489 = CARTESIAN_POINT ( 'NONE',  ( 29.21249999999999858, -5.773502691896255534, -1.060575238724906372E-15 ) ) ;
#21490 = CARTESIAN_POINT ( 'NONE',  ( 3.815625000614518036, -6.054752690667223547, -1.112240025338166033E-15 ) ) ;
#21491 = CARTESIAN_POINT ( 'NONE',  ( 15.89062500061451289, -3.027376345333614438, 5.243569643749998122 ) ) ;
#21492 = ORIENTED_EDGE ( 'NONE', *, *, #52383, .F. ) ;
#21493 = CARTESIAN_POINT ( 'NONE',  ( 10.07812500061451644, -4.541064518000419881, 2.621784821874995952 ) ) ;
#21494 = CARTESIAN_POINT ( 'NONE',  ( 7.940625000614518036, -3.027376345333610441, -5.243569643749999898 ) ) ;
#21495 = CARTESIAN_POINT ( 'NONE',  ( 19.65937500061451360, -4.119189519843965641, -2.378215178125001383 ) ) ;
#21496 = CARTESIAN_POINT ( 'NONE',  ( 9.712500000000002132, 2.886751345948126879, 4.999999999999999112 ) ) ;
#21497 = CARTESIAN_POINT ( 'NONE',  ( 3.150000001229034119, -2.886751345948129988, 4.999999999999997335 ) ) ;
#21498 = CARTESIAN_POINT ( 'NONE',  ( 18.37500000000000355, -4.330127018922194537, 2.499999999999995559 ) ) ;
#21499 = CARTESIAN_POINT ( 'NONE',  ( 19.43437500061451928, 4.541064518000418104, 2.621784821874999949 ) ) ;
#21500 = CARTESIAN_POINT ( 'NONE',  ( 14.51250000122903394, -4.330127018922190985, -2.500000000000001332 ) ) ;
#21501 = CARTESIAN_POINT ( 'NONE',  ( 20.40000000000000213, 4.330127018922192761, -2.499999999999997780 ) ) ;
#21502 = CARTESIAN_POINT ( 'NONE',  ( 4.243569643749999010, 17.36562500061451786, -32.45002607614398471 ) ) ;
#21503 = CARTESIAN_POINT ( 'NONE',  ( 22.08749999999999858, -2.886751345948159742, -4.999999999999942268 ) ) ;
#21504 = CARTESIAN_POINT ( 'NONE',  ( 19.25625000122903430, 0.000000000000000000, 4.999999999999998224 ) ) ;
#21505 = CARTESIAN_POINT ( 'NONE',  ( 28.56562500061451715, -6.054752690667223547, -1.112240025338166033E-15 ) ) ;
#21506 = CARTESIAN_POINT ( 'NONE',  ( 20.06250000122903643, 4.330127018922192761, -2.499999999999997780 ) ) ;
#21507 = CARTESIAN_POINT ( 'NONE',  ( 12.87187500061451750, -6.054752690667223547, -1.112240025338166033E-15 ) ) ;
#21508 = CARTESIAN_POINT ( 'NONE',  ( 26.02499999999999858, -4.330127018922194537, 2.499999999999995559 ) ) ;
#21509 = CARTESIAN_POINT ( 'NONE',  ( 9.515625000614518214, 3.027376345333611329, 5.243569643749999010 ) ) ;
#21510 = VECTOR ( 'NONE', #60611, 1000.000000000000000 ) ;
#21511 = CARTESIAN_POINT ( 'NONE',  ( 26.93437500061451573, 5.492252693125287522, 3.363034840372157021E-16 ) ) ;
#21512 = CARTESIAN_POINT ( 'NONE',  ( 22.17187500061451644, 3.027376345333611329, 5.243569643749999010 ) ) ;
#21513 = CARTESIAN_POINT ( 'NONE',  ( 13.80937500061451395, 2.746126346562645981, -4.756430356249997438 ) ) ;
#21514 = CARTESIAN_POINT ( 'NONE',  ( 8.503125000614515372, 4.541064518000418104, -2.621784821874998173 ) ) ;
#21515 = CARTESIAN_POINT ( 'NONE',  ( 12.83437500061451786, -4.541064518000419881, 2.621784821874995952 ) ) ;
#21516 = ORIENTED_EDGE ( 'NONE', *, *, #3316, .F. ) ;
#21517 = CARTESIAN_POINT ( 'NONE',  ( 24.90937500061451715, 0.000000000000000000, 5.243569643749999010 ) ) ;
#21518 = CARTESIAN_POINT ( 'NONE',  ( 1.095284332908923686, 4.886121113889972278, -33.85685977295008087 ) ) ;
#21519 = CARTESIAN_POINT ( 'NONE',  ( 5.137500000000000178, 5.773502691896255534, 3.535250795749688894E-16 ) ) ;
#21520 = CARTESIAN_POINT ( 'NONE',  ( 15.26250000122903216, 0.000000000000000000, 4.999999999999998224 ) ) ;
#21521 = CARTESIAN_POINT ( 'NONE',  ( 1.999999999999998668, 15.35000000000000142, -33.46410161513775705 ) ) ;
#21522 = CARTESIAN_POINT ( 'NONE',  ( 19.04999999999999716, 4.330127018922192761, -2.499999999999997780 ) ) ;
#21523 = ORIENTED_EDGE ( 'NONE', *, *, #51187, .T. ) ;
#21524 = CARTESIAN_POINT ( 'NONE',  ( 13.12500000000000178, 6.123233995736764310E-16, -4.999999999999998224 ) ) ;
#21525 = CARTESIAN_POINT ( 'NONE',  ( 15.67500000000000071, -4.330127018922194537, 2.499999999999995559 ) ) ;
#21526 = CARTESIAN_POINT ( 'NONE',  ( 13.50000000122903288, -2.886751345948129988, 4.999999999999997335 ) ) ;
#21527 = CARTESIAN_POINT ( 'NONE',  ( 10.37812500061451715, 4.541064518000418104, 2.621784821874999949 ) ) ;
#21528 = EDGE_CURVE ( 'NONE', #59300, #11494, #7944, .T. ) ;
#21529 = ORIENTED_EDGE ( 'NONE', *, *, #56383, .T. ) ;
#21530 = CARTESIAN_POINT ( 'NONE',  ( 8.775000000000002132, 4.330127018922191873, 2.499999999999999556 ) ) ;
#21531 = CARTESIAN_POINT ( 'NONE',  ( -3.137519842735245283E-14, 11.22500000122903430, -26.00000000000000711 ) ) ;
#21532 = CARTESIAN_POINT ( 'NONE',  ( 4.243569643749999898, 14.23437500061451821, -30.00000000000000000 ) ) ;
#21533 = CARTESIAN_POINT ( 'NONE',  ( 4.078125000614517326, 4.541064518000418104, 2.621784821874999949 ) ) ;
#21534 = CARTESIAN_POINT ( 'NONE',  ( -3.756430356249999214, 14.62812499938548427, 27.83122392262697176 ) ) ;
#21535 = CARTESIAN_POINT ( 'NONE',  ( 9.037499999999999645, -2.886751345948125991, -5.000000000000000000 ) ) ;
#21536 = CARTESIAN_POINT ( 'NONE',  ( 16.25625000122903074, -4.330127018922190985, -2.500000000000001332 ) ) ;
#21537 = ORIENTED_EDGE ( 'NONE', *, *, #23281, .F. ) ;
#21538 = CARTESIAN_POINT ( 'NONE',  ( 24.32812500061451289, 4.541064518000418104, 2.621784821874999949 ) ) ;
#21539 = CARTESIAN_POINT ( 'NONE',  ( 29.32499999999999929, 6.123233995736764310E-16, -4.999999999999998224 ) ) ;
#21540 = CARTESIAN_POINT ( 'NONE',  ( -3.756430356250000102, 19.16562499938548214, 30.00000000000000000 ) ) ;
#21541 = CARTESIAN_POINT ( 'NONE',  ( 21.42187500061451644, -6.054752690667223547, -1.112240025338166033E-15 ) ) ;
#21542 = EDGE_CURVE ( 'NONE', #14527, #50794, #18649, .T. ) ;
#21543 = CARTESIAN_POINT ( 'NONE',  ( 20.20312500061451644, 4.541064518000418104, -2.621784821874998173 ) ) ;
#21544 = CARTESIAN_POINT ( 'NONE',  ( -4.243569643749999898, 11.25312500061459531, -30.00000000000000000 ) ) ;
#21545 = CARTESIAN_POINT ( 'NONE',  ( 6.103125000614515905, -4.541064518000417216, -2.621784821875001281 ) ) ;
#21546 = CARTESIAN_POINT ( 'NONE',  ( 4.640625000614518214, -3.027376345333614438, 5.243569643749998122 ) ) ;
#21547 = CARTESIAN_POINT ( 'NONE',  ( 25.43437500061451573, -4.119189519843968306, 2.378215178124996054 ) ) ;
#21548 = CARTESIAN_POINT ( 'NONE',  ( 20.84062500061451217, -3.027376345333614438, 5.243569643749998122 ) ) ;
#21549 = CARTESIAN_POINT ( 'NONE',  ( 0.000000000000000000, 20.00000000000000000, -30.00000000000000000 ) ) ;
#21550 = CARTESIAN_POINT ( 'NONE',  ( -3.756430356249999214, 17.32812499938548356, 27.83122392262697531 ) ) ;
#21552 = ADVANCED_FACE ( 'NONE', ( #8975 ), #18935, .T. ) ;
#21551 = CARTESIAN_POINT ( 'NONE',  ( 14.25937500061451679, -4.541064518000417216, -2.621784821875001281 ) ) ;
#21553 = CARTESIAN_POINT ( 'NONE',  ( 14.37187500061451928, 3.027376345333613106, -5.243569643749998122 ) ) ;
#21554 = CARTESIAN_POINT ( 'NONE',  ( 22.50937500061451857, 4.541064518000418104, -2.621784821874998173 ) ) ;
#21555 = EDGE_LOOP ( 'NONE', ( #30871, #30996, #55384, #30790 ) ) ;
#21556 = CARTESIAN_POINT ( 'NONE',  ( 2.121784821875001281, 11.90937500061451892, 33.67503911421598417 ) ) ;
#21557 = CARTESIAN_POINT ( 'NONE',  ( 27.07499999999999929, 6.123233995736764310E-16, -4.999999999999998224 ) ) ;
#21558 = CARTESIAN_POINT ( 'NONE',  ( 25.71562500061451573, 3.027376345333611329, 5.243569643749999010 ) ) ;
#21559 = CARTESIAN_POINT ( 'NONE',  ( 25.64062500061451644, 6.054752690667223547, 3.707466751127219781E-16 ) ) ;
#21560 = CARTESIAN_POINT ( 'NONE',  ( 65.00000000000000000, -6.363961030678871644, 6.363961030678982667 ) ) ;
#21561 = CARTESIAN_POINT ( 'NONE',  ( 3.999999999999998668, 18.46249999999999858, 27.69059892324149175 ) ) ;
#21562 = CARTESIAN_POINT ( 'NONE',  ( 3.646875000614520079, 6.054752690667223547, 3.707466751127219781E-16 ) ) ;
#21563 = DIRECTION ( 'NONE',  ( 1.000000000000000000, 0.000000000000000000, 0.000000000000000000 ) ) ;
#21564 = CARTESIAN_POINT ( 'NONE',  ( 10.72500000122903252, 2.886751345948126879, 4.999999999999999112 ) ) ;
#21565 = CARTESIAN_POINT ( 'NONE',  ( 8.287500001229034297, 6.123233995736764310E-16, -4.999999999999998224 ) ) ;
#21566 = CARTESIAN_POINT ( 'NONE',  ( 3.553125000614516082, 4.541064518000418104, -2.621784821874998173 ) ) ;
#21567 = CARTESIAN_POINT ( 'NONE',  ( 4.000000000000000000, 16.94374999877096499, 30.00000000000000000 ) ) ;
#21568 = CARTESIAN_POINT ( 'NONE',  ( 19.18125000122903501, 4.330127018922191873, 2.499999999999999556 ) ) ;
#21569 = CARTESIAN_POINT ( 'NONE',  ( 12.42187500061451821, -6.054752690667223547, -1.112240025338166033E-15 ) ) ;
#21570 = DIRECTION ( 'NONE',  ( -0.000000000000000000, -1.000000000000000000, -0.000000000000000000 ) ) ;
#21571 = VERTEX_POINT ( 'NONE', #37038 ) ;
#21572 = CARTESIAN_POINT ( 'NONE',  ( 18.74062500061451431, -3.027376345333610441, -5.243569643749999898 ) ) ;
#21573 = CARTESIAN_POINT ( 'NONE',  ( 13.35937500061451821, -4.541064518000417216, -2.621784821875001281 ) ) ;
#21574 = CARTESIAN_POINT ( 'NONE',  ( 5.915625000614515905, 3.027376345333611329, 5.243569643749999010 ) ) ;
#21575 = CARTESIAN_POINT ( 'NONE',  ( 22.05937500061451573, 4.541064518000418104, -2.621784821874998173 ) ) ;
#21576 = CARTESIAN_POINT ( 'NONE',  ( 6.028125000614517504, -4.541064518000419881, 2.621784821874995952 ) ) ;
#21577 = CARTESIAN_POINT ( 'NONE',  ( -2.000000000000001776, 16.34374999877096712, 33.46410161513775705 ) ) ;
#21578 = CARTESIAN_POINT ( 'NONE',  ( 6.825000001229034829, -5.773502691896255534, -1.060575238724906372E-15 ) ) ;
#21579 = CARTESIAN_POINT ( 'NONE',  ( 21.96562500061451573, 3.027376345333613106, -5.243569643749998122 ) ) ;
#21580 = CARTESIAN_POINT ( 'NONE',  ( -3.999999999999997335, 17.00000000122903288, -27.69059892324149175 ) ) ;
#21581 = CARTESIAN_POINT ( 'NONE',  ( 9.075000001229033941, -5.773502691896255534, -1.060575238724906372E-15 ) ) ;
#21582 = CARTESIAN_POINT ( 'NONE',  ( 16.67812500061451786, 4.541064518000418104, 2.621784821874999949 ) ) ;
#21583 = CARTESIAN_POINT ( 'NONE',  ( 15.14062500061451644, -3.027376345333610441, -5.243569643749999898 ) ) ;
#21584 = CARTESIAN_POINT ( 'NONE',  ( 25.62187500061451573, 2.746126346562645981, -4.756430356249997438 ) ) ;
#21585 = CARTESIAN_POINT ( 'NONE',  ( 15.86250000000000249, 2.886751345948129099, -4.999999999999998224 ) ) ;
#21586 = CARTESIAN_POINT ( 'NONE',  ( 10.72500000122903252, 2.886751345948126879, 4.999999999999999112 ) ) ;
#21587 = EDGE_CURVE ( 'NONE', #12198, #59156, #38709, .T. ) ;
#21588 = CARTESIAN_POINT ( 'NONE',  ( 9.215625000614515727, -6.054752690667223547, -1.112240025338166033E-15 ) ) ;
#21589 = CARTESIAN_POINT ( 'NONE',  ( 10.94062500061451537, -3.027376345333614438, 5.243569643749998122 ) ) ;
#21590 = CARTESIAN_POINT ( 'NONE',  ( 21.33750000122903145, 6.123233995736764310E-16, -4.999999999999998224 ) ) ;
#21591 = CARTESIAN_POINT ( 'NONE',  ( 4.243569643749999010, 14.27187500061451964, -32.45002607614398471 ) ) ;
#21592 = CARTESIAN_POINT ( 'NONE',  ( 19.54687500061451644, -3.027376345333614438, 5.243569643749998122 ) ) ;
#21593 = CARTESIAN_POINT ( 'NONE',  ( 30.00000000000000000, 0.000000000000000000, 0.000000000000000000 ) ) ;
#21594 = CARTESIAN_POINT ( 'NONE',  ( 4.612500001229032698, -4.330127018922190985, -2.500000000000001332 ) ) ;
#21595 = CARTESIAN_POINT ( 'NONE',  ( 3.609375000614516882, 4.541064518000418104, -2.621784821874998173 ) ) ;
#21596 = CARTESIAN_POINT ( 'NONE',  ( 19.99687500061451573, -3.027376345333614438, 5.243569643749998122 ) ) ;
#21597 = CARTESIAN_POINT ( 'NONE',  ( 5.062500000000002665, 2.886751345948196157, -4.999999999999881872 ) ) ;
#21598 = CARTESIAN_POINT ( 'NONE',  ( 16.04062500061451857, -3.027376345333610441, -5.243569643749999898 ) ) ;
#21599 = CARTESIAN_POINT ( 'NONE',  ( 11.41875000122903394, 2.886751345948129099, -4.999999999999998224 ) ) ;
#21600 = CARTESIAN_POINT ( 'NONE',  ( -1.487416814333745711E-14, 14.82500000122903572, 34.00000000000000000 ) ) ;
#21601 = CARTESIAN_POINT ( 'NONE',  ( 1.626862140677534273E-15, 13.81250000000000000, 34.00000000000000000 ) ) ;
#21602 = CARTESIAN_POINT ( 'NONE',  ( 29.59687500061451715, -3.027376345333610441, -5.243569643749999898 ) ) ;
#21603 = CARTESIAN_POINT ( 'NONE',  ( 21.19687500061451502, 0.000000000000000000, 4.756430356249998326 ) ) ;
#21604 = CARTESIAN_POINT ( 'NONE',  ( 14.80312500061451608, 4.541064518000418104, -2.621784821874998173 ) ) ;
#21605 = CARTESIAN_POINT ( 'NONE',  ( 13.77187500061451786, -6.054752690667223547, -1.112240025338166033E-15 ) ) ;
#21606 = ORIENTED_EDGE ( 'NONE', *, *, #38374, .T. ) ;
#21607 = CARTESIAN_POINT ( 'NONE',  ( 9.299999999999998934, 0.000000000000000000, 4.999999999999998224 ) ) ;
#21608 = CARTESIAN_POINT ( 'NONE',  ( 23.65312500061451573, -4.541064518000417216, -2.621784821875001281 ) ) ;
#21609 = DIRECTION ( 'NONE',  ( 0.000000000000000000, 0.000000000000000000, -1.000000000000000000 ) ) ;
#21610 = CARTESIAN_POINT ( 'NONE',  ( 14.58750000000000036, 5.773502691896255534, 3.535250795749688401E-16 ) ) ;
#21611 = CARTESIAN_POINT ( 'NONE',  ( 13.23750000000000071, 5.773502691896255534, 3.535250795749688894E-16 ) ) ;
#21612 = CARTESIAN_POINT ( 'NONE',  ( 24.33750000122903145, -4.330127018922194537, 2.499999999999995559 ) ) ;
#21613 = CARTESIAN_POINT ( 'NONE',  ( 17.87812500061451715, 6.421520780324663323E-16, -5.243569643749999010 ) ) ;
#21614 = EDGE_LOOP ( 'NONE', ( #43157, #21666 ) ) ;
#21615 = CARTESIAN_POINT ( 'NONE',  ( 20.54999999999999716, 0.000000000000000000, 4.999999999999998224 ) ) ;
#21616 =( BOUNDED_CURVE ( )  B_SPLINE_CURVE ( 2, ( #20844, #60729, #59999, #71838, #72927, #38203, #37840 ),
 .UNSPECIFIED., .F., .F. ) 
 B_SPLINE_CURVE_WITH_KNOTS ( ( 3, 2, 2, 3 ),
 ( 0.4000000000000000777, 0.4033333333333333215, 0.4066666666666666763, 0.4099999999999999201 ),
 .UNSPECIFIED. ) 
 CURVE ( )  GEOMETRIC_REPRESENTATION_ITEM ( )  RATIONAL_B_SPLINE_CURVE ( ( 0.9999999999999977796, 0.8660254037844409281, 1.000000000000000000, 0.8660254037844387076, 1.000000000000000000, 0.8660254037844409281, 0.9999999999999977796 ) ) 
 REPRESENTATION_ITEM ( '' )  );
#21617 = CARTESIAN_POINT ( 'NONE',  ( 21.27187500061451786, 3.027376345333611329, 5.243569643749999010 ) ) ;
#21618 = ORIENTED_EDGE ( 'NONE', *, *, #16392, .T. ) ;
#21619 = CARTESIAN_POINT ( 'NONE',  ( 10.19062500061451892, -3.027376345333610441, -5.243569643749999898 ) ) ;
#21620 = CARTESIAN_POINT ( 'NONE',  ( 13.02187500061451786, 4.119189519843966529, 2.378215178124999607 ) ) ;
#21621 = CARTESIAN_POINT ( 'NONE',  ( 15.97499999999999964, 4.330127018922191873, 2.499999999999999556 ) ) ;
#21622 = CARTESIAN_POINT ( 'NONE',  ( 24.07499999999999929, 4.330127018922191873, 2.499999999999999556 ) ) ;
#21623 = CARTESIAN_POINT ( 'NONE',  ( 3.518507979705963518, -3.552478233113482542, -3.764599296078968926 ) ) ;
#21624 = CARTESIAN_POINT ( 'NONE',  ( 3.796875000614517326, -3.027376345333614438, 5.243569643749998122 ) ) ;
#21625 = CARTESIAN_POINT ( 'NONE',  ( 29.03437500061451715, -4.541064518000419881, 2.621784821874995952 ) ) ;
#21626 = ORIENTED_EDGE ( 'NONE', *, *, #72282, .F. ) ;
#21627 = CARTESIAN_POINT ( 'NONE',  ( 25.49062500061451786, -3.027376345333610441, -5.243569643749999898 ) ) ;
#21628 = CARTESIAN_POINT ( 'NONE',  ( 27.75937500061451502, -4.541064518000417216, -2.621784821875001281 ) ) ;
#21629 = CARTESIAN_POINT ( 'NONE',  ( 5.810221930991193690E-16, 14.80624999877096570, 26.00000000000000000 ) ) ;
#21630 = CARTESIAN_POINT ( 'NONE',  ( 12.78749999999999964, 5.773502691896255534, 3.535250795749688894E-16 ) ) ;
#21631 = CARTESIAN_POINT ( 'NONE',  ( 12.40312500061451573, -4.541064518000417216, -2.621784821875001281 ) ) ;
#21632 = CARTESIAN_POINT ( 'NONE',  ( 3.849931240356728512, 3.190302406438068505, 3.849931240356827544 ) ) ;
#21633 = CARTESIAN_POINT ( 'NONE',  ( 2.000000000000001332, 19.25000000000000000, -26.53589838486224650 ) ) ;
#21634 = CARTESIAN_POINT ( 'NONE',  ( 27.66562500061451502, -6.054752690667223547, -1.112240025338166033E-15 ) ) ;
#21635 = CARTESIAN_POINT ( 'NONE',  ( 15.90000000122903501, -2.886751345948125991, -5.000000000000000000 ) ) ;
#21636 = DIRECTION ( 'NONE',  ( -0.000000000000000000, -1.000000000000000000, -0.000000000000000000 ) ) ;
#21637 = CARTESIAN_POINT ( 'NONE',  ( 14.44687500061451679, 5.492252693125287522, 3.363034840372157021E-16 ) ) ;
#21638 = CARTESIAN_POINT ( 'NONE',  ( 5.240625000614516971, -3.027376345333610441, -5.243569643749999898 ) ) ;
#21639 = CARTESIAN_POINT ( 'NONE',  ( 21.68437500061451573, 4.541064518000418104, 2.621784821874999949 ) ) ;
#21640 = CARTESIAN_POINT ( 'NONE',  ( 4.243569643749999010, 14.72187500061451715, 27.54997392385601174 ) ) ;
#21641 = EDGE_CURVE ( 'NONE', #70308, #26824, #41320, .T. ) ;
#21642 = CARTESIAN_POINT ( 'NONE',  ( 22.02187500061452141, 3.027376345333613106, -5.243569643749998122 ) ) ;
#21643 = CARTESIAN_POINT ( 'NONE',  ( 29.40937500061451715, 0.000000000000000000, 5.243569643749999010 ) ) ;
#21644 = CARTESIAN_POINT ( 'NONE',  ( -2.121784821874999949, 17.98437500061451999, 26.32496088578401938 ) ) ;
#21645 = CARTESIAN_POINT ( 'NONE',  ( 10.07812500061451644, -4.541064518000419881, 2.621784821874995952 ) ) ;
#21646 = DIRECTION ( 'NONE',  ( 0.000000000000000000, 0.000000000000000000, 1.000000000000000000 ) ) ;
#21647 = CARTESIAN_POINT ( 'NONE',  ( 6.534375000614517148, -4.541064518000419881, 2.621784821874995952 ) ) ;
#21648 = CARTESIAN_POINT ( 'NONE',  ( 23.47499999999999787, 6.123233995736764310E-16, -4.999999999999998224 ) ) ;
#21649 = CARTESIAN_POINT ( 'NONE',  ( 7.565625000614518036, 3.027376345333613106, -5.243569643749998122 ) ) ;
#21650 = CARTESIAN_POINT ( 'NONE',  ( 11.10937500061451644, -4.541064518000417216, -2.621784821875001281 ) ) ;
#21651 = CARTESIAN_POINT ( 'NONE',  ( 30.00000000000000000, 0.000000000000000000, 0.000000000000000000 ) ) ;
#21652 = CARTESIAN_POINT ( 'NONE',  ( 21.07500000122903572, 2.886751345948126879, 4.999999999999999112 ) ) ;
#21653 = CARTESIAN_POINT ( 'NONE',  ( 6.834375000614518747, 4.541064518000418104, 2.621784821874999949 ) ) ;
#21654 = CARTESIAN_POINT ( 'NONE',  ( 10.79062500061451679, 6.054752690667223547, 3.707466751127219781E-16 ) ) ;
#21655 = CARTESIAN_POINT ( 'NONE',  ( 25.59375000122903288, -2.886751345948129988, 4.999999999999997335 ) ) ;
#21656 = CARTESIAN_POINT ( 'NONE',  ( 19.62187500061451573, -6.054752690667223547, -1.112240025338166033E-15 ) ) ;
#21657 = CARTESIAN_POINT ( 'NONE',  ( 1.626862140677534273E-15, 15.61250000000000071, -26.00000000000000355 ) ) ;
#21658 = CARTESIAN_POINT ( 'NONE',  ( 11.95312500061451644, -4.541064518000417216, -2.621784821875001281 ) ) ;
#21659 = CARTESIAN_POINT ( 'NONE',  ( 21.63750000122903572, -4.330127018922194537, 2.499999999999995559 ) ) ;
#21660 = CARTESIAN_POINT ( 'NONE',  ( 28.35937500061451289, 4.541064518000418104, -2.621784821874998173 ) ) ;
#21661 = CARTESIAN_POINT ( 'NONE',  ( -4.243569643749999898, 12.17187500061451999, -32.45002607614398471 ) ) ;
#21662 = CARTESIAN_POINT ( 'NONE',  ( 14.25000000122903465, 5.773502691896255534, 3.535250795749688894E-16 ) ) ;
#21663 = CARTESIAN_POINT ( 'NONE',  ( -4.243569643749999898, 15.71562500061451573, -32.45002607614398471 ) ) ;
#21664 = CARTESIAN_POINT ( 'NONE',  ( 15.78750000122903430, -4.330127018922194537, 2.499999999999995559 ) ) ;
#21665 = CARTESIAN_POINT ( 'NONE',  ( 11.09062500061451573, -3.027376345333610441, -5.243569643749999898 ) ) ;
#21666 = ORIENTED_EDGE ( 'NONE', *, *, #18349, .T. ) ;
#21667 = CARTESIAN_POINT ( 'NONE',  ( 14.06250000000000000, 2.886751345948129099, -4.999999999999998224 ) ) ;
#21668 = CARTESIAN_POINT ( 'NONE',  ( 10.25625000122903252, 0.000000000000000000, 4.999999999999998224 ) ) ;
#21669 = CARTESIAN_POINT ( 'NONE',  ( 21.77812500061451928, -4.541064518000419881, 2.621784821874995952 ) ) ;
#21670 = CARTESIAN_POINT ( 'NONE',  ( 7.659375000614518036, 4.541064518000418104, -2.621784821874998173 ) ) ;
#21671 = CARTESIAN_POINT ( 'NONE',  ( 11.10000000122903252, 5.773502691896255534, 3.535250795749688894E-16 ) ) ;
#21672 = CARTESIAN_POINT ( 'NONE',  ( 17.88750000122903216, 4.330127018922191873, 2.499999999999999556 ) ) ;
#21673 =( BOUNDED_CURVE ( )  B_SPLINE_CURVE ( 2, ( #11064, #10702, #33235, #65758, #32144, #44339, #38790 ),
 .UNSPECIFIED., .F., .F. ) 
 B_SPLINE_CURVE_WITH_KNOTS ( ( 3, 2, 2, 3 ),
 ( 0.3750000000000000000, 0.3777777777777777679, 0.3805555555555554803, 0.3833333333333333037 ),
 .UNSPECIFIED. ) 
 CURVE ( )  GEOMETRIC_REPRESENTATION_ITEM ( )  RATIONAL_B_SPLINE_CURVE ( ( 1.000000000000000000, 0.8660254037844387076, 1.000000000000000000, 0.8660254037844387076, 1.000000000000000000, 0.8660254037844413721, 0.9999999999999973355 ) ) 
 REPRESENTATION_ITEM ( '' )  );
#21674 = CARTESIAN_POINT ( 'NONE',  ( 14.54062500061451679, -3.027376345333614438, 5.243569643749998122 ) ) ;
#21675 = CARTESIAN_POINT ( 'NONE',  ( 19.34062500061451573, 6.054752690667223547, 3.707466751127219781E-16 ) ) ;
#21676 = CARTESIAN_POINT ( 'NONE',  ( 24.86250000122903359, -4.330127018922190985, -2.500000000000001332 ) ) ;
#21677 =( BOUNDED_CURVE ( )  B_SPLINE_CURVE ( 3, ( #37196, #60083, #14294, #3225 ),
 .UNSPECIFIED., .F., .F. ) 
 B_SPLINE_CURVE_WITH_KNOTS ( ( 4, 4 ),
 ( 3.141592653589793116, 4.712388980384689674 ),
 .UNSPECIFIED. ) 
 CURVE ( )  GEOMETRIC_REPRESENTATION_ITEM ( )  RATIONAL_B_SPLINE_CURVE ( ( 1.000000000000000000, 0.8047378541243649375, 0.8047378541243649375, 1.000000000000000000 ) ) 
 REPRESENTATION_ITEM ( '' )  );
#21678 = CARTESIAN_POINT ( 'NONE',  ( 27.75000000122903288, 5.773502691896255534, 3.535250795749688894E-16 ) ) ;
#21679 = CARTESIAN_POINT ( 'NONE',  ( 22.91249999999999432, -5.773502691896255534, -1.060575238724906372E-15 ) ) ;
#21680 = CARTESIAN_POINT ( 'NONE',  ( -3.756430356249999214, 14.17812499938548498, 27.83122392262697531 ) ) ;
#21681 = CARTESIAN_POINT ( 'NONE',  ( 26.14687500061451431, 6.054752690667223547, 3.707466751127219781E-16 ) ) ;
#21682 = CARTESIAN_POINT ( 'NONE',  ( 4.898587196589412829E-16, 27.50000000000000000, 34.00000000000000000 ) ) ;
#21683 = EDGE_CURVE ( 'NONE', #38944, #3324, #24495, .T. ) ;
#21684 = CARTESIAN_POINT ( 'NONE',  ( 12.78750000122903430, 6.123233995736764310E-16, -4.999999999999998224 ) ) ;
#21685 = CARTESIAN_POINT ( 'NONE',  ( 29.10937500061451644, -4.541064518000417216, -2.621784821875001281 ) ) ;
#21686 = CARTESIAN_POINT ( 'NONE',  ( 4.898587196589412829E-16, 27.50000000000000000, 34.00000000000000000 ) ) ;
#21687 =( BOUNDED_CURVE ( )  B_SPLINE_CURVE ( 2, ( #57300, #11881, #50333, #17761, #6705, #56933, #46226, #18123, #6337 ),
 .UNSPECIFIED., .F., .F. ) 
 B_SPLINE_CURVE_WITH_KNOTS ( ( 3, 2, 2, 2, 3 ),
 ( 0.2638888888888888951, 0.2685185185185185452, 0.2777777777777777901, 0.2870370370370370350, 0.2916666666666666852 ),
 .UNSPECIFIED. ) 
 CURVE ( )  GEOMETRIC_REPRESENTATION_ITEM ( )  RATIONAL_B_SPLINE_CURVE ( ( 0.9330127018922194093, 0.9330127018922194093, 1.000000000000000000, 0.8660254037844387076, 1.000000000000000000, 0.8660254037844387076, 1.000000000000000000, 0.9330127018922189652, 0.9330127018922194093 ) ) 
 REPRESENTATION_ITEM ( '' )  );
#21688 = CARTESIAN_POINT ( 'NONE',  ( 4.696875000614518569, -3.027376345333614438, 5.243569643749998122 ) ) ;
#21689 = CARTESIAN_POINT ( 'NONE',  ( 26.87812500061451360, 6.421520780324663323E-16, -5.243569643749999010 ) ) ;
#21690 = CARTESIAN_POINT ( 'NONE',  ( -3.756430356250000102, 13.87812499938548250, 30.00000000000000000 ) ) ;
#21691 = CARTESIAN_POINT ( 'NONE',  ( 10.24687500061451750, -3.027376345333610441, -5.243569643749999898 ) ) ;
#21692 = LINE ( 'NONE', #43145, #9993 ) ;
#21693 = CARTESIAN_POINT ( 'NONE',  ( 2.859375000614519546, 0.000000000000000000, 5.243569643749999010 ) ) ;
#21694 = CARTESIAN_POINT ( 'NONE',  ( 9.796875000614519990, -3.027376345333610441, -5.243569643749999898 ) ) ;
#21695 = CARTESIAN_POINT ( 'NONE',  ( 27.98437500061451289, 4.541064518000418104, 2.621784821874999949 ) ) ;
#21696 = CARTESIAN_POINT ( 'NONE',  ( 4.243569643749999898, 13.27812500061459566, 30.00000000000000000 ) ) ;
#21697 = CARTESIAN_POINT ( 'NONE',  ( 19.46249999999999858, 2.886751345948129099, -4.999999999999998224 ) ) ;
#21698 = ORIENTED_EDGE ( 'NONE', *, *, #30772, .T. ) ;
#21699 = CARTESIAN_POINT ( 'NONE',  ( 28.83749999999999858, -2.886751345948125991, -5.000000000000000000 ) ) ;
#21700 = CARTESIAN_POINT ( 'NONE',  ( 4.987500000000002487, -2.886751345948125991, -5.000000000000000000 ) ) ;
#21701 = EDGE_LOOP ( 'NONE', ( #70688, #52589, #31389, #43018 ) ) ;
#21702 = CARTESIAN_POINT ( 'NONE',  ( 16.86562500061451786, -6.054752690667223547, -1.112240025338166033E-15 ) ) ;
#21703 = CARTESIAN_POINT ( 'NONE',  ( 8.578125000614518214, 4.541064518000418104, 2.621784821874999949 ) ) ;
#21704 = CARTESIAN_POINT ( 'NONE',  ( 22.09687500061451360, 0.000000000000000000, 4.756430356249998326 ) ) ;
#21705 = CARTESIAN_POINT ( 'NONE',  ( 6.159375000614517148, -4.541064518000417216, -2.621784821875001281 ) ) ;
#21706 = CARTESIAN_POINT ( 'NONE',  ( 18.75000000122903288, 5.773502691896255534, 3.535250795749688894E-16 ) ) ;
#21707 = CARTESIAN_POINT ( 'NONE',  ( 23.85000000122903430, -2.886751345948096681, 5.000000000000054179 ) ) ;
#21708 = CARTESIAN_POINT ( 'NONE',  ( 7.959375000614516971, -4.541064518000417216, -2.621784821875001281 ) ) ;
#21709 = CARTESIAN_POINT ( 'NONE',  ( 12.27187500061451786, 3.027376345333611329, 5.243569643749999010 ) ) ;
#21710 = CARTESIAN_POINT ( 'NONE',  ( 23.44687500061451502, 6.054752690667223547, 3.707466751127219781E-16 ) ) ;
#21711 = DIRECTION ( 'NONE',  ( -0.000000000000000000, -1.000000000000000000, -0.000000000000000000 ) ) ;
#21712 = EDGE_LOOP ( 'NONE', ( #5240, #12671, #27622, #61588 ) ) ;
#21713 = CARTESIAN_POINT ( 'NONE',  ( 10.53750000000000320, 5.773502691896255534, 3.535250795749688894E-16 ) ) ;
#21714 = CARTESIAN_POINT ( 'NONE',  ( 16.95937500061451786, -4.541064518000417216, -2.621784821875001281 ) ) ;
#21715 = CARTESIAN_POINT ( 'NONE',  ( 9.946875000614516793, 6.054752690667223547, 3.707466751127219781E-16 ) ) ;
#21716 = CARTESIAN_POINT ( 'NONE',  ( 3.756430356250000102, 15.34062499938548285, 30.00000000000000000 ) ) ;
#21717 = CARTESIAN_POINT ( 'NONE',  ( 20.88749999999999929, 5.773502691896255534, 3.535250795749688894E-16 ) ) ;
#21718 = CARTESIAN_POINT ( 'NONE',  ( -3.999999999999999556, 16.73750000000000071, 27.69059892324149175 ) ) ;
#21719 = CARTESIAN_POINT ( 'NONE',  ( -4.243569643749999898, 10.37187500061451750, -32.45002607614398471 ) ) ;
#21720 = CARTESIAN_POINT ( 'NONE',  ( 22.32187500061451502, -5.492252693125287522, -1.008910452111647106E-15 ) ) ;
#21721 = CARTESIAN_POINT ( 'NONE',  ( 13.15312500061451750, 0.000000000000000000, 5.243569643749999010 ) ) ;
#21722 = CARTESIAN_POINT ( 'NONE',  ( 28.84687500061452070, 6.054752690667223547, 3.707466751127219781E-16 ) ) ;
#21723 = CARTESIAN_POINT ( 'NONE',  ( 20.28749999999999787, -2.886751345948181946, -4.999999999999904077 ) ) ;
#21724 = CARTESIAN_POINT ( 'NONE',  ( 28.28437500061451715, 6.421520780324663323E-16, -5.243569643749999010 ) ) ;
#21725 = CARTESIAN_POINT ( 'NONE',  ( 9.375000000000001776, -4.330127018922194537, 2.499999999999995559 ) ) ;
#21726 = CARTESIAN_POINT ( 'NONE',  ( 4.000000000000000000, 16.25000000122903643, 32.30940107675849049 ) ) ;
#21727 = CARTESIAN_POINT ( 'NONE',  ( 10.08750000122903323, 6.123233995736764310E-16, -4.999999999999998224 ) ) ;
#21728 = CARTESIAN_POINT ( 'NONE',  ( 20.29687500061451644, 6.054752690667223547, 3.707466751127219781E-16 ) ) ;
#21729 = CARTESIAN_POINT ( 'NONE',  ( 14.67187500061451821, -6.054752690667223547, -1.112240025338166033E-15 ) ) ;
#21730 = ORIENTED_EDGE ( 'NONE', *, *, #32398, .F. ) ;
#21731 = AXIS2_PLACEMENT_3D ( 'NONE', #67581, #16947, #39500 ) ;
#21732 = CARTESIAN_POINT ( 'NONE',  ( 18.06562500061451715, 3.027376345333611329, 5.243569643749999010 ) ) ;
#21733 = CARTESIAN_POINT ( 'NONE',  ( 27.63750000122903216, 6.123233995736764310E-16, -4.999999999999998224 ) ) ;
#21734 = CARTESIAN_POINT ( 'NONE',  ( 15.72187500061451892, 3.027376345333613106, -5.243569643749998122 ) ) ;
#21735 = CARTESIAN_POINT ( 'NONE',  ( 3.035296952380283297, 9.529902216964481809, -24.82070563642345462 ) ) ;
#21736 = CARTESIAN_POINT ( 'NONE',  ( 17.65312500061451573, 0.000000000000000000, 5.243569643749999010 ) ) ;
#21737 = DIRECTION ( 'NONE',  ( -1.000000000000000000, 0.000000000000000000, 0.000000000000000000 ) ) ;
#21738 = CARTESIAN_POINT ( 'NONE',  ( 25.32187500061451857, 3.027376345333611329, 5.243569643749999010 ) ) ;
#21739 = CARTESIAN_POINT ( 'NONE',  ( -4.243569643749999898, 11.66562500061451679, 27.54997392385601529 ) ) ;
#21740 = CARTESIAN_POINT ( 'NONE',  ( 15.12187500061451750, -6.054752690667223547, -1.112240025338166033E-15 ) ) ;
#21741 = CARTESIAN_POINT ( 'NONE',  ( 13.50000000122903288, -2.886751345948129988, 4.999999999999997335 ) ) ;
#21742 = CARTESIAN_POINT ( 'NONE',  ( 9.571875000614518569, 2.746126346562643317, 4.756430356249998326 ) ) ;
#21743 = CARTESIAN_POINT ( 'NONE',  ( 3.310802318797580579, -3.746810377620464205, 3.668301323911666412 ) ) ;
#21744 = CARTESIAN_POINT ( 'NONE',  ( 20.55937500061451573, -4.541064518000417216, -2.621784821875001281 ) ) ;
#21745 = CARTESIAN_POINT ( 'NONE',  ( 23.28750000122903430, 4.330127018922191873, 2.499999999999999556 ) ) ;
#21746 = CARTESIAN_POINT ( 'NONE',  ( 17.78437500061451715, -4.541064518000419881, 2.621784821874995952 ) ) ;
#21747 = CARTESIAN_POINT ( 'NONE',  ( 12.59062500061451573, 6.054752690667223547, 3.707466751127219781E-16 ) ) ;
#21748 = CARTESIAN_POINT ( 'NONE',  ( -3.000416591977282496E-16, 13.44687500061451857, 25.09994784771203058 ) ) ;
#21749 = CARTESIAN_POINT ( 'NONE',  ( 17.39062500061451644, -3.027376345333610441, -5.243569643749999898 ) ) ;
#21750 = ORIENTED_EDGE ( 'NONE', *, *, #25488, .F. ) ;
#21751 = VERTEX_POINT ( 'NONE', #47398 ) ;
#21752 = CARTESIAN_POINT ( 'NONE',  ( 19.68750000000000355, -2.886751345948129988, 4.999999999999997335 ) ) ;
#21753 = CARTESIAN_POINT ( 'NONE',  ( 28.27500000122902435, 2.886751345948143754, 4.999999999999969802 ) ) ;
#21754 = CARTESIAN_POINT ( 'NONE',  ( 25.30312500061451431, 0.000000000000000000, 5.243569643749999010 ) ) ;
#21755 = CARTESIAN_POINT ( 'NONE',  ( 4.940625000614515372, 6.054752690667223547, 3.707466751127219781E-16 ) ) ;
#21756 = CARTESIAN_POINT ( 'NONE',  ( 17.10000000122903430, -2.886751345948129988, 4.999999999999997335 ) ) ;
#21757 = CARTESIAN_POINT ( 'NONE',  ( 23.54062500061451146, -3.027376345333614438, 5.243569643749998122 ) ) ;
#21758 = CARTESIAN_POINT ( 'NONE',  ( 22.87500000000000000, -4.330127018922194537, 2.499999999999995559 ) ) ;
#21759 = CARTESIAN_POINT ( 'NONE',  ( 26.35312500061451857, -4.541064518000417216, -2.621784821875001281 ) ) ;
#21760 = CARTESIAN_POINT ( 'NONE',  ( 6.515625000614516438, -6.054752690667223547, -1.112240025338166033E-15 ) ) ;
#21761 = ORIENTED_EDGE ( 'NONE', *, *, #64577, .F. ) ;
#21762 = CARTESIAN_POINT ( 'NONE',  ( -1.071796769724490339, 20.22634618820329777, 26.00000000000000000 ) ) ;
#21763 = DIRECTION ( 'NONE',  ( -0.000000000000000000, -1.000000000000000000, -0.000000000000000000 ) ) ;
#21764 = CARTESIAN_POINT ( 'NONE',  ( 11.14687500061451608, -2.746126346562642428, -4.756430356249999214 ) ) ;
#21765 = CARTESIAN_POINT ( 'NONE',  ( -1.071796769724504328, 11.20490381179670081, 33.99999999999999289 ) ) ;
#21766 = CARTESIAN_POINT ( 'NONE',  ( 1.999999999999998668, 13.66250000122903607, -33.46410161513775705 ) ) ;
#21767 = CARTESIAN_POINT ( 'NONE',  ( 9.001249775931846008E-16, 18.17187500061451999, -25.09994784771203058 ) ) ;
#21768 = CARTESIAN_POINT ( 'NONE',  ( 9.487500000000000711, -2.886751345948125991, -5.000000000000000000 ) ) ;
#21769 = CARTESIAN_POINT ( 'NONE',  ( 9.084375000614517859, 4.541064518000418104, 2.621784821874999949 ) ) ;
#21770 = CARTESIAN_POINT ( 'NONE',  ( 7.087500001229034119, 4.330127018922191873, 2.499999999999999556 ) ) ;
#21771 = CARTESIAN_POINT ( 'NONE',  ( 11.63437500061451857, 6.421520780324663323E-16, -5.243569643749999010 ) ) ;
#21772 = CARTESIAN_POINT ( 'NONE',  ( 6.196875000614515905, -3.027376345333610441, -5.243569643749999898 ) ) ;
#21773 = LINE ( 'NONE', #67234, #57415 ) ;
#21774 = VECTOR ( 'NONE', #15230, 1000.000000000000000 ) ;
#21775 = DIRECTION ( 'NONE',  ( -1.000000000000000000, -0.000000000000000000, -0.000000000000000000 ) ) ;
#21776 = CARTESIAN_POINT ( 'NONE',  ( 11.03437500061451715, -4.541064518000419881, 2.621784821874995952 ) ) ;
#21777 = DIRECTION ( 'NONE',  ( 0.000000000000000000, 0.000000000000000000, 1.000000000000000000 ) ) ;
#21778 = CARTESIAN_POINT ( 'NONE',  ( 19.45312500061451644, 0.000000000000000000, 5.243569643749999010 ) ) ;
#21779 = CARTESIAN_POINT ( 'NONE',  ( -5.810221930991193690E-16, 12.35000000122903430, -34.00000000000000000 ) ) ;
#21780 = CARTESIAN_POINT ( 'NONE',  ( 45.00000000000000000, 0.000000000000000000, 4.999999999999998224 ) ) ;
#21781 = CARTESIAN_POINT ( 'NONE',  ( 23.29687500061451644, -3.027376345333610441, -5.243569643749999898 ) ) ;
#21782 = CARTESIAN_POINT ( 'NONE',  ( 4.000000000000000000, 19.28749999999999787, 32.30940107675849760 ) ) ;
#21783 = CARTESIAN_POINT ( 'NONE',  ( 3.103125000614517237, 4.541064518000418104, -2.621784821874998173 ) ) ;
#21784 = ADVANCED_FACE ( 'NONE', ( #19300 ), #64381, .T. ) ;
#21785 = CARTESIAN_POINT ( 'NONE',  ( 20.78437500061451360, -2.746126346562646425, 4.756430356249996549 ) ) ;
#21786 = CARTESIAN_POINT ( 'NONE',  ( 26.05312500061451431, 4.541064518000418104, -2.621784821874998173 ) ) ;
#21787 = CARTESIAN_POINT ( 'NONE',  ( 15.77812500061451573, 4.541064518000418104, 2.621784821874999949 ) ) ;
#21788 = CARTESIAN_POINT ( 'NONE',  ( 14.49375000122903145, -2.886751345948125991, -5.000000000000000000 ) ) ;
#21789 = CARTESIAN_POINT ( 'NONE',  ( 14.70937500061451786, -4.541064518000417216, -2.621784821875001281 ) ) ;
#21790 = CARTESIAN_POINT ( 'NONE',  ( 7.237500001229035362, -4.330127018922194537, 2.499999999999995559 ) ) ;
#21791 = CARTESIAN_POINT ( 'NONE',  ( 24.41250000122903430, -4.330127018922190985, -2.500000000000001332 ) ) ;
#21792 = CARTESIAN_POINT ( 'NONE',  ( 3.084375000614519191, 6.421520780324663323E-16, -5.243569643749999010 ) ) ;
#21793 = CARTESIAN_POINT ( 'NONE',  ( 13.95937500061451786, 4.541064518000418104, -2.621784821874998173 ) ) ;
#21794 = CARTESIAN_POINT ( 'NONE',  ( 5.810221930991193690E-16, 17.95624999877096784, 26.00000000000000000 ) ) ;
#21795 = CARTESIAN_POINT ( 'NONE',  ( 3.149999999999999911, -4.330127018922190985, -2.500000000000001332 ) ) ;
#21796 = CARTESIAN_POINT ( 'NONE',  ( 3.337500001229034563, 6.123233995736764310E-16, -4.999999999999998224 ) ) ;
#21797 = CARTESIAN_POINT ( 'NONE',  ( 24.79687500061451999, 6.054752690667223547, 3.707466751127219781E-16 ) ) ;
#21798 = CARTESIAN_POINT ( 'NONE',  ( 16.77187500061451786, 3.027376345333611329, 5.243569643749999010 ) ) ;
#21799 = CARTESIAN_POINT ( 'NONE',  ( 3.756430356250000102, 15.90312499938548108, 30.00000000000000000 ) ) ;
#21800 = ADVANCED_FACE ( 'NONE', ( #30769 ), #53300, .F. ) ;
#21801 = CARTESIAN_POINT ( 'NONE',  ( 27.41250000000000142, -5.773502691896255534, -1.060575238724906372E-15 ) ) ;
#21802 = CARTESIAN_POINT ( 'NONE',  ( 3.975000001229033852, 2.886751345948126879, 4.999999999999999112 ) ) ;
#21803 = CARTESIAN_POINT ( 'NONE',  ( 6.787500000000001421, -2.886751345948125991, -5.000000000000000000 ) ) ;
#21804 = CARTESIAN_POINT ( 'NONE',  ( 7.509375000614516793, 2.746126346562645981, -4.756430356249997438 ) ) ;
#21805 = CARTESIAN_POINT ( 'NONE',  ( 19.30312500061451786, 4.541064518000418104, -2.621784821874998173 ) ) ;
#21806 = CARTESIAN_POINT ( 'NONE',  ( 10.42500000000000071, 6.123233995736764310E-16, -4.999999999999998224 ) ) ;
#21807 = CARTESIAN_POINT ( 'NONE',  ( 4.715625000614516615, -6.054752690667223547, -1.112240025338166033E-15 ) ) ;
#21808 = CARTESIAN_POINT ( 'NONE',  ( 18.26249999999999929, 2.886751345948126879, 4.999999999999999112 ) ) ;
#21809 = EDGE_CURVE ( 'NONE', #43716, #33795, #38515, .T. ) ;
#21810 = CARTESIAN_POINT ( 'NONE',  ( -3.999999999999999112, 17.30000000000000071, 30.00000000000000000 ) ) ;
#21811 = CARTESIAN_POINT ( 'NONE',  ( 21.45000000122903216, 5.773502691896255534, 3.535250795749688894E-16 ) ) ;
#21812 = CARTESIAN_POINT ( 'NONE',  ( -0.6945831915928805111, 10.00052343484236772, -33.93923269050669944 ) ) ;
#21813 = CARTESIAN_POINT ( 'NONE',  ( 29.44687500061451857, -3.027376345333614438, 5.243569643749998122 ) ) ;
#21814 = ORIENTED_EDGE ( 'NONE', *, *, #54584, .F. ) ;
#21815 = CARTESIAN_POINT ( 'NONE',  ( 17.12812500061451715, 4.541064518000418104, 2.621784821874999949 ) ) ;
#21816 = CARTESIAN_POINT ( 'NONE',  ( 24.36562500061451786, 3.027376345333611329, 5.243569643749999010 ) ) ;
#21817 = CARTESIAN_POINT ( 'NONE',  ( 21.49687500061451573, -3.027376345333610441, -5.243569643749999898 ) ) ;
#21818 = CARTESIAN_POINT ( 'NONE',  ( 6.112499999999999822, 2.886751345948126879, 4.999999999999999112 ) ) ;
#21819 = CARTESIAN_POINT ( 'NONE',  ( 9.290625000614515017, -3.027376345333610441, -5.243569643749999898 ) ) ;
#21820 = CARTESIAN_POINT ( 'NONE',  ( 24.17812500061451786, 6.421520780324663323E-16, -5.243569643749999010 ) ) ;
#21821 = CARTESIAN_POINT ( 'NONE',  ( 15.75937500061451857, 4.541064518000418104, -2.621784821874998173 ) ) ;
#21822 = CARTESIAN_POINT ( 'NONE',  ( 20.03437500061451715, -4.541064518000419881, 2.621784821874995952 ) ) ;
#21823 = CARTESIAN_POINT ( 'NONE',  ( 17.45625000122903003, 0.000000000000000000, 4.999999999999998224 ) ) ;
#21824 = CARTESIAN_POINT ( 'NONE',  ( 4.243569643749999010, 19.61562500061451431, 27.54997392385601174 ) ) ;
#21825 = CARTESIAN_POINT ( 'NONE',  ( 22.42500000122903359, 2.886751345948126879, 4.999999999999999112 ) ) ;
#21826 = CARTESIAN_POINT ( 'NONE',  ( 16.47187500061452070, -5.492252693125287522, -1.008910452111647106E-15 ) ) ;
#21827 = CARTESIAN_POINT ( 'NONE',  ( 10.75312500061451715, 4.541064518000418104, -2.621784821874998173 ) ) ;
#21828 = CARTESIAN_POINT ( 'NONE',  ( 8.221875000614518925, 3.027376345333611329, 5.243569643749999010 ) ) ;
#21829 = CARTESIAN_POINT ( 'NONE',  ( 6.796875000614516438, 6.054752690667223547, 3.707466751127219781E-16 ) ) ;
#21830 = EDGE_CURVE ( 'NONE', #48891, #37048, #66986, .T. ) ;
#21831 = ORIENTED_EDGE ( 'NONE', *, *, #70383, .T. ) ;
#21832 = CARTESIAN_POINT ( 'NONE',  ( 27.49687500061451217, 6.054752690667223547, 3.707466751127219781E-16 ) ) ;
#21833 = CARTESIAN_POINT ( 'NONE',  ( 19.82812500061451644, 4.541064518000418104, 2.621784821874999949 ) ) ;
#21834 = CARTESIAN_POINT ( 'NONE',  ( 28.87500000122902932, -5.773502691896255534, -1.060575238724906372E-15 ) ) ;
#21835 = CARTESIAN_POINT ( 'NONE',  ( 27.59062500061451573, -3.027376345333614438, 5.243569643749998122 ) ) ;
#21836 = CARTESIAN_POINT ( 'NONE',  ( 24.53437500061451715, -4.541064518000419881, 2.621784821874995952 ) ) ;
#21837 = CARTESIAN_POINT ( 'NONE',  ( 18.66562500061451146, -6.054752690667223547, -1.112240025338166033E-15 ) ) ;
#21838 = CARTESIAN_POINT ( 'NONE',  ( -2.121784821874996840, 18.58437500061451786, 33.67503911421598417 ) ) ;
#21839 = AXIS2_PLACEMENT_3D ( 'NONE', #8017, #59334, #65253 ) ;
#21840 = CARTESIAN_POINT ( 'NONE',  ( 25.30312500061451431, 0.000000000000000000, 5.243569643749999010 ) ) ;
#21841 = CARTESIAN_POINT ( 'NONE',  ( 3.637500001229036162, -4.330127018922194537, 2.499999999999995559 ) ) ;
#21842 = ORIENTED_EDGE ( 'NONE', *, *, #35681, .T. ) ;
#21843 = CARTESIAN_POINT ( 'NONE',  ( 28.35000000000000142, -4.330127018922190985, -2.500000000000001332 ) ) ;
#21844 = CARTESIAN_POINT ( 'NONE',  ( -3.999999999999999112, 15.50000000000000000, -30.00000000000000000 ) ) ;
#21845 = CARTESIAN_POINT ( 'NONE',  ( 1.878215178125000495, 17.32812499938548356, 26.74683588394047007 ) ) ;
#21846 = CARTESIAN_POINT ( 'NONE',  ( 5.596875000614516260, -3.027376345333614438, 5.243569643749998122 ) ) ;
#21847 = CARTESIAN_POINT ( 'NONE',  ( 13.64062500061451644, -3.027376345333614438, 5.243569643749998122 ) ) ;
#21848 = CARTESIAN_POINT ( 'NONE',  ( 5.371875000614516615, 3.027376345333613106, -5.243569643749998122 ) ) ;
#21849 = CARTESIAN_POINT ( 'NONE',  ( 25.50000000122903288, 5.773502691896255534, 3.535250795749688894E-16 ) ) ;
#21850 = CARTESIAN_POINT ( 'NONE',  ( 14.74687500061451750, -3.027376345333610441, -5.243569643749999898 ) ) ;
#21851 = CARTESIAN_POINT ( 'NONE',  ( 29.39062500061451289, -3.027376345333614438, 5.243569643749998122 ) ) ;
#21852 = CARTESIAN_POINT ( 'NONE',  ( -1.071796769724488563, 11.09240381056766545, 34.00000000000000000 ) ) ;
#21853 = CARTESIAN_POINT ( 'NONE',  ( 27.83437500061451786, 6.421520780324663323E-16, -5.243569643749999010 ) ) ;
#21854 = CARTESIAN_POINT ( 'NONE',  ( 30.00000000000000000, 0.000000000000000000, 0.000000000000000000 ) ) ;
#21855 = CARTESIAN_POINT ( 'NONE',  ( 13.34062500061451750, -3.027376345333610441, -5.243569643749999898 ) ) ;
#21856 = ORIENTED_EDGE ( 'NONE', *, *, #70520, .F. ) ;
#21857 = AXIS2_PLACEMENT_3D ( 'NONE', #28003, #39446, #61967 ) ;
#21858 = CARTESIAN_POINT ( 'NONE',  ( 10.75312500061451715, 4.541064518000418104, -2.621784821874998173 ) ) ;
#21859 = VECTOR ( 'NONE', #40734, 1000.000000000000000 ) ;
#21860 = CARTESIAN_POINT ( 'NONE',  ( 9.328125000614518214, 6.421520780324663323E-16, -5.243569643749999010 ) ) ;
#21861 = CARTESIAN_POINT ( 'NONE',  ( 19.92187500061451644, 2.746126346562643317, 4.756430356249998326 ) ) ;
#21862 = CARTESIAN_POINT ( 'NONE',  ( 8.025000000000000355, -4.330127018922194537, 2.499999999999995559 ) ) ;
#21863 = CARTESIAN_POINT ( 'NONE',  ( 2.662500001229036073, 0.000000000000000000, 4.999999999999998224 ) ) ;
#21864 = CARTESIAN_POINT ( 'NONE',  ( 17.32499999999999929, 4.330127018922191873, 2.499999999999999556 ) ) ;
#21865 = CARTESIAN_POINT ( 'NONE',  ( 18.87187500061451573, 3.027376345333613106, -5.243569643749998122 ) ) ;
#21866 = CARTESIAN_POINT ( 'NONE',  ( 13.50000000122903288, -2.886751345948129988, 4.999999999999997335 ) ) ;
#21867 = CARTESIAN_POINT ( 'NONE',  ( 19.72499999999999787, -4.330127018922194537, 2.499999999999995559 ) ) ;
#21868 = CARTESIAN_POINT ( 'NONE',  ( 4.243569643749999010, 16.91562500061451502, -32.45002607614398471 ) ) ;
#21869 = CARTESIAN_POINT ( 'NONE',  ( -1.071796769724490783, 13.66115380933863399, 34.00000000000000711 ) ) ;
#21870 = CARTESIAN_POINT ( 'NONE',  ( 24.68437500061451573, 5.492252693125287522, 3.363034840372157021E-16 ) ) ;
#21871 = CARTESIAN_POINT ( 'NONE',  ( 14.34375000122903465, -2.886751345948074920, 5.000000000000092371 ) ) ;
#21872 = CARTESIAN_POINT ( 'NONE',  ( 25.82812500061451644, -4.541064518000419881, 2.621784821874995952 ) ) ;
#21873 = SURFACE_STYLE_USAGE ( .BOTH. , #10072 ) ;
#21874 = CARTESIAN_POINT ( 'NONE',  ( 4.898587196589412829E-16, 27.50000000000000000, 34.00000000000000000 ) ) ;
#21875 = CARTESIAN_POINT ( 'NONE',  ( 26.96249999999999858, -5.773502691896255534, -1.060575238724906372E-15 ) ) ;
#21876 = CARTESIAN_POINT ( 'NONE',  ( 10.41562500061451679, 3.027376345333611329, 5.243569643749999010 ) ) ;
#21877 = CARTESIAN_POINT ( 'NONE',  ( 26.85937500061451644, 2.746126346562645981, -4.756430356249997438 ) ) ;
#21878 = CARTESIAN_POINT ( 'NONE',  ( 21.19687500061451502, 6.054752690667223547, 3.707466751127219781E-16 ) ) ;
#21879 = CARTESIAN_POINT ( 'NONE',  ( 14.78437500061451537, 5.492252693125287522, 3.363034840372157021E-16 ) ) ;
#21880 = AXIS2_PLACEMENT_3D ( 'NONE', #65263, #20927, #20188 ) ;
#21881 = CARTESIAN_POINT ( 'NONE',  ( 7.153125000614518392, 4.541064518000418104, -2.621784821874998173 ) ) ;
#21882 = CARTESIAN_POINT ( 'NONE',  ( 10.92187500061451644, 3.027376345333611329, 5.243569643749999010 ) ) ;
#21883 = VERTEX_POINT ( 'NONE', #55141 ) ;
#21884 = CARTESIAN_POINT ( 'NONE',  ( 20.93437500061451573, -4.541064518000419881, 2.621784821874995952 ) ) ;
#21885 = CARTESIAN_POINT ( 'NONE',  ( 4.907911205059083602E-16, 5.000000000000000000, -26.00000000000000000 ) ) ;
#21886 = ADVANCED_FACE ( 'NONE', ( #71770 ), #4174, .F. ) ;
#21887 = ADVANCED_FACE ( 'NONE', ( #61036, #26704 ), #55868, .F. ) ;
#21888 = CARTESIAN_POINT ( 'NONE',  ( 28.72500000000000142, -4.330127018922194537, 2.499999999999995559 ) ) ;
#21889 = VECTOR ( 'NONE', #3382, 1000.000000000000000 ) ;
#21890 = CARTESIAN_POINT ( 'NONE',  ( 5.250000000000000888, 0.000000000000000000, 4.999999999999998224 ) ) ;
#21891 = CARTESIAN_POINT ( 'NONE',  ( 14.13750000122903394, 6.123233995736764310E-16, -4.999999999999998224 ) ) ;
#21892 = DIRECTION ( 'NONE',  ( -1.000000000000000000, -0.000000000000000000, -0.000000000000000000 ) ) ;
#21893 = CARTESIAN_POINT ( 'NONE',  ( 14.36250000122903359, 0.000000000000000000, 4.999999999999998224 ) ) ;
#21894 = ORIENTED_EDGE ( 'NONE', *, *, #7572, .T. ) ;
#21895 = CARTESIAN_POINT ( 'NONE',  ( 12.75000000000000178, 4.330127018922192761, -2.499999999999997780 ) ) ;
#21896 = CARTESIAN_POINT ( 'NONE',  ( 16.80000000000000071, 4.330127018922192761, -2.499999999999997780 ) ) ;
#21897 = CARTESIAN_POINT ( 'NONE',  ( 13.42500000122903536, 2.886751345948126879, 4.999999999999999112 ) ) ;
#21898 = CARTESIAN_POINT ( 'NONE',  ( 11.76562500061451644, 3.027376345333611329, 5.243569643749999010 ) ) ;
#21899 =( BOUNDED_CURVE ( )  B_SPLINE_CURVE ( 2, ( #37124, #30856, #3160, #47858, #42678, #70387, #37862 ),
 .UNSPECIFIED., .F., .F. ) 
 B_SPLINE_CURVE_WITH_KNOTS ( ( 3, 2, 2, 3 ),
 ( 0.1083333333333333648, 0.1111111111111111327, 0.1138888888888889006, 0.1166666666666666824 ),
 .UNSPECIFIED. ) 
 CURVE ( )  GEOMETRIC_REPRESENTATION_ITEM ( )  RATIONAL_B_SPLINE_CURVE ( ( 0.9999999999999986677, 0.8660254037844400399, 1.000000000000000000, 0.8660254037844387076, 1.000000000000000000, 0.8660254037844380415, 1.000000000000000666 ) ) 
 REPRESENTATION_ITEM ( '' )  );
#21900 = ORIENTED_EDGE ( 'NONE', *, *, #41575, .F. ) ;
#21901 = CARTESIAN_POINT ( 'NONE',  ( 9.112500000000000711, 2.886751345948129099, -4.999999999999998224 ) ) ;
#21902 = CARTESIAN_POINT ( 'NONE',  ( 18.56250000122903288, -4.330127018922190985, -2.500000000000001332 ) ) ;
#21903 = CARTESIAN_POINT ( 'NONE',  ( 2.121784821874999061, 13.85937500061451821, -33.67503911421598417 ) ) ;
#21904 = CARTESIAN_POINT ( 'NONE',  ( 28.61250000122903359, 4.330127018922192761, -2.499999999999997780 ) ) ;
#21905 = CARTESIAN_POINT ( 'NONE',  ( 3.756430356249998770, 14.40312499938548463, 32.16877607737301759 ) ) ;
#21906 = CARTESIAN_POINT ( 'NONE',  ( 10.76250000000000107, -5.773502691896255534, -1.060575238724906372E-15 ) ) ;
#21907 = DIRECTION ( 'NONE',  ( -1.000000000000000000, -0.000000000000000000, -0.000000000000000000 ) ) ;
#21908 = ORIENTED_EDGE ( 'NONE', *, *, #20969, .T. ) ;
#21909 = CARTESIAN_POINT ( 'NONE',  ( 24.44062500061451715, -3.027376345333614438, 5.243569643749998122 ) ) ;
#21910 = CARTESIAN_POINT ( 'NONE',  ( 4.000000000000000000, 13.43750000000000000, -27.69059892324149885 ) ) ;
#21911 = VECTOR ( 'NONE', #34078, 1000.000000000000000 ) ;
#21912 = CARTESIAN_POINT ( 'NONE',  ( 29.40937500061451715, 0.000000000000000000, 5.243569643749999010 ) ) ;
#21913 = CARTESIAN_POINT ( 'NONE',  ( 20.52187500061451786, -6.054752690667223547, -1.112240025338166033E-15 ) ) ;
#21914 = CARTESIAN_POINT ( 'NONE',  ( 17.57812500061451644, 4.541064518000418104, 2.621784821874999949 ) ) ;
#21915 = CARTESIAN_POINT ( 'NONE',  ( -4.243569643749999898, 11.21562500061459389, -32.45002607614398471 ) ) ;
#21916 = CARTESIAN_POINT ( 'NONE',  ( 6.215625000614517504, 3.027376345333613106, -5.243569643749998122 ) ) ;
#21917 = CARTESIAN_POINT ( 'NONE',  ( 29.43750000122903288, 6.123233995736764310E-16, -4.999999999999998224 ) ) ;
#21918 = CARTESIAN_POINT ( 'NONE',  ( 23.97187500061451715, 2.746126346562643317, 4.756430356249998326 ) ) ;
#21919 = CARTESIAN_POINT ( 'NONE',  ( 20.05312500061451431, -4.541064518000417216, -2.621784821875001281 ) ) ;
#21920 = CARTESIAN_POINT ( 'NONE',  ( 7.434375000614519280, -4.119189519843968306, 2.378215178124996054 ) ) ;
#21921 = CARTESIAN_POINT ( 'NONE',  ( 2.655984681222220721E-16, 19.05312499938548143, 25.66244784525396483 ) ) ;
#21922 = CARTESIAN_POINT ( 'NONE',  ( 16.32187500061451502, 3.027376345333611329, 5.243569643749999010 ) ) ;
#21923 = CARTESIAN_POINT ( 'NONE',  ( 13.58437500061451786, 4.541064518000418104, 2.621784821874999949 ) ) ;
#21924 = CARTESIAN_POINT ( 'NONE',  ( 22.02187500061452141, 3.027376345333613106, -5.243569643749998122 ) ) ;
#21925 = ORIENTED_EDGE ( 'NONE', *, *, #48397, .T. ) ;
#21926 = CARTESIAN_POINT ( 'NONE',  ( -3.000416591977282496E-16, 12.09687500061451892, 25.09994784771203058 ) ) ;
#21927 = CARTESIAN_POINT ( 'NONE',  ( 2.915625000614516793, -6.054752690667223547, -1.112240025338166033E-15 ) ) ;
#21928 = CARTESIAN_POINT ( 'NONE',  ( 26.39062500061451644, -3.027376345333610441, -5.243569643749999898 ) ) ;
#21929 = CARTESIAN_POINT ( 'NONE',  ( 27.77812500061451573, 6.421520780324663323E-16, -5.243569643749999010 ) ) ;
#21930 = CARTESIAN_POINT ( 'NONE',  ( 1.999999999999998668, 19.51250000122903216, -33.46410161513775705 ) ) ;
#21931 = CARTESIAN_POINT ( 'NONE',  ( 1.999999999999998668, 16.25000000000000000, 26.53589838486224650 ) ) ;
#21932 = CARTESIAN_POINT ( 'NONE',  ( 4.546875000614517326, 6.054752690667223547, 3.707466751127219781E-16 ) ) ;
#21933 = CARTESIAN_POINT ( 'NONE',  ( 11.73750000122903181, -4.330127018922194537, 2.499999999999995559 ) ) ;
#21934 = CARTESIAN_POINT ( 'NONE',  ( 9.337500001229033231, 4.330127018922191873, 2.499999999999999556 ) ) ;
#21935 = CARTESIAN_POINT ( 'NONE',  ( 3.440625000614518036, -3.027376345333610441, -5.243569643749999898 ) ) ;
#21936 = CARTESIAN_POINT ( 'NONE',  ( -3.999999999999999556, 17.58124999877096784, 27.69059892324149175 ) ) ;
#21937 = CARTESIAN_POINT ( 'NONE',  ( 19.06875000122903430, 2.886751345948129099, -4.999999999999998224 ) ) ;
#21938 = CARTESIAN_POINT ( 'NONE',  ( 11.67187500061451821, 3.027376345333613106, -5.243569643749998122 ) ) ;
#21939 = PRODUCT_RELATED_PRODUCT_CATEGORY ( 'part', '', ( #65012 ) ) ;
#21940 = CYLINDRICAL_SURFACE ( 'NONE', #72678, 4.000000000000000000 ) ;
#21941 = ORIENTED_EDGE ( 'NONE', *, *, #63349, .T. ) ;
#21942 = CARTESIAN_POINT ( 'NONE',  ( 20.61562500061451431, 3.027376345333613106, -5.243569643749998122 ) ) ;
#21943 = CARTESIAN_POINT ( 'NONE',  ( 12.75937500061451857, 0.000000000000000000, 5.243569643749999010 ) ) ;
#21944 = CARTESIAN_POINT ( 'NONE',  ( 5.315625000614516260, 3.027376345333613106, -5.243569643749998122 ) ) ;
#21945 = CARTESIAN_POINT ( 'NONE',  ( 21.27187500061451786, 3.027376345333611329, 5.243569643749999010 ) ) ;
#21946 = CARTESIAN_POINT ( 'NONE',  ( 6.215625000614517504, 3.027376345333613106, -5.243569643749998122 ) ) ;
#21947 = CARTESIAN_POINT ( 'NONE',  ( 6.600000001229032520, 5.773502691896255534, 3.535250795749688894E-16 ) ) ;
#21948 = CARTESIAN_POINT ( 'NONE',  ( 19.41562500061451146, 3.027376345333611329, 5.243569643749999010 ) ) ;
#21949 = CARTESIAN_POINT ( 'NONE',  ( 7.650000001229034119, -2.886751345948129988, 4.999999999999997335 ) ) ;
#21950 = CARTESIAN_POINT ( 'NONE',  ( 17.69062500061451715, -3.027376345333614438, 5.243569643749998122 ) ) ;
#21951 = CARTESIAN_POINT ( 'NONE',  ( 16.60312500061451857, 4.541064518000418104, -2.621784821874998173 ) ) ;
#21952 = CARTESIAN_POINT ( 'NONE',  ( 26.33437500061451431, -4.119189519843968306, 2.378215178124996054 ) ) ;
#21953 = CARTESIAN_POINT ( 'NONE',  ( 15.82499999999999929, 6.123233995736764310E-16, -4.999999999999998224 ) ) ;
#21954 = CARTESIAN_POINT ( 'NONE',  ( 10.68750000122903288, 4.330127018922191873, 2.499999999999999556 ) ) ;
#21955 = CARTESIAN_POINT ( 'NONE',  ( 7.378125000614518036, -4.541064518000419881, 2.621784821874995952 ) ) ;
#21956 = CARTESIAN_POINT ( 'NONE',  ( 11.72812500061451857, 4.541064518000418104, 2.621784821874999949 ) ) ;
#21957 = EDGE_CURVE ( 'NONE', #59877, #38481, #68729, .T. ) ;
#21958 = CARTESIAN_POINT ( 'NONE',  ( 21.22500000122903074, -5.773502691896255534, -1.060575238724906372E-15 ) ) ;
#21959 = CARTESIAN_POINT ( 'NONE',  ( 27.82499999999999929, -4.330127018922194537, 2.499999999999995559 ) ) ;
#21960 = CARTESIAN_POINT ( 'NONE',  ( -3.000416591977282496E-16, 12.54687500061451999, -34.90005215228797653 ) ) ;
#21961 = CARTESIAN_POINT ( 'NONE',  ( -1.071796769724490339, 14.37634618820330168, 26.00000000000000000 ) ) ;
#21962 = CARTESIAN_POINT ( 'NONE',  ( 4.425000001229032698, 2.886751345948126879, 4.999999999999999112 ) ) ;
#21963 = CARTESIAN_POINT ( 'NONE',  ( 3.984375000614517326, 6.421520780324663323E-16, -5.243569643749999010 ) ) ;
#21964 = CARTESIAN_POINT ( 'NONE',  ( 19.69687500061451857, -3.027376345333610441, -5.243569643749999898 ) ) ;
#21965 = CARTESIAN_POINT ( 'NONE',  ( 5.137499999999999289, 5.773502691896255534, 3.535250795749688401E-16 ) ) ;
#21966 = CARTESIAN_POINT ( 'NONE',  ( 15.51562500061451644, -6.054752690667223547, -1.112240025338166033E-15 ) ) ;
#21967 = CARTESIAN_POINT ( 'NONE',  ( 11.75625000122903430, -4.330127018922190985, -2.500000000000001332 ) ) ;
#21968 = CARTESIAN_POINT ( 'NONE',  ( 1.626862140677534273E-15, 9.875000001229034652, 34.00000000000000000 ) ) ;
#21969 = CARTESIAN_POINT ( 'NONE',  ( 28.39687500061452141, 6.054752690667223547, 3.707466751127219781E-16 ) ) ;
#21970 = CARTESIAN_POINT ( 'NONE',  ( 19.69687500061451502, 4.119189519843966529, -2.378215178124998275 ) ) ;
#21971 = CARTESIAN_POINT ( 'NONE',  ( 14.91562500061451679, 3.027376345333611329, 5.243569643749999010 ) ) ;
#21972 = CARTESIAN_POINT ( 'NONE',  ( 11.85937500061451644, 0.000000000000000000, 5.243569643749999010 ) ) ;
#21973 = EDGE_LOOP ( 'NONE', ( #45718, #51877, #15257, #68837 ) ) ;
#21974 = DIRECTION ( 'NONE',  ( 1.000000000000000000, 0.000000000000000000, 0.000000000000000000 ) ) ;
#21975 = CARTESIAN_POINT ( 'NONE',  ( 21.55312500061451431, 4.541064518000418104, -2.621784821874998173 ) ) ;
#21976 = DIRECTION ( 'NONE',  ( -0.000000000000000000, -1.000000000000000000, -0.000000000000000000 ) ) ;
#21977 = EDGE_CURVE ( 'NONE', #48607, #2372, #10687, .T. ) ;
#21978 = CARTESIAN_POINT ( 'NONE',  ( -3.999999999999999112, 18.31250000122903288, 30.00000000000000000 ) ) ;
#21979 = CARTESIAN_POINT ( 'NONE',  ( 13.42499999999999893, -4.330127018922194537, 2.499999999999995559 ) ) ;
#21980 = CARTESIAN_POINT ( 'NONE',  ( 20.81250000122903643, -4.330127018922190985, -2.500000000000001332 ) ) ;
#21981 = CARTESIAN_POINT ( 'NONE',  ( 16.67812500061451786, 4.541064518000418104, 2.621784821874999949 ) ) ;
#21982 = CARTESIAN_POINT ( 'NONE',  ( 12.79687500061451466, -4.119189519843965641, -2.378215178125001383 ) ) ;
#21983 = ORIENTED_EDGE ( 'NONE', *, *, #15704, .T. ) ;
#21984 = CARTESIAN_POINT ( 'NONE',  ( 20.13749999999999929, -2.886751345948129988, 4.999999999999997335 ) ) ;
#21985 = CARTESIAN_POINT ( 'NONE',  ( 22.62187500061451573, 3.027376345333611329, 5.243569643749999010 ) ) ;
#21986 = CARTESIAN_POINT ( 'NONE',  ( 26.87812500061451360, 6.421520780324663323E-16, -5.243569643749999010 ) ) ;
#21987 = ORIENTED_EDGE ( 'NONE', *, *, #39247, .T. ) ;
#21988 = CARTESIAN_POINT ( 'NONE',  ( 21.05625000122903145, 0.000000000000000000, 4.999999999999998224 ) ) ;
#21989 = CARTESIAN_POINT ( 'NONE',  ( 10.75312500061451715, 4.541064518000418104, -2.621784821874998173 ) ) ;
#21990 = CARTESIAN_POINT ( 'NONE',  ( 6.337500000000000355, -2.886751345948126435, -5.000000000000000000 ) ) ;
#21991 = AXIS2_PLACEMENT_3D ( 'NONE', #42125, #32137, #71293 ) ;
#21992 = CARTESIAN_POINT ( 'NONE',  ( 17.69999999999999929, 4.330127018922192761, -2.499999999999997780 ) ) ;
#21993 = CARTESIAN_POINT ( 'NONE',  ( 24.26249999999999929, -5.773502691896255534, -1.060575238724906372E-15 ) ) ;
#21994 = DIRECTION ( 'NONE',  ( -1.000000000000000000, -0.000000000000000000, -0.000000000000000000 ) ) ;
#21995 = CARTESIAN_POINT ( 'NONE',  ( 5.071875000614519458, 3.027376345333611329, 5.243569643749999010 ) ) ;
#21996 = CARTESIAN_POINT ( 'NONE',  ( 27.60937500061451644, 0.000000000000000000, 5.243569643749999010 ) ) ;
#21997 = ORIENTED_EDGE ( 'NONE', *, *, #5228, .T. ) ;
#21998 = CARTESIAN_POINT ( 'NONE',  ( 24.36562500061451786, 3.027376345333611329, 5.243569643749999010 ) ) ;
#21999 = MANIFOLD_SOLID_BREP ( 'CirPattern1', #47738 ) ;
#22000 = CARTESIAN_POINT ( 'NONE',  ( 24.42187500061451999, 3.027376345333611329, 5.243569643749999010 ) ) ;
#22002 = EDGE_CURVE ( 'NONE', #23329, #60892, #66963, .T. ) ;
#22001 = CARTESIAN_POINT ( 'NONE',  ( -2.121784821874999949, 19.27812500061459033, -33.67503911421598417 ) ) ;
#22003 = CARTESIAN_POINT ( 'NONE',  ( 14.02499999999999858, 6.123233995736764310E-16, -4.999999999999998224 ) ) ;
#22004 = CARTESIAN_POINT ( 'NONE',  ( 7.903125000614515727, -4.541064518000417216, -2.621784821875001281 ) ) ;
#22005 = CARTESIAN_POINT ( 'NONE',  ( 5.924999999999999822, 6.123233995736764310E-16, -4.999999999999998224 ) ) ;
#22006 = CARTESIAN_POINT ( 'NONE',  ( 19.46249999999999503, 2.886751345948062486, -5.000000000000113687 ) ) ;
#22007 = CARTESIAN_POINT ( 'NONE',  ( 25.49062500061451431, -3.027376345333610441, -5.243569643749999898 ) ) ;
#22008 = CARTESIAN_POINT ( 'NONE',  ( 16.61250000122903359, 0.000000000000000000, 4.999999999999998224 ) ) ;
#22009 = CARTESIAN_POINT ( 'NONE',  ( 29.33437500061451431, -2.746126346562646425, 4.756430356249996549 ) ) ;
#22010 = CARTESIAN_POINT ( 'NONE',  ( 16.09687500061452070, -2.746126346562642428, -4.756430356249999214 ) ) ;
#22011 = CARTESIAN_POINT ( 'NONE',  ( 3.553125000614516082, 4.541064518000418104, -2.621784821874998173 ) ) ;
#22012 = CARTESIAN_POINT ( 'NONE',  ( 18.68437500061451928, -4.541064518000419881, 2.621784821874995952 ) ) ;
#22013 = CARTESIAN_POINT ( 'NONE',  ( -4.243569643749999898, 14.42187500061451644, 27.54997392385601529 ) ) ;
#22014 = CARTESIAN_POINT ( 'NONE',  ( 21.12187500061451573, 3.027376345333613106, -5.243569643749998122 ) ) ;
#22015 = CARTESIAN_POINT ( 'NONE',  ( 3.900000000000000799, 0.000000000000000000, 4.999999999999998224 ) ) ;
#22016 = CARTESIAN_POINT ( 'NONE',  ( 4.243569643749999898, 18.69687500061451857, 32.45002607614398471 ) ) ;
#22017 = CARTESIAN_POINT ( 'NONE',  ( 10.94062500061451537, -3.027376345333614438, 5.243569643749998122 ) ) ;
#22018 = CARTESIAN_POINT ( 'NONE',  ( 9.528763966825557376E-15, 17.07500000122903572, 34.00000000000000000 ) ) ;
#22019 = CARTESIAN_POINT ( 'NONE',  ( 6.834375000614518747, 4.541064518000418104, 2.621784821874999949 ) ) ;
#22020 = CARTESIAN_POINT ( 'NONE',  ( 8.390625000614518214, -3.027376345333610441, -5.243569643749999898 ) ) ;
#22021 = CARTESIAN_POINT ( 'NONE',  ( 13.13437500061451857, 4.541064518000418104, 2.621784821874999949 ) ) ;
#22022 = CARTESIAN_POINT ( 'NONE',  ( 19.80000000122903359, -2.886751345948129988, 4.999999999999997335 ) ) ;
#22023 = CARTESIAN_POINT ( 'NONE',  ( 7.996875000614519280, -3.027376345333610441, -5.243569643749999898 ) ) ;
#22024 = CARTESIAN_POINT ( 'NONE',  ( 10.04062500061451502, -3.027376345333614438, 5.243569643749998122 ) ) ;
#22025 = CARTESIAN_POINT ( 'NONE',  ( 7.940625000614518036, -3.027376345333610441, -5.243569643749999898 ) ) ;
#22026 = CARTESIAN_POINT ( 'NONE',  ( 25.55625000122903501, 0.000000000000000000, 4.999999999999998224 ) ) ;
#22027 = CARTESIAN_POINT ( 'NONE',  ( 19.77187500061451786, 3.027376345333613106, -5.243569643749998122 ) ) ;
#22028 = CARTESIAN_POINT ( 'NONE',  ( 9.112500001229033586, -4.330127018922190985, -2.500000000000001332 ) ) ;
#22029 = CARTESIAN_POINT ( 'NONE',  ( 26.61562500061451786, 3.027376345333611329, 5.243569643749999010 ) ) ;
#22030 = CARTESIAN_POINT ( 'NONE',  ( 12.36562500061451608, -6.054752690667223547, -1.112240025338166033E-15 ) ) ;
#22031 = CARTESIAN_POINT ( 'NONE',  ( 2.873218894584086858, -4.343029460077421078, 2.964791603877473314 ) ) ;
#22032 = CARTESIAN_POINT ( 'NONE',  ( -4.243569643749999898, 13.10937500061451821, -30.00000000000000000 ) ) ;
#22033 = CARTESIAN_POINT ( 'NONE',  ( 12.97500000122903252, 2.886751345948126879, 4.999999999999999112 ) ) ;
#22034 = CARTESIAN_POINT ( 'NONE',  ( 4.243569643749999010, 14.66562500061451857, -32.45002607614398471 ) ) ;
#22035 = CARTESIAN_POINT ( 'NONE',  ( 14.43750000122903288, -4.330127018922194537, 2.499999999999995559 ) ) ;
#22036 = CARTESIAN_POINT ( 'NONE',  ( 9.365625000614519635, 3.027376345333613106, -5.243569643749998122 ) ) ;
#22037 = CARTESIAN_POINT ( 'NONE',  ( 12.52500000000000213, -4.330127018922194537, 2.499999999999995559 ) ) ;
#22038 = CARTESIAN_POINT ( 'NONE',  ( 10.38750000122903572, -4.330127018922194537, 2.499999999999995559 ) ) ;
#22039 = CARTESIAN_POINT ( 'NONE',  ( 22.56562500061451715, 3.027376345333611329, 5.243569643749999010 ) ) ;
#22040 = CARTESIAN_POINT ( 'NONE',  ( 7.696875000614516793, 6.054752690667223547, 3.707466751127219781E-16 ) ) ;
#22041 = CARTESIAN_POINT ( 'NONE',  ( 9.937500001229032875, -4.330127018922194537, 2.499999999999995559 ) ) ;
#22042 = CARTESIAN_POINT ( 'NONE',  ( 18.15000000122903501, -2.886751345948125991, -5.000000000000000000 ) ) ;
#22043 = CARTESIAN_POINT ( 'NONE',  ( 14.87812500061451537, 4.541064518000418104, 2.621784821874999949 ) ) ;
#22044 = CARTESIAN_POINT ( 'NONE',  ( 17.99062500061451786, 6.054752690667223547, 3.707466751127219781E-16 ) ) ;
#22045 = CARTESIAN_POINT ( 'NONE',  ( 26.10000000122903430, -2.886751345948129988, 4.999999999999997335 ) ) ;
#22046 = CARTESIAN_POINT ( 'NONE',  ( 27.03750000122903430, -4.330127018922194537, 2.499999999999995559 ) ) ;
#22047 = CARTESIAN_POINT ( 'NONE',  ( 23.06250000000000355, 2.886751345948129099, -4.999999999999998224 ) ) ;
#22048 = CARTESIAN_POINT ( 'NONE',  ( 3.756430356250000546, 14.02812499938548463, 27.83122392262697886 ) ) ;
#22049 = CIRCLE ( 'NONE', #44487, 9.000000000000000000 ) ;
#22050 = CARTESIAN_POINT ( 'NONE',  ( 25.80937500061451928, 0.000000000000000000, 5.243569643749999010 ) ) ;
#22051 = LINE ( 'NONE', #44611, #48898 ) ;
#22052 = CARTESIAN_POINT ( 'NONE',  ( 11.47500000122903252, 2.886751345948129099, -4.999999999999998224 ) ) ;
#22053 = CARTESIAN_POINT ( 'NONE',  ( 29.07187500061451502, -6.054752690667223547, -1.112240025338166033E-15 ) ) ;
#22054 =( BOUNDED_CURVE ( )  B_SPLINE_CURVE ( 2, ( #25077, #14727, #13996, #30995, #54270, #47620, #59055 ),
 .UNSPECIFIED., .F., .F. ) 
 B_SPLINE_CURVE_WITH_KNOTS ( ( 3, 2, 2, 3 ),
 ( 0.1900000000000000855, 0.1933333333333333848, 0.1966666666666667118, 0.2000000000000000389 ),
 .UNSPECIFIED. ) 
 CURVE ( )  GEOMETRIC_REPRESENTATION_ITEM ( )  RATIONAL_B_SPLINE_CURVE ( ( 0.9999999999999966693, 0.8660254037844420383, 1.000000000000000000, 0.8660254037844387076, 1.000000000000000000, 0.8660254037844375974, 1.000000000000001110 ) ) 
 REPRESENTATION_ITEM ( '' )  );
#22055 = EDGE_CURVE ( 'NONE', #64264, #47295, #66585, .T. ) ;
#22056 = CARTESIAN_POINT ( 'NONE',  ( -1.999999999999997113, 13.32499999999999929, 33.46410161513775705 ) ) ;
#22057 = CARTESIAN_POINT ( 'NONE',  ( 4.359375000614517326, -4.541064518000417216, -2.621784821875001281 ) ) ;
#22058 = CARTESIAN_POINT ( 'NONE',  ( 24.14062500061451289, -3.027376345333610441, -5.243569643749999898 ) ) ;
#22059 = CARTESIAN_POINT ( 'NONE',  ( -1.878215178124999163, 14.25312499938548250, 26.74683588394047007 ) ) ;
#22060 = CARTESIAN_POINT ( 'NONE',  ( 4.544497808834801589, -2.085075457992688897, -4.544497808831748920 ) ) ;
#22061 = CARTESIAN_POINT ( 'NONE',  ( 9.609375000614518214, 0.000000000000000000, 5.243569643749999010 ) ) ;
#22062 = CARTESIAN_POINT ( 'NONE',  ( 22.20000000122903216, -2.886751345948159742, -4.999999999999942268 ) ) ;
#22063 = CARTESIAN_POINT ( 'NONE',  ( 29.54062500061451502, -3.027376345333610441, -5.243569643749999898 ) ) ;
#22064 = CARTESIAN_POINT ( 'NONE',  ( 5.896875000614518747, 6.054752690667223547, 3.707466751127219781E-16 ) ) ;
#22065 = CARTESIAN_POINT ( 'NONE',  ( 29.59687500061451715, -3.027376345333610441, -5.243569643749999898 ) ) ;
#22066 = CARTESIAN_POINT ( 'NONE',  ( 28.93125000122903145, 6.123233995736764310E-16, -4.999999999999998224 ) ) ;
#22067 = CARTESIAN_POINT ( 'NONE',  ( 19.16250000000000142, 2.886751345948126879, 4.999999999999999112 ) ) ;
#22068 = VERTEX_POINT ( 'NONE', #71399 ) ;
#22069 = CARTESIAN_POINT ( 'NONE',  ( 27.22499999999999787, 4.330127018922191873, 2.499999999999999556 ) ) ;
#22070 = CARTESIAN_POINT ( 'NONE',  ( 29.37187500061451928, 3.027376345333611329, 5.243569643749999010 ) ) ;
#22071 = ORIENTED_EDGE ( 'NONE', *, *, #54732, .T. ) ;
#22072 = CARTESIAN_POINT ( 'NONE',  ( 18.17812500061451786, -4.541064518000419881, 2.621784821874995952 ) ) ;
#22073 = CARTESIAN_POINT ( 'NONE',  ( 7.978125000614517681, 6.421520780324663323E-16, -5.243569643749999010 ) ) ;
#22074 = CARTESIAN_POINT ( 'NONE',  ( 21.83437500061451786, -2.746126346562642428, -4.756430356249999214 ) ) ;
#22075 = CARTESIAN_POINT ( 'NONE',  ( 4.509375000614518569, 4.541064518000418104, -2.621784821874998173 ) ) ;
#22076 = CARTESIAN_POINT ( 'NONE',  ( 16.76250000122903216, -4.330127018922190985, -2.500000000000001332 ) ) ;
#22077 = CARTESIAN_POINT ( 'NONE',  ( 1.626862140677534273E-15, 13.81250000000000000, -26.00000000000000355 ) ) ;
#22078 = CARTESIAN_POINT ( 'NONE',  ( 7.921875000614517326, -6.054752690667223547, -1.112240025338166033E-15 ) ) ;
#22079 = CARTESIAN_POINT ( 'NONE',  ( 10.92187500061451644, 3.027376345333611329, 5.243569643749999010 ) ) ;
#22080 = CARTESIAN_POINT ( 'NONE',  ( 21.23437500061451644, 4.541064518000418104, 2.621784821874999949 ) ) ;
#22081 = CARTESIAN_POINT ( 'NONE',  ( -3.137519842735245283E-14, 14.71250000000000213, -26.00000000000000711 ) ) ;
#22082 = ORIENTED_EDGE ( 'NONE', *, *, #32388, .T. ) ;
#22083 = CARTESIAN_POINT ( 'NONE',  ( 11.32500000000000107, 6.123233995736764310E-16, -4.999999999999998224 ) ) ;
#22084 = CARTESIAN_POINT ( 'NONE',  ( 6.009375000614519458, 0.000000000000000000, 5.243569643749999010 ) ) ;
#22085 = AXIS2_PLACEMENT_3D ( 'NONE', #44298, #27661, #61271 ) ;
#22086 = CARTESIAN_POINT ( 'NONE',  ( -3.756430356250000102, 16.01562499938548356, 30.00000000000000000 ) ) ;
#22087 = CARTESIAN_POINT ( 'NONE',  ( 21.33749999999999858, 5.773502691896255534, 3.535250795749688894E-16 ) ) ;
#22088 = CARTESIAN_POINT ( 'NONE',  ( 18.47812500061451857, 4.541064518000418104, 2.621784821874999949 ) ) ;
#22089 = CARTESIAN_POINT ( 'NONE',  ( 4.000000000000000000, 16.55000000000000071, 30.00000000000000000 ) ) ;
#22090 = CARTESIAN_POINT ( 'NONE',  ( 2.121784821875001281, 10.10937500061451821, -26.32496088578401938 ) ) ;
#22091 = CARTESIAN_POINT ( 'NONE',  ( 22.95937500061451431, 4.119189519843966529, -2.378215178124998275 ) ) ;
#22092 = CARTESIAN_POINT ( 'NONE',  ( 13.04062500061451502, 6.054752690667223547, 3.707466751127219781E-16 ) ) ;
#22093 = CARTESIAN_POINT ( 'NONE',  ( 27.90937500061451715, 4.541064518000418104, -2.621784821874998173 ) ) ;
#22094 = CARTESIAN_POINT ( 'NONE',  ( 10.93125000122903501, 6.123233995736764310E-16, -4.999999999999998224 ) ) ;
#22095 = CARTESIAN_POINT ( 'NONE',  ( 29.59687500061451715, -3.027376345333610441, -5.243569643749999898 ) ) ;
#22096 = CARTESIAN_POINT ( 'NONE',  ( 9.637499999999999289, 5.773502691896255534, 3.535250795749688894E-16 ) ) ;
#22097 = CARTESIAN_POINT ( 'NONE',  ( 4.000000000000000000, 14.90000000122903323, 32.30940107675849049 ) ) ;
#22098 = CARTESIAN_POINT ( 'NONE',  ( 9.487500001229033586, -4.330127018922194537, 2.499999999999995559 ) ) ;
#22099 = CARTESIAN_POINT ( 'NONE',  ( 19.28437500061451360, 6.421520780324663323E-16, -5.243569643749999010 ) ) ;
#22100 = CARTESIAN_POINT ( 'NONE',  ( 13.17187500061451999, 3.027376345333611329, 5.243569643749999010 ) ) ;
#22101 = CARTESIAN_POINT ( 'NONE',  ( -1.487416814333745711E-14, 16.62500000122903288, 34.00000000000000000 ) ) ;
#22102 = ORIENTED_EDGE ( 'NONE', *, *, #21050, .T. ) ;
#22103 = CARTESIAN_POINT ( 'NONE',  ( 15.89062500061451289, -3.027376345333614438, 5.243569643749998122 ) ) ;
#22104 = CARTESIAN_POINT ( 'NONE',  ( 25.98750000122903003, 4.330127018922191873, 2.499999999999999556 ) ) ;
#22105 = CARTESIAN_POINT ( 'NONE',  ( 14.70937500061451786, -4.541064518000417216, -2.621784821875001281 ) ) ;
#22106 = CARTESIAN_POINT ( 'NONE',  ( 5.192387018522393483, 8.549830518147029323, -26.96928673404218202 ) ) ;
#22107 = CARTESIAN_POINT ( 'NONE',  ( 16.11562500061451786, 3.027376345333613106, -5.243569643749998122 ) ) ;
#22108 = CARTESIAN_POINT ( 'NONE',  ( 25.78125000122903288, 6.123233995736764310E-16, -4.999999999999998224 ) ) ;
#22109 = ADVANCED_FACE ( 'NONE', ( #32235 ), #45514, .F. ) ;
#22110 = CARTESIAN_POINT ( 'NONE',  ( 26.59687500061451360, 6.054752690667223547, 3.707466751127219781E-16 ) ) ;
#22111 = CARTESIAN_POINT ( 'NONE',  ( 2.910968003956619921, -4.065258101981855887, 3.311910103879776024 ) ) ;
#22112 = CARTESIAN_POINT ( 'NONE',  ( 14.97187500061451892, 3.027376345333611329, 5.243569643749999010 ) ) ;
#22113 = CARTESIAN_POINT ( 'NONE',  ( 13.61250000122903359, -4.330127018922190985, -2.500000000000001332 ) ) ;
#22114 = CARTESIAN_POINT ( 'NONE',  ( 7.584375000614516082, 5.824947211148865298E-16, -4.756430356249998326 ) ) ;
#22115 = EDGE_CURVE ( 'NONE', #4158, #13105, #36571, .T. ) ;
#22116 = CARTESIAN_POINT ( 'NONE',  ( 9.001249775931846008E-16, 18.62187500061451573, -25.09994784771203058 ) ) ;
#22117 = CARTESIAN_POINT ( 'NONE',  ( 21.38437500061451502, -4.541064518000419881, 2.621784821874995952 ) ) ;
#22118 = CARTESIAN_POINT ( 'NONE',  ( 19.57500000122903216, 2.886751345948129099, -4.999999999999998224 ) ) ;
#22119 =( BOUNDED_CURVE ( )  B_SPLINE_CURVE ( 2, ( #41982, #58949, #36435, #7995, #20519, #2818, #48991 ),
 .UNSPECIFIED., .F., .F. ) 
 B_SPLINE_CURVE_WITH_KNOTS ( ( 3, 2, 2, 3 ),
 ( 0.3583333333333333925, 0.3611111111111111605, 0.3638888888888888729, 0.3666666666666666408 ),
 .UNSPECIFIED. ) 
 CURVE ( )  GEOMETRIC_REPRESENTATION_ITEM ( )  RATIONAL_B_SPLINE_CURVE ( ( 0.9999999999999973355, 0.8660254037844413721, 1.000000000000000000, 0.8660254037844387076, 1.000000000000000000, 0.8660254037844387076, 1.000000000000000000 ) ) 
 REPRESENTATION_ITEM ( '' )  );
#22120 = CARTESIAN_POINT ( 'NONE',  ( 16.88437500061451502, -4.541064518000419881, 2.621784821874995952 ) ) ;
#22121 = CARTESIAN_POINT ( 'NONE',  ( -4.243569643749997233, 11.79687500061451999, 32.45002607614398471 ) ) ;
#22122 = CARTESIAN_POINT ( 'NONE',  ( 16.79062500061451857, -3.027376345333614438, 5.243569643749998122 ) ) ;
#22123 = ORIENTED_EDGE ( 'NONE', *, *, #43393, .F. ) ;
#22124 = ORIENTED_EDGE ( 'NONE', *, *, #10210, .F. ) ;
#22125 = CARTESIAN_POINT ( 'NONE',  ( 19.38749999999999929, -2.886751345948125991, -5.000000000000000000 ) ) ;
#22126 = DIRECTION ( 'NONE',  ( -1.000000000000000000, -0.000000000000000000, -0.000000000000000000 ) ) ;
#22127 = CARTESIAN_POINT ( 'NONE',  ( 24.10312500061451502, -4.541064518000417216, -2.621784821875001281 ) ) ;
#22128 = CARTESIAN_POINT ( 'NONE',  ( 6.590625000614518392, -3.027376345333610441, -5.243569643749999898 ) ) ;
#22129 = CARTESIAN_POINT ( 'NONE',  ( 16.23750000122903359, -4.330127018922194537, 2.499999999999995559 ) ) ;
#22130 = CARTESIAN_POINT ( 'NONE',  ( 23.61562500061451431, -6.054752690667223547, -1.112240025338166033E-15 ) ) ;
#22131 = CARTESIAN_POINT ( 'NONE',  ( 20.66250000000000142, -5.773502691896255534, -1.060575238724906372E-15 ) ) ;
#22132 = CARTESIAN_POINT ( 'NONE',  ( 25.04062500061451502, -3.027376345333610441, -5.243569643749999898 ) ) ;
#22133 = CARTESIAN_POINT ( 'NONE',  ( 5.353125000614515905, 4.541064518000418104, -2.621784821874998173 ) ) ;
#22134 = ORIENTED_EDGE ( 'NONE', *, *, #69513, .F. ) ;
#22135 = CARTESIAN_POINT ( 'NONE',  ( 7.347880794884118750E-16, 20.00000000000000000, 36.00000000000000000 ) ) ;
#22136 = CARTESIAN_POINT ( 'NONE',  ( -5.810221930991193690E-16, 14.60000000122903252, 26.00000000000000355 ) ) ;
#22137 = CARTESIAN_POINT ( 'NONE',  ( 11.82187500061451679, 2.746126346562643317, 4.756430356249998326 ) ) ;
#22138 = CARTESIAN_POINT ( 'NONE',  ( 1.626862140677534273E-15, 18.76250000000000284, 34.00000000000000000 ) ) ;
#22139 = CARTESIAN_POINT ( 'NONE',  ( 3.999999999999999112, 12.23750000122903359, -30.00000000000000000 ) ) ;
#22140 = CARTESIAN_POINT ( 'NONE',  ( 4.243569643749999898, 17.34687500061451715, -27.54997392385601529 ) ) ;
#22141 = ADVANCED_FACE ( 'NONE', ( #68402 ), #12603, .F. ) ;
#22142 = CARTESIAN_POINT ( 'NONE',  ( 8.212500000000000355, 2.886751345948129099, -4.999999999999998224 ) ) ;
#22143 = CARTESIAN_POINT ( 'NONE',  ( 5.925000001229033586, -5.773502691896255534, -1.060575238724906372E-15 ) ) ;
#22144 = CARTESIAN_POINT ( 'NONE',  ( 13.39687500061451608, -3.027376345333610441, -5.243569643749999898 ) ) ;
#22145 = CARTESIAN_POINT ( 'NONE',  ( 24.48750000122903359, 6.123233995736764310E-16, -4.999999999999998224 ) ) ;
#22146 = CARTESIAN_POINT ( 'NONE',  ( 3.759375000614517681, 0.000000000000000000, 5.243569643749999010 ) ) ;
#22147 = CARTESIAN_POINT ( 'NONE',  ( 28.16250000000000142, 2.886751345948119329, 5.000000000000014211 ) ) ;
#22148 = CARTESIAN_POINT ( 'NONE',  ( 10.00000000000000000, 1.224646799147353256E-15, -10.00000000000000888 ) ) ;
#22149 = CARTESIAN_POINT ( 'NONE',  ( 10.09687500061451715, -3.027376345333614438, 5.243569643749998122 ) ) ;
#22150 = CARTESIAN_POINT ( 'NONE',  ( 3.999999999999998668, 17.22500000122903430, -32.30940107675850470 ) ) ;
#22151 = CARTESIAN_POINT ( 'NONE',  ( 19.94062500061451715, -3.027376345333614438, 5.243569643749998122 ) ) ;
#22152 = CYLINDRICAL_SURFACE ( 'NONE', #51052, 4.000000000000000000 ) ;
#22153 = CARTESIAN_POINT ( 'NONE',  ( 4.243569643749999898, 18.19062500061459176, 32.45002607614398471 ) ) ;
#22154 = CARTESIAN_POINT ( 'NONE',  ( 24.12187500061451217, -6.054752690667223547, -1.112240025338166033E-15 ) ) ;
#22155 = CARTESIAN_POINT ( 'NONE',  ( 2.867942972713479755, -4.095717654485441450, 3.274159358307527690 ) ) ;
#22156 = CARTESIAN_POINT ( 'NONE',  ( 28.01250000122903216, -4.330127018922190985, -2.500000000000001332 ) ) ;
#22157 = CARTESIAN_POINT ( 'NONE',  ( 19.73437500061451289, 5.492252693125287522, 3.363034840372157021E-16 ) ) ;
#22158 = CARTESIAN_POINT ( 'NONE',  ( 24.62812500061451715, 6.421520780324663323E-16, -5.243569643749999010 ) ) ;
#22159 = CARTESIAN_POINT ( 'NONE',  ( 15.59062500061451573, -3.027376345333610441, -5.243569643749999898 ) ) ;
#22160 = CARTESIAN_POINT ( 'NONE',  ( 15.05625000122903323, 4.330127018922192761, -2.499999999999997780 ) ) ;
#22161 = CARTESIAN_POINT ( 'NONE',  ( 10.80937500061451928, 4.541064518000418104, -2.621784821874998173 ) ) ;
#22162 = FACE_OUTER_BOUND ( 'NONE', #33877, .T. ) ;
#22163 = CARTESIAN_POINT ( 'NONE',  ( 24.07500000122903216, 2.886751345948129099, -4.999999999999998224 ) ) ;
#22164 = CARTESIAN_POINT ( 'NONE',  ( 27.07499999999999929, 6.123233995736764310E-16, -4.999999999999998224 ) ) ;
#22165 = CARTESIAN_POINT ( 'NONE',  ( 13.05937500061451750, 4.541064518000418104, -2.621784821874998173 ) ) ;
#22166 = DIRECTION ( 'NONE',  ( 0.000000000000000000, 0.000000000000000000, -1.000000000000000000 ) ) ;
#22167 = CARTESIAN_POINT ( 'NONE',  ( -3.137519842735245283E-14, 11.56250000000000178, 34.00000000000000000 ) ) ;
#22168 = CARTESIAN_POINT ( 'NONE',  ( -2.000000000000000000, 12.27500000000000036, -33.46410161513775705 ) ) ;
#22169 = CARTESIAN_POINT ( 'NONE',  ( 24.49687500061451573, -3.027376345333614438, 5.243569643749998122 ) ) ;
#22170 = CARTESIAN_POINT ( 'NONE',  ( 17.63437500061451502, 4.541064518000418104, 2.621784821874999949 ) ) ;
#22171 = CARTESIAN_POINT ( 'NONE',  ( 3.756430356250000102, 16.80312499938548498, 30.00000000000000000 ) ) ;
#22172 = CARTESIAN_POINT ( 'NONE',  ( 28.46249999999999858, 2.886751345948129099, -4.999999999999998224 ) ) ;
#22173 = CARTESIAN_POINT ( 'NONE',  ( 4.387500001229033053, 4.330127018922191873, 2.499999999999999556 ) ) ;
#22174 = CARTESIAN_POINT ( 'NONE',  ( 4.837500000000001243, -2.886751345948129988, 4.999999999999997335 ) ) ;
#22175 = CARTESIAN_POINT ( 'NONE',  ( 8.034375000614515372, 5.492252693125287522, 3.363034840372157021E-16 ) ) ;
#22176 = CARTESIAN_POINT ( 'NONE',  ( 19.94062500061451715, -3.027376345333614438, 5.243569643749998122 ) ) ;
#22177 = CARTESIAN_POINT ( 'NONE',  ( 10.53750000000000320, 5.773502691896255534, 3.535250795749688894E-16 ) ) ;
#22178 = CARTESIAN_POINT ( 'NONE',  ( 2.878125000614517592, -4.541064518000419881, 2.621784821874995952 ) ) ;
#22179 = CARTESIAN_POINT ( 'NONE',  ( 16.83749999999999858, 5.773502691896255534, 3.535250795749688894E-16 ) ) ;
#22180 = CARTESIAN_POINT ( 'NONE',  ( -4.243569643749997233, 11.74062500061451786, 32.45002607614398471 ) ) ;
#22181 = FACE_OUTER_BOUND ( 'NONE', #4557, .T. ) ;
#22182 = CARTESIAN_POINT ( 'NONE',  ( 19.72500000122903074, 2.886751345948126879, 4.999999999999999112 ) ) ;
#22183 = CARTESIAN_POINT ( 'NONE',  ( -3.999999999999999112, 10.06250000000000178, -32.30940107675850470 ) ) ;
#22184 = CARTESIAN_POINT ( 'NONE',  ( 27.15937500061451360, 0.000000000000000000, 5.243569643749999010 ) ) ;
#22185 = EDGE_LOOP ( 'NONE', ( #62352, #5121, #41248, #61150 ) ) ;
#22186 = CARTESIAN_POINT ( 'NONE',  ( 16.26562500061451289, 3.027376345333611329, 5.243569643749999010 ) ) ;
#22187 = CARTESIAN_POINT ( 'NONE',  ( 21.14062500061451289, 6.054752690667223547, 3.707466751127219781E-16 ) ) ;
#22188 = CARTESIAN_POINT ( 'NONE',  ( 22.92187500061451644, 3.027376345333613106, -5.243569643749998122 ) ) ;
#22189 = CARTESIAN_POINT ( 'NONE',  ( 5.475000000000000533, 6.123233995736764310E-16, -4.999999999999998224 ) ) ;
#22190 = CARTESIAN_POINT ( 'NONE',  ( 9.478125000614515017, 4.541064518000418104, 2.621784821874999949 ) ) ;
#22191 = CARTESIAN_POINT ( 'NONE',  ( 25.34062500061451217, -3.027376345333614438, 5.243569643749998122 ) ) ;
#22192 = CARTESIAN_POINT ( 'NONE',  ( 13.84687500061451537, -3.027376345333610441, -5.243569643749999898 ) ) ;
#22193 = CARTESIAN_POINT ( 'NONE',  ( 18.87187500061451573, 3.027376345333613106, -5.243569643749998122 ) ) ;
#22194 = CARTESIAN_POINT ( 'NONE',  ( 34.99999999999999289, 2.500000000000000000, -3.500000000000000000 ) ) ;
#22195 = CARTESIAN_POINT ( 'NONE',  ( 2.121784821874999061, 17.40312500061451573, 26.32496088578401583 ) ) ;
#22196 = CARTESIAN_POINT ( 'NONE',  ( 21.11250000122903359, 0.000000000000000000, 4.999999999999998224 ) ) ;
#22197 = CARTESIAN_POINT ( 'NONE',  ( 17.63437500061451502, 4.119189519843966529, 2.378215178124999607 ) ) ;
#22198 = CARTESIAN_POINT ( 'NONE',  ( 12.70312500061451821, 0.000000000000000000, 5.243569643749999010 ) ) ;
#22199 = CARTESIAN_POINT ( 'NONE',  ( 5.071875000614519458, 3.027376345333611329, 5.243569643749999010 ) ) ;
#22200 = CARTESIAN_POINT ( 'NONE',  ( 5.671875000614519102, -6.054752690667223547, -1.112240025338166033E-15 ) ) ;
#22201 = ORIENTED_EDGE ( 'NONE', *, *, #45751, .T. ) ;
#22202 = CARTESIAN_POINT ( 'NONE',  ( 26.89687500061451431, -3.027376345333610441, -5.243569643749999898 ) ) ;
#22203 = CARTESIAN_POINT ( 'NONE',  ( 20.39062500061451644, -3.027376345333614438, 5.243569643749998122 ) ) ;
#22204 = CARTESIAN_POINT ( 'NONE',  ( 28.68750000122903288, 4.330127018922191873, 2.499999999999999556 ) ) ;
#22205 = CARTESIAN_POINT ( 'NONE',  ( 28.94062500061452070, -3.027376345333614438, 5.243569643749998122 ) ) ;
#22206 = CARTESIAN_POINT ( 'NONE',  ( 23.18437500061451573, -4.541064518000419881, 2.621784821874995952 ) ) ;
#22207 = CARTESIAN_POINT ( 'NONE',  ( 18.51562500061451289, 3.027376345333611329, 5.243569643749999010 ) ) ;
#22208 = CARTESIAN_POINT ( 'NONE',  ( -4.243569643749997233, 18.54687500061451289, 32.45002607614398471 ) ) ;
#22209 = CARTESIAN_POINT ( 'NONE',  ( 24.29062500061451502, 6.054752690667223547, 3.707466751127219781E-16 ) ) ;
#22210 = CARTESIAN_POINT ( 'NONE',  ( 5.287500001229035185, 4.330127018922191873, 2.499999999999999556 ) ) ;
#22211 = ORIENTED_EDGE ( 'NONE', *, *, #50947, .T. ) ;
#22212 = CARTESIAN_POINT ( 'NONE',  ( 27.22499999999999787, 4.330127018922191873, 2.499999999999999556 ) ) ;
#22213 = CARTESIAN_POINT ( 'NONE',  ( 8.484601909799253346E-16, 16.51249999999999929, -25.38119784648299770 ) ) ;
#22214 = CARTESIAN_POINT ( 'NONE',  ( 3.756430356250000546, 16.84062499938548285, 27.83122392262697886 ) ) ;
#22215 = CARTESIAN_POINT ( 'NONE',  ( 5.859375000614519102, 4.541064518000418104, -2.621784821874998173 ) ) ;
#22216 = CARTESIAN_POINT ( 'NONE',  ( 12.17812500061451608, 4.541064518000418104, 2.621784821874999949 ) ) ;
#22217 = CARTESIAN_POINT ( 'NONE',  ( 7.096875000614517148, -3.027376345333610441, -5.243569643749999898 ) ) ;
#22218 = CARTESIAN_POINT ( 'NONE',  ( 24.67500000122903359, 2.886751345948126879, 4.999999999999999112 ) ) ;
#22219 = CARTESIAN_POINT ( 'NONE',  ( 14.78437500061451715, 6.421520780324663323E-16, -5.243569643749999010 ) ) ;
#22220 = CARTESIAN_POINT ( 'NONE',  ( 3.609375000614516882, 4.541064518000418104, -2.621784821874998173 ) ) ;
#22221 = CARTESIAN_POINT ( 'NONE',  ( 28.27499999999999858, -4.330127018922194537, 2.499999999999995559 ) ) ;
#22222 = CARTESIAN_POINT ( 'NONE',  ( 27.30937500061451573, -4.541064518000417216, -2.621784821875001281 ) ) ;
#22223 = CARTESIAN_POINT ( 'NONE',  ( 2.840625000614518392, -3.027376345333614438, 5.243569643749998122 ) ) ;
#22224 = CARTESIAN_POINT ( 'NONE',  ( 12.40312500061451573, -4.541064518000417216, -2.621784821875001281 ) ) ;
#22225 = EDGE_LOOP ( 'NONE', ( #26581, #22134, #64367, #49664 ) ) ;
#22226 = CARTESIAN_POINT ( 'NONE',  ( 9.778125000614517504, 6.421520780324663323E-16, -5.243569643749999010 ) ) ;
#22227 = CARTESIAN_POINT ( 'NONE',  ( 8.953125000614518214, 4.541064518000418104, -2.621784821874998173 ) ) ;
#22228 = CARTESIAN_POINT ( 'NONE',  ( 18.68437500061451928, -4.119189519843968306, 2.378215178124996054 ) ) ;
#22229 = FACE_OUTER_BOUND ( 'NONE', #36458, .T. ) ;
#22230 = CARTESIAN_POINT ( 'NONE',  ( 16.01249999999999929, 2.886751345948126879, 4.999999999999999112 ) ) ;
#22231 = EDGE_CURVE ( 'NONE', #5140, #12584, #62030, .T. ) ;
#22232 = CARTESIAN_POINT ( 'NONE',  ( 15.15937500061451715, -4.541064518000417216, -2.621784821875001281 ) ) ;
#22233 = CARTESIAN_POINT ( 'NONE',  ( 14.06250000122903288, -4.330127018922190985, -2.500000000000001332 ) ) ;
#22234 = CARTESIAN_POINT ( 'NONE',  ( 19.20000000000000284, 0.000000000000000000, 4.999999999999998224 ) ) ;
#22235 = CARTESIAN_POINT ( 'NONE',  ( 19.99687500061451573, -3.027376345333614438, 5.243569643749998122 ) ) ;
#22236 = CARTESIAN_POINT ( 'NONE',  ( 2.121784821874999061, 15.15312500061451750, -33.67503911421598417 ) ) ;
#22237 = CARTESIAN_POINT ( 'NONE',  ( 21.52499999999999858, -4.330127018922194537, 2.499999999999995559 ) ) ;
#22238 = CARTESIAN_POINT ( 'NONE',  ( 24.98437500061451289, -2.746126346562641984, -4.756430356249999214 ) ) ;
#22239 = DIRECTION ( 'NONE',  ( 0.000000000000000000, 0.000000000000000000, 1.000000000000000000 ) ) ;
#22240 = MANIFOLD_SOLID_BREP ( 'Thread3', #65457 ) ;
#22241 = CARTESIAN_POINT ( 'NONE',  ( 25.90312500061451573, -4.541064518000417216, -2.621784821875001281 ) ) ;
#22242 = CARTESIAN_POINT ( 'NONE',  ( -1.071796769724490339, 19.64240381056766438, -26.00000000000000355 ) ) ;
#22243 = CARTESIAN_POINT ( 'NONE',  ( 50.00000000000000000, 1.494782592887768269, 8.874999999999984013 ) ) ;
#22244 = CARTESIAN_POINT ( 'NONE',  ( 27.22499999999999787, 4.330127018922191873, 2.499999999999999556 ) ) ;
#22245 = CARTESIAN_POINT ( 'NONE',  ( 9.065625000614517148, 3.027376345333611329, 5.243569643749999010 ) ) ;
#22246 = CARTESIAN_POINT ( 'NONE',  ( 28.24687500061451217, 4.119189519843966529, -2.378215178124998275 ) ) ;
#22247 = CARTESIAN_POINT ( 'NONE',  ( 22.58437500061451431, 4.541064518000418104, 2.621784821874999949 ) ) ;
#22248 = CARTESIAN_POINT ( 'NONE',  ( 12.57187500061451502, 4.119189519843966529, 2.378215178124999607 ) ) ;
#22249 = CARTESIAN_POINT ( 'NONE',  ( 6.178125000614518747, 6.421520780324663323E-16, -5.243569643749999010 ) ) ;
#22250 = CARTESIAN_POINT ( 'NONE',  ( 10.35937500061451644, 4.541064518000418104, -2.621784821874998173 ) ) ;
#22251 = EDGE_LOOP ( 'NONE', ( #13184, #46559, #62828, #59139 ) ) ;
#22252 = CARTESIAN_POINT ( 'NONE',  ( 21.45937500061451786, -4.541064518000417216, -2.621784821875001281 ) ) ;
#22253 = CARTESIAN_POINT ( 'NONE',  ( 30.00000000000000000, 0.000000000000000000, 0.000000000000000000 ) ) ;
#22254 = CARTESIAN_POINT ( 'NONE',  ( 29.81250000000000000, 2.886751345948129099, -4.999999999999998224 ) ) ;
#22255 = CARTESIAN_POINT ( 'NONE',  ( 5.625000000000001776, 4.330127018922191873, 2.499999999999999556 ) ) ;
#22256 = CARTESIAN_POINT ( 'NONE',  ( 15.37500000122903465, -5.773502691896255534, -1.060575238724906372E-15 ) ) ;
#22257 = CARTESIAN_POINT ( 'NONE',  ( 45.00000000000000000, 0.000000000000000000, 0.000000000000000000 ) ) ;
#22258 = CARTESIAN_POINT ( 'NONE',  ( 12.90000000000000213, 0.000000000000000000, 4.999999999999998224 ) ) ;
#22259 = ORIENTED_EDGE ( 'NONE', *, *, #25821, .T. ) ;
#22260 = CARTESIAN_POINT ( 'NONE',  ( 12.52500000000000213, -4.330127018922194537, 2.499999999999995559 ) ) ;
#22261 = CARTESIAN_POINT ( 'NONE',  ( 27.29062500061451502, -3.027376345333610441, -5.243569643749999898 ) ) ;
#22262 = CARTESIAN_POINT ( 'NONE',  ( 16.87500000000000000, 4.330127018922191873, 2.499999999999999556 ) ) ;
#22263 = CARTESIAN_POINT ( 'NONE',  ( 9.712500001229033231, 4.330127018922192761, -2.499999999999997780 ) ) ;
#22264 = CARTESIAN_POINT ( 'NONE',  ( 9.928125000614517859, 4.541064518000418104, 2.621784821874999949 ) ) ;
#22265 = CARTESIAN_POINT ( 'NONE',  ( 9.187500000000001776, 5.773502691896255534, 3.535250795749688894E-16 ) ) ;
#22266 = CARTESIAN_POINT ( 'NONE',  ( -5.810221930991193690E-16, 15.50000000122903465, 26.00000000000000355 ) ) ;
#22267 = CARTESIAN_POINT ( 'NONE',  ( -4.243569643749997233, 14.04687500061451999, -27.54997392385601174 ) ) ;
#22268 = CARTESIAN_POINT ( 'NONE',  ( 27.18750000122903288, 6.123233995736764310E-16, -4.999999999999998224 ) ) ;
#22269 = CARTESIAN_POINT ( 'NONE',  ( -1.878215178125001827, 15.64062499938548356, 33.25316411605952283 ) ) ;
#22270 = CARTESIAN_POINT ( 'NONE',  ( 8.250000000000000000, 4.330127018922192761, -2.499999999999997780 ) ) ;
#22271 = CARTESIAN_POINT ( 'NONE',  ( -2.000000000000000000, 12.72499999999999964, 26.53589838486224650 ) ) ;
#22272 = EDGE_LOOP ( 'NONE', ( #65872, #49571, #44174, #29777 ) ) ;
#22273 = CARTESIAN_POINT ( 'NONE',  ( 24.40312500061451573, 0.000000000000000000, 5.243569643749999010 ) ) ;
#22274 = CARTESIAN_POINT ( 'NONE',  ( 4.210772704977717495, -2.696194641284411109, 4.497291047846275980 ) ) ;
#22275 = CARTESIAN_POINT ( 'NONE',  ( 19.05000000122903003, -2.886751345948193048, -4.999999999999883649 ) ) ;
#22276 = CARTESIAN_POINT ( 'NONE',  ( 22.43437500061451573, 6.421520780324663323E-16, -5.243569643749999010 ) ) ;
#22277 = CARTESIAN_POINT ( 'NONE',  ( 15.66562500061451857, 3.027376345333613106, -5.243569643749998122 ) ) ;
#22278 = CARTESIAN_POINT ( 'NONE',  ( 4.243569643749999898, 10.99062500061459424, -27.54997392385601529 ) ) ;
#22279 = CARTESIAN_POINT ( 'NONE',  ( 7.753125000614518036, 0.000000000000000000, 5.243569643749999010 ) ) ;
#22280 = CARTESIAN_POINT ( 'NONE',  ( 29.36250000122903003, -4.330127018922190985, -2.500000000000001332 ) ) ;
#22281 = CARTESIAN_POINT ( 'NONE',  ( 24.19687500061451502, -2.746126346562641984, -4.756430356249999214 ) ) ;
#22282 = CARTESIAN_POINT ( 'NONE',  ( 18.55312500061451431, 0.000000000000000000, 5.243569643749999010 ) ) ;
#22283 = CARTESIAN_POINT ( 'NONE',  ( 13.35000000000000142, 0.000000000000000000, 4.999999999999998224 ) ) ;
#22284 = CARTESIAN_POINT ( 'NONE',  ( -3.756430356249999214, 19.57812499938548001, 27.83122392262697531 ) ) ;
#22285 = CARTESIAN_POINT ( 'NONE',  ( 14.52187500061451608, 3.027376345333611329, 5.243569643749999010 ) ) ;
#22286 = CARTESIAN_POINT ( 'NONE',  ( 15.27187500061451786, 3.027376345333613106, -5.243569643749998122 ) ) ;
#22287 = CARTESIAN_POINT ( 'NONE',  ( 22.73437500061451644, -4.541064518000419881, 2.621784821874995952 ) ) ;
#22288 = ORIENTED_EDGE ( 'NONE', *, *, #47314, .T. ) ;
#22289 = CARTESIAN_POINT ( 'NONE',  ( 3.365625000614516082, -6.054752690667223547, -1.112240025338166033E-15 ) ) ;
#22290 = CARTESIAN_POINT ( 'NONE',  ( 26.16562500061451502, 3.027376345333611329, 5.243569643749999010 ) ) ;
#22291 = CARTESIAN_POINT ( 'NONE',  ( 27.70312500061451289, -4.541064518000417216, -2.621784821875001281 ) ) ;
#22292 = CARTESIAN_POINT ( 'NONE',  ( -5.810221930991193690E-16, 10.55000000122903359, -34.00000000000000000 ) ) ;
#22293 = CARTESIAN_POINT ( 'NONE',  ( -2.828200636599751609E-16, 16.28749999999999787, 25.38119784648299770 ) ) ;
#22294 = CARTESIAN_POINT ( 'NONE',  ( 4.771875000614516971, -6.054752690667223547, -1.112240025338166033E-15 ) ) ;
#22295 = CARTESIAN_POINT ( 'NONE',  ( 11.25000000122903288, -2.886751345948129988, 4.999999999999997335 ) ) ;
#22296 = CARTESIAN_POINT ( 'NONE',  ( 6.937500001229033764, 6.123233995736764310E-16, -4.999999999999998224 ) ) ;
#22297 = CARTESIAN_POINT ( 'NONE',  ( 3.628125000614518036, 4.541064518000418104, 2.621784821874999949 ) ) ;
#22298 = CARTESIAN_POINT ( 'NONE',  ( 2.000000000000000444, 17.46874999877096712, 26.53589838486224650 ) ) ;
#22299 = CARTESIAN_POINT ( 'NONE',  ( 18.28125000122903288, 4.330127018922191873, 2.499999999999999556 ) ) ;
#22300 = CARTESIAN_POINT ( 'NONE',  ( 12.60937500061451821, 4.541064518000418104, -2.621784821874998173 ) ) ;
#22301 = CARTESIAN_POINT ( 'NONE',  ( 2.000000000000000444, 13.02500000000000036, 26.53589838486224650 ) ) ;
#22302 = ORIENTED_EDGE ( 'NONE', *, *, #11801, .F. ) ;
#22303 = CARTESIAN_POINT ( 'NONE',  ( 20.99062500061451431, -3.027376345333610441, -5.243569643749999898 ) ) ;
#22304 = CARTESIAN_POINT ( 'NONE',  ( 13.09687500061451892, 6.054752690667223547, 3.707466751127219781E-16 ) ) ;
#22305 = CARTESIAN_POINT ( 'NONE',  ( 4.378125000614518925, 6.421520780324663323E-16, -5.243569643749999010 ) ) ;
#22306 = CARTESIAN_POINT ( 'NONE',  ( 21.60937500061451644, 4.541064518000418104, -2.621784821874998173 ) ) ;
#22307 = CARTESIAN_POINT ( 'NONE',  ( 11.03437500061451715, -4.541064518000419881, 2.621784821874995952 ) ) ;
#22308 = CARTESIAN_POINT ( 'NONE',  ( 4.790625000614518569, -3.027376345333610441, -5.243569643749999898 ) ) ;
#22309 = LINE ( 'NONE', #37479, #13224 ) ;
#22310 = CARTESIAN_POINT ( 'NONE',  ( 6.562500001229032875, 4.330127018922192761, -2.499999999999997780 ) ) ;
#22311 = CARTESIAN_POINT ( 'NONE',  ( 20.84062500061451573, -3.027376345333614438, 5.243569643749998122 ) ) ;
#22312 = CARTESIAN_POINT ( 'NONE',  ( 7.087500001229034119, 4.330127018922191873, 2.499999999999999556 ) ) ;
#22313 = CARTESIAN_POINT ( 'NONE',  ( 17.42812500061451786, 6.421520780324663323E-16, -5.243569643749999010 ) ) ;
#22314 = CARTESIAN_POINT ( 'NONE',  ( 15.96562500061451573, -6.054752690667223547, -1.112240025338166033E-15 ) ) ;
#22315 = CARTESIAN_POINT ( 'NONE',  ( 24.87187500061451573, 2.746126346562643317, 4.756430356249998326 ) ) ;
#22316 = CARTESIAN_POINT ( 'NONE',  ( 16.50000000000000000, 0.000000000000000000, 4.999999999999998224 ) ) ;
#22317 = CARTESIAN_POINT ( 'NONE',  ( 9.337500001229033231, 4.330127018922191873, 2.499999999999999556 ) ) ;
#22318 = CARTESIAN_POINT ( 'NONE',  ( 6.703125000614516438, 4.541064518000418104, -2.621784821874998173 ) ) ;
#22319 = EDGE_CURVE ( 'NONE', #35328, #5464, #1195, .T. ) ;
#22320 = CARTESIAN_POINT ( 'NONE',  ( 20.06250000122903643, 4.330127018922192761, -2.499999999999997780 ) ) ;
#22321 = CARTESIAN_POINT ( 'NONE',  ( 25.91250000000000142, 2.886751345948126879, 4.999999999999999112 ) ) ;
#22322 = CARTESIAN_POINT ( 'NONE',  ( -4.243569643749997233, 11.34687500061451892, -27.54997392385601174 ) ) ;
#22323 = CARTESIAN_POINT ( 'NONE',  ( 21.41250000000000142, 2.886751345948126879, 4.999999999999998224 ) ) ;
#22324 = CARTESIAN_POINT ( 'NONE',  ( 3.637500001229036162, -4.330127018922194537, 2.499999999999995559 ) ) ;
#22325 = CARTESIAN_POINT ( 'NONE',  ( 4.134375000614517681, 4.541064518000418104, 2.621784821874999949 ) ) ;
#22326 = CARTESIAN_POINT ( 'NONE',  ( 21.27187500061451786, 3.027376345333611329, 5.243569643749999010 ) ) ;
#22327 =( BOUNDED_CURVE ( )  B_SPLINE_CURVE ( 2, ( #15163, #65045, #8532, #36244, #48435, #47328, #31436 ),
 .UNSPECIFIED., .F., .F. ) 
 B_SPLINE_CURVE_WITH_KNOTS ( ( 3, 2, 2, 3 ),
 ( 0.2999999999999999889, 0.3027777777777777568, 0.3055555555555555802, 0.3083333333333333481 ),
 .UNSPECIFIED. ) 
 CURVE ( )  GEOMETRIC_REPRESENTATION_ITEM ( )  RATIONAL_B_SPLINE_CURVE ( ( 1.000000000000000000, 0.8660254037844387076, 1.000000000000000000, 0.8660254037844387076, 1.000000000000000000, 0.8660254037844387076, 1.000000000000000000 ) ) 
 REPRESENTATION_ITEM ( '' )  );
#22328 = CARTESIAN_POINT ( 'NONE',  ( -3.999999999999999112, 15.05000000000000071, 30.00000000000000000 ) ) ;
#22329 = CARTESIAN_POINT ( 'NONE',  ( 16.82812500061451644, -4.541064518000419881, 2.621784821874995952 ) ) ;
#22330 = CARTESIAN_POINT ( 'NONE',  ( 12.73125000122903394, 6.123233995736764310E-16, -4.999999999999998224 ) ) ;
#22331 = CARTESIAN_POINT ( 'NONE',  ( 14.02499999999999858, 6.123233995736764310E-16, -4.999999999999998224 ) ) ;
#22332 = CYLINDRICAL_SURFACE ( 'NONE', #12290, 4.000000000000000000 ) ;
#22333 = CARTESIAN_POINT ( 'NONE',  ( 28.35937500061451289, 4.541064518000418104, -2.621784821874998173 ) ) ;
#22334 = CARTESIAN_POINT ( 'NONE',  ( 20.40937500061451360, -5.492252693125287522, -1.008910452111647106E-15 ) ) ;
#22335 = CARTESIAN_POINT ( 'NONE',  ( 13.22812500061451502, -4.541064518000419881, 2.621784821874995952 ) ) ;
#22336 = CARTESIAN_POINT ( 'NONE',  ( 11.29687500061451644, 6.054752690667223547, 3.707466751127219781E-16 ) ) ;
#22337 = ORIENTED_EDGE ( 'NONE', *, *, #16156, .T. ) ;
#22338 = CARTESIAN_POINT ( 'NONE',  ( 2.883025145109703313, -4.085149263999829472, -3.067080541767196245 ) ) ;
#22339 = CARTESIAN_POINT ( 'NONE',  ( 22.75312500061451360, -4.541064518000417216, -2.621784821875001281 ) ) ;
#22340 = CARTESIAN_POINT ( 'NONE',  ( 45.00000000000000000, 0.000000000000000000, 0.000000000000000000 ) ) ;
#22341 = DIRECTION ( 'NONE',  ( -1.000000000000000000, -0.000000000000000000, -0.000000000000000000 ) ) ;
#22342 = CARTESIAN_POINT ( 'NONE',  ( 11.36250000000000071, 2.886751345948129099, -4.999999999999998224 ) ) ;
#22343 = CARTESIAN_POINT ( 'NONE',  ( 20.96250000122903145, 4.330127018922192761, -2.499999999999997780 ) ) ;
#22344 = CARTESIAN_POINT ( 'NONE',  ( 15.96562500061451573, -6.054752690667223547, -1.112240025338166033E-15 ) ) ;
#22345 = CARTESIAN_POINT ( 'NONE',  ( 13.73437500061451644, -2.746126346562642428, -4.756430356249999214 ) ) ;
#22346 = ORIENTED_EDGE ( 'NONE', *, *, #32675, .F. ) ;
#22347 = CARTESIAN_POINT ( 'NONE',  ( 19.23749999999999716, -2.886751345948129988, 4.999999999999997335 ) ) ;
#22348 = CARTESIAN_POINT ( 'NONE',  ( 23.32499999999999929, -4.330127018922194537, 2.499999999999995559 ) ) ;
#22349 = CARTESIAN_POINT ( 'NONE',  ( 22.35937500061451644, -4.541064518000417216, -2.621784821875001281 ) ) ;
#22350 = CARTESIAN_POINT ( 'NONE',  ( 26.42812500061451431, 6.421520780324663323E-16, -5.243569643749999010 ) ) ;
#22351 = ORIENTED_EDGE ( 'NONE', *, *, #38259, .T. ) ;
#22352 = LINE ( 'NONE', #67078, #66677 ) ;
#22353 = CARTESIAN_POINT ( 'NONE',  ( 9.478125000614515017, 4.541064518000418104, 2.621784821874999949 ) ) ;
#22354 = CARTESIAN_POINT ( 'NONE',  ( 6.375000000000001776, 6.123233995736764310E-16, -4.999999999999998224 ) ) ;
#22355 = CARTESIAN_POINT ( 'NONE',  ( 13.57500000000000107, 6.123233995736764310E-16, -4.999999999999998224 ) ) ;
#22356 = CARTESIAN_POINT ( 'NONE',  ( 4.243569643749999898, 19.57812500061451644, 30.00000000000000000 ) ) ;
#22357 = CARTESIAN_POINT ( 'NONE',  ( 4.059375000614519280, 4.541064518000418104, -2.621784821874998173 ) ) ;
#22358 = CARTESIAN_POINT ( 'NONE',  ( 28.80937500061451573, 4.541064518000418104, -2.621784821874998173 ) ) ;
#22359 = ORIENTED_EDGE ( 'NONE', *, *, #26472, .F. ) ;
#22360 = CARTESIAN_POINT ( 'NONE',  ( 23.72812500061451502, 6.421520780324663323E-16, -5.243569643749999010 ) ) ;
#22361 = CARTESIAN_POINT ( 'NONE',  ( 25.54687500061451644, -3.027376345333610441, -5.243569643749999898 ) ) ;
#22362 = CARTESIAN_POINT ( 'NONE',  ( 2.121784821875001281, 19.50312500061459176, -26.32496088578401938 ) ) ;
#22363 = CARTESIAN_POINT ( 'NONE',  ( 11.96250000000000213, 2.886751345948126879, 4.999999999999999112 ) ) ;
#22364 = CARTESIAN_POINT ( 'NONE',  ( 8.053125000614516082, 4.541064518000418104, -2.621784821874998173 ) ) ;
#22365 = CARTESIAN_POINT ( 'NONE',  ( 3.829234068599516760, 3.215278937808554005, 3.875698639894808117 ) ) ;
#22366 = CARTESIAN_POINT ( 'NONE',  ( 13.46249999999999858, -5.773502691896255534, -1.060575238724906372E-15 ) ) ;
#22367 = CARTESIAN_POINT ( 'NONE',  ( 27.10312500061451502, 0.000000000000000000, 5.243569643749999010 ) ) ;
#22368 = CARTESIAN_POINT ( 'NONE',  ( 23.75625000122903074, 0.000000000000000000, 4.999999999999998224 ) ) ;
#22369 = CARTESIAN_POINT ( 'NONE',  ( 15.53437500061451715, -4.119189519843968306, 2.378215178124996054 ) ) ;
#22370 = CARTESIAN_POINT ( 'NONE',  ( 4.040625000614517681, 6.054752690667223547, 3.707466751127219781E-16 ) ) ;
#22371 = CARTESIAN_POINT ( 'NONE',  ( 20.40937500061451715, 0.000000000000000000, 5.243569643749999010 ) ) ;
#22372 = CARTESIAN_POINT ( 'NONE',  ( 4.243569643749999898, 15.09687500061451892, 32.45002607614398471 ) ) ;
#22373 = CARTESIAN_POINT ( 'NONE',  ( 21.64687500061451786, 6.054752690667223547, 3.707466751127219781E-16 ) ) ;
#22374 = CARTESIAN_POINT ( 'NONE',  ( 29.37187500061451928, 3.027376345333611329, 5.243569643749999010 ) ) ;
#22375 = CARTESIAN_POINT ( 'NONE',  ( 4.243569643749999898, 19.59687500061451360, 32.45002607614398471 ) ) ;
#22376 = CARTESIAN_POINT ( 'NONE',  ( 9.890625000614516438, 6.054752690667223547, 3.707466751127219781E-16 ) ) ;
#22377 = CARTESIAN_POINT ( 'NONE',  ( 2.812500001229033320, -4.330127018922190985, -2.500000000000001332 ) ) ;
#22378 = EDGE_CURVE ( 'NONE', #61146, #18509, #56836, .T. ) ;
#22379 = CARTESIAN_POINT ( 'NONE',  ( 7.209375000614519635, 4.541064518000418104, -2.621784821874998173 ) ) ;
#22380 = CARTESIAN_POINT ( 'NONE',  ( 11.60625000122903216, 0.000000000000000000, 4.999999999999998224 ) ) ;
#22381 = ADVANCED_FACE ( 'NONE', ( #17052 ), #39609, .T. ) ;
#22382 = CARTESIAN_POINT ( 'NONE',  ( 6.853125000614516793, 0.000000000000000000, 5.243569643749999010 ) ) ;
#22383 = CARTESIAN_POINT ( 'NONE',  ( 12.57187500061451857, 3.027376345333613106, -5.243569643749998122 ) ) ;
#22384 = CARTESIAN_POINT ( 'NONE',  ( 18.67500000122903714, 2.886751345948129099, -4.999999999999998224 ) ) ;
#22385 = CARTESIAN_POINT ( 'NONE',  ( 7.396875000614519635, -3.027376345333614438, 5.243569643749998122 ) ) ;
#22386 = CARTESIAN_POINT ( 'NONE',  ( 9.178125000614517859, -4.541064518000419881, 2.621784821874995952 ) ) ;
#22387 = CARTESIAN_POINT ( 'NONE',  ( 4.648177544792955741E-15, 14.58124999877096606, 33.99999999999999289 ) ) ;
#22388 = CARTESIAN_POINT ( 'NONE',  ( 25.21875000122903288, -5.773502691896255534, -1.060575238724906372E-15 ) ) ;
#22389 = CARTESIAN_POINT ( 'NONE',  ( 19.88437500061451857, 4.541064518000418104, 2.621784821874999949 ) ) ;
#22390 = CARTESIAN_POINT ( 'NONE',  ( 18.07499999999999929, 6.123233995736764310E-16, -4.999999999999998224 ) ) ;
#22391 = CARTESIAN_POINT ( 'NONE',  ( 28.04062500061451502, -3.027376345333614438, 5.243569643749998122 ) ) ;
#22392 = CARTESIAN_POINT ( 'NONE',  ( 12.74062500061451786, -3.027376345333614438, 5.243569643749998122 ) ) ;
#22393 = CARTESIAN_POINT ( 'NONE',  ( 50.00000000000000000, -8.875000000000000000, 1.494782592887675232 ) ) ;
#22394 = CARTESIAN_POINT ( 'NONE',  ( 4.243569643749999898, 11.98437500061451821, -30.00000000000000000 ) ) ;
#22395 = EDGE_CURVE ( 'NONE', #2080, #39643, #18202, .T. ) ;
#22396 = CARTESIAN_POINT ( 'NONE',  ( 12.63750000122903394, -4.330127018922194537, 2.499999999999995559 ) ) ;
#22397 = CARTESIAN_POINT ( 'NONE',  ( 27.44062500061451715, 6.054752690667223547, 3.707466751127219781E-16 ) ) ;
#22398 = CARTESIAN_POINT ( 'NONE',  ( 2.121784821874999061, 15.15312500061451750, -33.67503911421598417 ) ) ;
#22399 = CARTESIAN_POINT ( 'NONE',  ( 15.67500000122903181, 2.886751345948126879, 4.999999999999999112 ) ) ;
#22400 = CARTESIAN_POINT ( 'NONE',  ( 12.37500000000000000, 4.330127018922191873, 2.499999999999999556 ) ) ;
#22401 = CARTESIAN_POINT ( 'NONE',  ( -1.071796769724491005, 13.60759618943233384, 26.00000000000000355 ) ) ;
#22402 = CARTESIAN_POINT ( 'NONE',  ( 22.07812500061451644, 4.541064518000418104, 2.621784821874999949 ) ) ;
#22403 = CARTESIAN_POINT ( 'NONE',  ( 7.096875000614518036, -3.027376345333610441, -5.243569643749999898 ) ) ;
#22404 = EDGE_CURVE ( 'NONE', #46196, #39643, #46957, .T. ) ;
#22405 = CARTESIAN_POINT ( 'NONE',  ( 6.825000001229034829, -5.773502691896255534, -1.060575238724906372E-15 ) ) ;
#22406 = CARTESIAN_POINT ( 'NONE',  ( 15.33750000122903323, -4.330127018922194537, 2.499999999999995559 ) ) ;
#22407 = CARTESIAN_POINT ( 'NONE',  ( 12.44062500061451537, -3.027376345333610441, -5.243569643749999898 ) ) ;
#22408 = CARTESIAN_POINT ( 'NONE',  ( 17.31562500061451715, -6.054752690667223547, -1.112240025338166033E-15 ) ) ;
#22409 = CARTESIAN_POINT ( 'NONE',  ( 25.35000000122903074, -2.886751345948125991, -5.000000000000000000 ) ) ;
#22410 = CARTESIAN_POINT ( 'NONE',  ( 29.21250000122903145, 0.000000000000000000, 4.999999999999998224 ) ) ;
#22411 = CARTESIAN_POINT ( 'NONE',  ( 22.98749999999999716, -2.886751345948125991, -5.000000000000000000 ) ) ;
#22412 = CARTESIAN_POINT ( 'NONE',  ( 24.87187500061451573, 3.027376345333611329, 5.243569643749999010 ) ) ;
#22413 = CARTESIAN_POINT ( 'NONE',  ( 25.80000000122903359, -2.886751345948109559, -5.000000000000028422 ) ) ;
#22414 = CARTESIAN_POINT ( 'NONE',  ( 9.375000001229036428, 2.886751345948126879, 4.999999999999999112 ) ) ;
#22415 = CARTESIAN_POINT ( 'NONE',  ( 28.47187500061451715, 3.027376345333611329, 5.243569643749999010 ) ) ;
#22416 = CARTESIAN_POINT ( 'NONE',  ( 4.884375000614518569, 6.421520780324663323E-16, -5.243569643749999010 ) ) ;
#22417 = CARTESIAN_POINT ( 'NONE',  ( 23.42812500061451786, 4.541064518000418104, 2.621784821874999949 ) ) ;
#22418 = CARTESIAN_POINT ( 'NONE',  ( 2.655984681222220721E-16, 14.21562499938548285, 25.66244784525396483 ) ) ;
#22419 = CARTESIAN_POINT ( 'NONE',  ( 4.544497808834801589, -2.085075457992688897, -4.544497808831748920 ) ) ;
#22420 = CARTESIAN_POINT ( 'NONE',  ( 9.159375000614515372, 0.000000000000000000, 5.243569643749999010 ) ) ;
#22421 = DIRECTION ( 'NONE',  ( -1.000000000000000000, -0.000000000000000000, -0.000000000000000000 ) ) ;
#22422 = CARTESIAN_POINT ( 'NONE',  ( 3.234375000614516438, 4.541064518000418104, 2.621784821874999949 ) ) ;
#22423 = CARTESIAN_POINT ( 'NONE',  ( 5.559375000614517504, 0.000000000000000000, 5.243569643749999010 ) ) ;
#22424 = PLANE ( 'NONE',  #43113 ) ;
#22425 = CARTESIAN_POINT ( 'NONE',  ( 27.72187500061451715, -6.054752690667223547, -1.112240025338166033E-15 ) ) ;
#22426 = LINE ( 'NONE', #55689, #17215 ) ;
#22427 = CARTESIAN_POINT ( 'NONE',  ( 19.38749999999999929, -2.886751345948125991, -5.000000000000000000 ) ) ;
#22428 = ORIENTED_EDGE ( 'NONE', *, *, #8538, .T. ) ;
#22429 = CARTESIAN_POINT ( 'NONE',  ( 26.73749999999999716, 5.773502691896255534, 3.535250795749688894E-16 ) ) ;
#22430 = CARTESIAN_POINT ( 'NONE',  ( 27.90937500061451715, 4.541064518000418104, -2.621784821874998173 ) ) ;
#22431 = ORIENTED_EDGE ( 'NONE', *, *, #53850, .T. ) ;
#22432 = CARTESIAN_POINT ( 'NONE',  ( 14.50312500061451537, 0.000000000000000000, 5.243569643749999010 ) ) ;
#22433 = CARTESIAN_POINT ( 'NONE',  ( 7.378125000614518036, -4.541064518000419881, 2.621784821874995952 ) ) ;
#22434 = CARTESIAN_POINT ( 'NONE',  ( 20.44687500061451502, -4.119189519843965641, -2.378215178125001383 ) ) ;
#22435 = CARTESIAN_POINT ( 'NONE',  ( 5.259375000614518569, -4.541064518000417216, -2.621784821875001281 ) ) ;
#22436 = CARTESIAN_POINT ( 'NONE',  ( 18.82500000122903216, 2.886751345948126879, 4.999999999999999112 ) ) ;
#22437 = CARTESIAN_POINT ( 'NONE',  ( 23.88749999999999929, -2.886751345948125991, -5.000000000000000000 ) ) ;
#22438 = CARTESIAN_POINT ( 'NONE',  ( 7.996875000614519280, -3.027376345333610441, -5.243569643749999898 ) ) ;
#22439 = CARTESIAN_POINT ( 'NONE',  ( 12.45937500061451786, -4.541064518000417216, -2.621784821875001281 ) ) ;
#22440 = CARTESIAN_POINT ( 'NONE',  ( 21.12187500061451573, 3.027376345333613106, -5.243569643749998122 ) ) ;
#22441 = LINE ( 'NONE', #38723, #41879 ) ;
#22442 = EDGE_LOOP ( 'NONE', ( #35606, #63871 ) ) ;
#22443 = CARTESIAN_POINT ( 'NONE',  ( 3.721875000614518036, 3.027376345333611329, 5.243569643749999010 ) ) ;
#22444 = CARTESIAN_POINT ( 'NONE',  ( 10.87500000000000000, 6.123233995736764310E-16, -4.999999999999998224 ) ) ;
#22445 = CARTESIAN_POINT ( 'NONE',  ( 7.284375000614518036, 4.541064518000418104, 2.621784821874999949 ) ) ;
#22446 = CARTESIAN_POINT ( 'NONE',  ( 20.62499999999999645, -4.330127018922194537, 2.499999999999995559 ) ) ;
#22447 = CARTESIAN_POINT ( 'NONE',  ( 14.99062500061451786, -3.027376345333614438, 5.243569643749998122 ) ) ;
#22448 = CARTESIAN_POINT ( 'NONE',  ( 1.999999999999997335, 17.37500000000000000, 33.46410161513775705 ) ) ;
#22449 = DIRECTION ( 'NONE',  ( -1.000000000000000000, -0.000000000000000000, -0.000000000000000000 ) ) ;
#22450 = CARTESIAN_POINT ( 'NONE',  ( 21.90937500061451715, -4.119189519843965641, -2.378215178125001383 ) ) ;
#22451 = CARTESIAN_POINT ( 'NONE',  ( 10.45312500061451644, 0.000000000000000000, 5.243569643749999010 ) ) ;
#22452 = CARTESIAN_POINT ( 'NONE',  ( 26.97187500061451360, 3.027376345333613106, -5.243569643749998122 ) ) ;
#22453 = CYLINDRICAL_SURFACE ( 'NONE', #38402, 4.999999999999998224 ) ;
#22454 = CARTESIAN_POINT ( 'NONE',  ( 28.20937500061451786, -4.541064518000417216, -2.621784821875001281 ) ) ;
#22455 = CARTESIAN_POINT ( 'NONE',  ( 9.600000000000001421, 4.330127018922192761, -2.499999999999997780 ) ) ;
#22456 = CARTESIAN_POINT ( 'NONE',  ( -2.000000000000000000, 14.63750000122903394, 26.53589838486224650 ) ) ;
#22457 = CARTESIAN_POINT ( 'NONE',  ( 8.700000001229032165, -2.886751345948125991, -5.000000000000000000 ) ) ;
#22458 = CARTESIAN_POINT ( 'NONE',  ( 18.94687500061451502, 6.054752690667223547, 3.707466751127219781E-16 ) ) ;
#22459 = CARTESIAN_POINT ( 'NONE',  ( 14.97187500061451892, 3.027376345333611329, 5.243569643749999010 ) ) ;
#22460 = LINE ( 'NONE', #12825, #54852 ) ;
#22461 = ORIENTED_EDGE ( 'NONE', *, *, #33073, .T. ) ;
#22462 = CARTESIAN_POINT ( 'NONE',  ( 14.27812500061451573, 6.421520780324663323E-16, -5.243569643749999010 ) ) ;
#22463 = CARTESIAN_POINT ( 'NONE',  ( 25.12500000122903288, 2.886751345948126879, 4.999999999999999112 ) ) ;
#22464 = CARTESIAN_POINT ( 'NONE',  ( 16.17187500061451644, 3.027376345333613106, -5.243569643749998122 ) ) ;
#22465 = CARTESIAN_POINT ( 'NONE',  ( 7.612500001229035362, 0.000000000000000000, 4.999999999999998224 ) ) ;
#22466 = CARTESIAN_POINT ( 'NONE',  ( 16.67812500061451786, 4.541064518000418104, 2.621784821874999949 ) ) ;
#22467 = CARTESIAN_POINT ( 'NONE',  ( 18.48750000000000071, -2.886751345948126435, -5.000000000000000000 ) ) ;
#22468 = CARTESIAN_POINT ( 'NONE',  ( 25.65937500061451715, 4.541064518000418104, -2.621784821874998173 ) ) ;
#22469 = CARTESIAN_POINT ( 'NONE',  ( -4.243569643749999898, 11.25312500061451892, 30.00000000000000000 ) ) ;
#22470 = CARTESIAN_POINT ( 'NONE',  ( 15.23437500061451644, 6.421520780324663323E-16, -5.243569643749999010 ) ) ;
#22471 = CARTESIAN_POINT ( 'NONE',  ( 14.25000000122903465, 5.773502691896255534, 3.535250795749688894E-16 ) ) ;
#22472 = CYLINDRICAL_SURFACE ( 'NONE', #4495, 3.999999999999996447 ) ;
#22473 = CARTESIAN_POINT ( 'NONE',  ( -2.121784821874999949, 18.88437500061451857, -33.67503911421598417 ) ) ;
#22474 = EDGE_CURVE ( 'NONE', #14695, #24785, #70578, .T. ) ;
#22475 = CARTESIAN_POINT ( 'NONE',  ( 19.05937500061451928, 0.000000000000000000, 5.243569643749999010 ) ) ;
#22476 = CARTESIAN_POINT ( 'NONE',  ( 19.91250000122903074, -4.330127018922190985, -2.500000000000001332 ) ) ;
#22477 = CARTESIAN_POINT ( 'NONE',  ( 15.75937500061451857, 4.541064518000418104, -2.621784821874998173 ) ) ;
#22478 = CARTESIAN_POINT ( 'NONE',  ( 4.243569643749999898, 11.49687500061451928, 32.45002607614398471 ) ) ;
#22479 = CARTESIAN_POINT ( 'NONE',  ( 21.67500000122903359, -5.773502691896255534, -1.060575238724906372E-15 ) ) ;
#22480 = CARTESIAN_POINT ( 'NONE',  ( 18.47812500061451857, 4.541064518000418104, 2.621784821874999949 ) ) ;
#22481 = ORIENTED_EDGE ( 'NONE', *, *, #25529, .F. ) ;
#22482 = ORIENTED_EDGE ( 'NONE', *, *, #7942, .T. ) ;
#22483 = CARTESIAN_POINT ( 'NONE',  ( 21.11249999999999716, -5.773502691896255534, -1.060575238724906372E-15 ) ) ;
#22484 = CARTESIAN_POINT ( 'NONE',  ( -2.672702088255949472E-15, 13.45624999877096784, 26.00000000000000000 ) ) ;
#22485 = CARTESIAN_POINT ( 'NONE',  ( 22.79062500061451502, -3.027376345333610441, -5.243569643749999898 ) ) ;
#22486 = CARTESIAN_POINT ( 'NONE',  ( 4.003125000614518925, 4.541064518000418104, -2.621784821874998173 ) ) ;
#22487 = CARTESIAN_POINT ( 'NONE',  ( 18.56250000122903288, -4.330127018922190985, -2.500000000000001332 ) ) ;
#22488 = CARTESIAN_POINT ( 'NONE',  ( 21.51562500061451644, 3.027376345333613106, -5.243569643749998122 ) ) ;
#22489 =( BOUNDED_CURVE ( )  B_SPLINE_CURVE ( 2, ( #68848, #1617, #57020, #62926, #6425, #24126, #28958 ),
 .UNSPECIFIED., .F., .F. ) 
 B_SPLINE_CURVE_WITH_KNOTS ( ( 3, 2, 2, 3 ),
 ( 0.7916666666666666297, 0.7944444444444443976, 0.7972222222222222765, 0.8000000000000000444 ),
 .UNSPECIFIED. ) 
 CURVE ( )  GEOMETRIC_REPRESENTATION_ITEM ( )  RATIONAL_B_SPLINE_CURVE ( ( 1.000000000000000000, 0.8660254037844387076, 1.000000000000000000, 0.8660254037844387076, 1.000000000000000000, 0.8660254037844387076, 1.000000000000000000 ) ) 
 REPRESENTATION_ITEM ( '' )  );
#22490 = CARTESIAN_POINT ( 'NONE',  ( 26.46562500061451573, 3.027376345333613106, -5.243569643749998122 ) ) ;
#22491 = CARTESIAN_POINT ( 'NONE',  ( 6.478125000614516793, -4.541064518000419881, 2.621784821874995952 ) ) ;
#22492 = ORIENTED_EDGE ( 'NONE', *, *, #21050, .F. ) ;
#22493 = CARTESIAN_POINT ( 'NONE',  ( 29.09999999999999787, 0.000000000000000000, 4.999999999999998224 ) ) ;
#22494 = CARTESIAN_POINT ( 'NONE',  ( -1.999999999999997113, 10.28750000122903430, -26.53589838486224295 ) ) ;
#22495 = CARTESIAN_POINT ( 'NONE',  ( 11.25937500061451679, 4.119189519843966529, -2.378215178124998275 ) ) ;
#22496 = FACE_OUTER_BOUND ( 'NONE', #50799, .T. ) ;
#22497 = CARTESIAN_POINT ( 'NONE',  ( 3.999999999999999112, 10.43750000122903465, -30.00000000000000000 ) ) ;
#22498 = CARTESIAN_POINT ( 'NONE',  ( 4.243569643749999898, 19.18437500061451928, -30.00000000000000000 ) ) ;
#22499 = EDGE_CURVE ( 'NONE', #26592, #72158, #69576, .T. ) ;
#22500 = CARTESIAN_POINT ( 'NONE',  ( 6.937500001229033764, 6.123233995736764310E-16, -4.999999999999998224 ) ) ;
#22501 = CARTESIAN_POINT ( 'NONE',  ( 7.350000000000002309, 4.330127018922192761, -2.499999999999997780 ) ) ;
#22502 = CARTESIAN_POINT ( 'NONE',  ( 4.387500001229033053, 4.330127018922191873, 2.499999999999999556 ) ) ;
#22503 = CARTESIAN_POINT ( 'NONE',  ( 11.44687500061451857, -3.027376345333614438, 5.243569643749998122 ) ) ;
#22504 = CARTESIAN_POINT ( 'NONE',  ( 19.38750000122903216, -4.330127018922194537, 2.499999999999995559 ) ) ;
#22505 = CARTESIAN_POINT ( 'NONE',  ( 14.53125000122903288, 6.123233995736764310E-16, -4.999999999999998224 ) ) ;
#22506 = CARTESIAN_POINT ( 'NONE',  ( 24.28125000122903288, -4.330127018922194537, 2.499999999999995559 ) ) ;
#22507 = CARTESIAN_POINT ( 'NONE',  ( 10.58437500061451964, -4.541064518000419881, 2.621784821874995952 ) ) ;
#22508 = CARTESIAN_POINT ( 'NONE',  ( 29.83125000061451715, 0.000000000000000000, 5.243569643749999010 ) ) ;
#22509 = EDGE_CURVE ( 'NONE', #57768, #60913, #67857, .T. ) ;
#22510 = CARTESIAN_POINT ( 'NONE',  ( 18.89062500061451644, 6.054752690667223547, 3.707466751127219781E-16 ) ) ;
#22511 = CARTESIAN_POINT ( 'NONE',  ( 1.071796769724489895, 14.46740381056766545, 26.00000000000000355 ) ) ;
#22512 = CARTESIAN_POINT ( 'NONE',  ( 9.001249775931846008E-16, 17.21562500061459744, 34.90005215228797653 ) ) ;
#22513 = CARTESIAN_POINT ( 'NONE',  ( 21.90937500061451715, -4.541064518000417216, -2.621784821875001281 ) ) ;
#22514 = FACE_OUTER_BOUND ( 'NONE', #11022, .T. ) ;
#22515 = CARTESIAN_POINT ( 'NONE',  ( 27.93750000122903288, -4.330127018922194537, 2.499999999999995559 ) ) ;
#22516 = CARTESIAN_POINT ( 'NONE',  ( 17.59687500061451360, 0.000000000000000000, 4.756430356249998326 ) ) ;
#22517 = CARTESIAN_POINT ( 'NONE',  ( 25.19062500061451715, 6.054752690667223547, 3.707466751127219781E-16 ) ) ;
#22518 = CARTESIAN_POINT ( 'NONE',  ( 15.40312500061451573, 0.000000000000000000, 5.243569643749999010 ) ) ;
#22519 = CARTESIAN_POINT ( 'NONE',  ( 14.26875000122903536, 2.886751345948126879, 4.999999999999999112 ) ) ;
#22520 = CARTESIAN_POINT ( 'NONE',  ( 11.18437500061451928, 6.421520780324663323E-16, -5.243569643749999010 ) ) ;
#22521 = CARTESIAN_POINT ( 'NONE',  ( 28.68749999999999645, -2.886751345948129988, 4.999999999999997335 ) ) ;
#22522 = CARTESIAN_POINT ( 'NONE',  ( 25.31250000122903288, -4.330127018922190985, -2.500000000000001332 ) ) ;
#22523 = CARTESIAN_POINT ( 'NONE',  ( 3.871875000614519280, -6.054752690667223547, -1.112240025338166033E-15 ) ) ;
#22524 = CARTESIAN_POINT ( 'NONE',  ( 15.42187500061451821, 3.027376345333611329, 5.243569643749999010 ) ) ;
#22525 = CARTESIAN_POINT ( 'NONE',  ( 29.48437500061451644, -4.541064518000419881, 2.621784821874995952 ) ) ;
#22526 = CARTESIAN_POINT ( 'NONE',  ( 2.393811435568372112E-14, 16.88750000000000284, 34.00000000000000000 ) ) ;
#22527 = CARTESIAN_POINT ( 'NONE',  ( 1.626862140677534273E-15, 12.46250000000000213, -26.00000000000000355 ) ) ;
#22528 = CARTESIAN_POINT ( 'NONE',  ( 22.47187500061451715, 3.027376345333613106, -5.243569643749998122 ) ) ;
#22529 = CARTESIAN_POINT ( 'NONE',  ( 13.92187500061451644, 3.027376345333613106, -5.243569643749998122 ) ) ;
#22530 = CARTESIAN_POINT ( 'NONE',  ( -3.756430356250000102, 16.57812499938548356, 30.00000000000000000 ) ) ;
#22531 = CARTESIAN_POINT ( 'NONE',  ( 28.23750000000000426, -2.886751345948129988, 4.999999999999997335 ) ) ;
#22532 = CARTESIAN_POINT ( 'NONE',  ( 2.962500001229034119, 4.330127018922192761, -2.499999999999997780 ) ) ;
#22533 = CARTESIAN_POINT ( 'NONE',  ( 7.246875000614514839, 0.000000000000000000, 4.756430356249998326 ) ) ;
#22534 = CARTESIAN_POINT ( 'NONE',  ( 17.87812500061451715, 6.421520780324663323E-16, -5.243569643749999010 ) ) ;
#22535 = CARTESIAN_POINT ( 'NONE',  ( 6.337499999999998579, -2.886751345948125991, -5.000000000000000000 ) ) ;
#22536 =( BOUNDED_CURVE ( )  B_SPLINE_CURVE ( 2, ( #19882, #2541, #49079, #20981, #30977, #70870, #64590 ),
 .UNSPECIFIED., .F., .F. ) 
 B_SPLINE_CURVE_WITH_KNOTS ( ( 3, 2, 2, 3 ),
 ( 0.2900000000000000355, 0.2933333333333333903, 0.2966666666666666896, 0.2999999999999999889 ),
 .UNSPECIFIED. ) 
 CURVE ( )  GEOMETRIC_REPRESENTATION_ITEM ( )  RATIONAL_B_SPLINE_CURVE ( ( 0.9999999999999977796, 0.8660254037844409281, 1.000000000000000000, 0.8660254037844387076, 1.000000000000000000, 0.8660254037844387076, 1.000000000000000000 ) ) 
 REPRESENTATION_ITEM ( '' )  );
#22537 = CARTESIAN_POINT ( 'NONE',  ( 17.02499999999999858, -4.330127018922194537, 2.499999999999995559 ) ) ;
#22538 = CARTESIAN_POINT ( 'NONE',  ( -4.243569643749999898, 12.15312500061451573, 30.00000000000000000 ) ) ;
#22539 = CARTESIAN_POINT ( 'NONE',  ( 24.76875000122903003, -5.773502691896255534, -1.060575238724906372E-15 ) ) ;
#22540 = CARTESIAN_POINT ( 'NONE',  ( 21.33750000122903145, 6.123233995736764310E-16, -4.999999999999998224 ) ) ;
#22541 = CARTESIAN_POINT ( 'NONE',  ( 11.34375000122903465, -2.886751345948126435, -5.000000000000000000 ) ) ;
#22542 = CARTESIAN_POINT ( 'NONE',  ( 26.52187500061451431, 3.027376345333613106, -5.243569643749998122 ) ) ;
#22543 = ORIENTED_EDGE ( 'NONE', *, *, #62922, .T. ) ;
#22544 = CARTESIAN_POINT ( 'NONE',  ( 21.96562500061451573, 3.027376345333613106, -5.243569643749998122 ) ) ;
#22545 = CARTESIAN_POINT ( 'NONE',  ( 22.62187500061451573, 3.027376345333611329, 5.243569643749999010 ) ) ;
#22546 = CARTESIAN_POINT ( 'NONE',  ( 5.924999999999999822, 6.123233995736764310E-16, -4.999999999999998224 ) ) ;
#22547 = CARTESIAN_POINT ( 'NONE',  ( 10.15312500061451750, -4.541064518000417216, -2.621784821875001281 ) ) ;
#22548 = CARTESIAN_POINT ( 'NONE',  ( 24.21562500061451573, 3.027376345333613106, -5.243569643749998122 ) ) ;
#22549 = CARTESIAN_POINT ( 'NONE',  ( 13.88437500061451679, 6.421520780324663323E-16, -5.243569643749999010 ) ) ;
#22550 = CARTESIAN_POINT ( 'NONE',  ( 18.08437500061451431, 4.541064518000418104, 2.621784821874999949 ) ) ;
#22551 = LINE ( 'NONE', #56536, #21510 ) ;
#22552 = CARTESIAN_POINT ( 'NONE',  ( -2.121784821874999949, 17.47812500061451502, 26.32496088578401938 ) ) ;
#22553 = CARTESIAN_POINT ( 'NONE',  ( 22.35000000122903074, 5.773502691896255534, 3.535250795749688894E-16 ) ) ;
#22554 = CARTESIAN_POINT ( 'NONE',  ( 13.84687500061451537, -2.746126346562641984, -4.756430356249999214 ) ) ;
#22555 = CARTESIAN_POINT ( 'NONE',  ( 11.09062500061451573, -3.027376345333610441, -5.243569643749999898 ) ) ;
#22556 = CARTESIAN_POINT ( 'NONE',  ( 5.896875000614518747, 6.054752690667223547, 3.707466751127219781E-16 ) ) ;
#22557 = CARTESIAN_POINT ( 'NONE',  ( 3.759375000614517681, 0.000000000000000000, 5.243569643749999010 ) ) ;
#22558 = ORIENTED_EDGE ( 'NONE', *, *, #6300, .F. ) ;
#22559 = EDGE_CURVE ( 'NONE', #64855, #71132, #48053, .T. ) ;
#22560 = CARTESIAN_POINT ( 'NONE',  ( 27.64687500061452141, -3.027376345333614438, 5.243569643749998122 ) ) ;
#22561 = CARTESIAN_POINT ( 'NONE',  ( 16.86562500061451786, -6.054752690667223547, -1.112240025338166033E-15 ) ) ;
#22562 = CARTESIAN_POINT ( 'NONE',  ( 27.37500000122903288, 2.886751345948126879, 4.999999999999999112 ) ) ;
#22563 = CARTESIAN_POINT ( 'NONE',  ( 28.00312500061451715, 0.000000000000000000, 5.243569643749999010 ) ) ;
#22564 = CARTESIAN_POINT ( 'NONE',  ( 24.45937500061451786, 0.000000000000000000, 5.243569643749999010 ) ) ;
#22565 = CARTESIAN_POINT ( 'NONE',  ( 17.12812500061451715, 4.541064518000418104, 2.621784821874999949 ) ) ;
#22566 = CARTESIAN_POINT ( 'NONE',  ( 2.121784821875001281, 19.10937500061451644, 33.67503911421598417 ) ) ;
#22567 = CARTESIAN_POINT ( 'NONE',  ( 24.51562500061451289, -6.054752690667223547, -1.112240025338166033E-15 ) ) ;
#22568 = CARTESIAN_POINT ( 'NONE',  ( 5.325000001229033941, 2.886751345948126879, 4.999999999999999112 ) ) ;
#22569 = ORIENTED_EDGE ( 'NONE', *, *, #5952, .F. ) ;
#22570 = CARTESIAN_POINT ( 'NONE',  ( 27.75000000000000000, 0.000000000000000000, 4.999999999999998224 ) ) ;
#22571 = CARTESIAN_POINT ( 'NONE',  ( 1.999999999999998668, 14.45000000000000107, -33.46410161513775705 ) ) ;
#22572 = CARTESIAN_POINT ( 'NONE',  ( 2.655984681222220721E-16, 17.36562499938548498, 25.66244784525396483 ) ) ;
#22573 = CARTESIAN_POINT ( 'NONE',  ( 4.734375000614518214, -4.541064518000419881, 2.621784821874995952 ) ) ;
#22574 = CARTESIAN_POINT ( 'NONE',  ( 10.52812500061451750, -4.541064518000419881, 2.621784821874995952 ) ) ;
#22575 = CARTESIAN_POINT ( 'NONE',  ( 5.934375000614517504, 4.541064518000418104, 2.621784821874999949 ) ) ;
#22576 = CARTESIAN_POINT ( 'NONE',  ( 24.37500000122903288, -5.773502691896255534, -1.060575238724906372E-15 ) ) ;
#22577 = CARTESIAN_POINT ( 'NONE',  ( 14.63437500061451679, -4.541064518000419881, 2.621784821874995952 ) ) ;
#22578 = CARTESIAN_POINT ( 'NONE',  ( 28.82812500061451644, 4.541064518000418104, 2.621784821874999949 ) ) ;
#22579 = CARTESIAN_POINT ( 'NONE',  ( 27.26249999999999929, 2.886751345948126879, 4.999999999999999112 ) ) ;
#22580 = CARTESIAN_POINT ( 'NONE',  ( 3.590625000614518836, 6.054752690667223547, 3.707466751127219781E-16 ) ) ;
#22581 = CARTESIAN_POINT ( 'NONE',  ( 12.85312500061451502, -4.541064518000417216, -2.621784821875001281 ) ) ;
#22582 = ORIENTED_EDGE ( 'NONE', *, *, #65502, .F. ) ;
#22583 = CARTESIAN_POINT ( 'NONE',  ( 8.915625000614515017, 3.027376345333613106, -5.243569643749998122 ) ) ;
#22584 = CARTESIAN_POINT ( 'NONE',  ( 5.990625000614517859, -3.027376345333614438, 5.243569643749998122 ) ) ;
#22585 = CARTESIAN_POINT ( 'NONE',  ( 17.74687500061451928, -2.746126346562646425, 4.756430356249996549 ) ) ;
#22586 = DIRECTION ( 'NONE',  ( 0.000000000000000000, 0.000000000000000000, 1.000000000000000000 ) ) ;
#22587 = CARTESIAN_POINT ( 'NONE',  ( 14.62500000000000000, 4.330127018922191873, 2.499999999999999556 ) ) ;
#22588 = CARTESIAN_POINT ( 'NONE',  ( 17.18437500061451573, 4.541064518000418104, 2.621784821874999949 ) ) ;
#22589 = CARTESIAN_POINT ( 'NONE',  ( 12.22500000122903430, -5.773502691896255534, -1.060575238724906372E-15 ) ) ;
#22590 = CARTESIAN_POINT ( 'NONE',  ( 19.04999999999999716, 4.330127018922192761, -2.499999999999997780 ) ) ;
#22591 = CARTESIAN_POINT ( 'NONE',  ( 20.74687500061451573, 6.054752690667223547, 3.707466751127219781E-16 ) ) ;
#22592 = CARTESIAN_POINT ( 'NONE',  ( 2.121784821874999061, 12.90312500061451750, -33.67503911421598417 ) ) ;
#22593 = CARTESIAN_POINT ( 'NONE',  ( -4.000000000000000000, 19.92499999999999716, 30.00000000000000000 ) ) ;
#22594 = CARTESIAN_POINT ( 'NONE',  ( 25.09687500061451360, 4.119189519843966529, -2.378215178124998275 ) ) ;
#22595 = CARTESIAN_POINT ( 'NONE',  ( 30.00000000000000000, 0.000000000000000000, 0.000000000000000000 ) ) ;
#22596 = ADVANCED_FACE ( 'NONE', ( #2610 ), #52855, .F. ) ;
#22597 = CARTESIAN_POINT ( 'NONE',  ( 27.47812500061451502, 4.541064518000418104, 2.621784821874999949 ) ) ;
#22598 = CARTESIAN_POINT ( 'NONE',  ( 29.78437500061451715, 4.541064518000418104, 2.621784821874999949 ) ) ;
#22599 = CARTESIAN_POINT ( 'NONE',  ( 23.25000000000000000, 0.000000000000000000, 4.999999999999998224 ) ) ;
#22600 = CARTESIAN_POINT ( 'NONE',  ( 9.778125000614517504, 6.421520780324663323E-16, -5.243569643749999010 ) ) ;
#22601 = CARTESIAN_POINT ( 'NONE',  ( 27.45937500061451431, 2.746126346562643317, 4.756430356249998326 ) ) ;
#22602 = CARTESIAN_POINT ( 'NONE',  ( 18.72187500061451360, -6.054752690667223547, -1.112240025338166033E-15 ) ) ;
#22603 = CARTESIAN_POINT ( 'NONE',  ( 12.08437500061451608, 5.492252693125287522, 3.363034840372157021E-16 ) ) ;
#22604 = CARTESIAN_POINT ( 'NONE',  ( 4.153125000614515727, 0.000000000000000000, 5.243569643749999010 ) ) ;
#22605 = CARTESIAN_POINT ( 'NONE',  ( 9.946875000614516793, 6.054752690667223547, 3.707466751127219781E-16 ) ) ;
#22606 = ORIENTED_EDGE ( 'NONE', *, *, #54179, .F. ) ;
#22607 = CARTESIAN_POINT ( 'NONE',  ( 21.68437500061451573, 4.541064518000418104, 2.621784821874999949 ) ) ;
#22608 = CARTESIAN_POINT ( 'NONE',  ( 8.006250001229034297, 0.000000000000000000, 4.999999999999998224 ) ) ;
#22609 = CARTESIAN_POINT ( 'NONE',  ( 29.32499999999999929, 6.123233995736764310E-16, -4.999999999999998224 ) ) ;
#22610 = CARTESIAN_POINT ( 'NONE',  ( 5.775000000000002132, -4.330127018922194537, 2.499999999999995559 ) ) ;
#22611 = CARTESIAN_POINT ( 'NONE',  ( 15.75000000122902932, -2.886751345948129988, 4.999999999999997335 ) ) ;
#22612 = FACE_OUTER_BOUND ( 'NONE', #21973, .T. ) ;
#22613 = CARTESIAN_POINT ( 'NONE',  ( 65.00000000000000000, 8.874999999999998224, 1.494782592887675232 ) ) ;
#22614 = AXIS2_PLACEMENT_3D ( 'NONE', #14559, #65539, #48925 ) ;
#22615 = ORIENTED_EDGE ( 'NONE', *, *, #7766, .T. ) ;
#22616 = CARTESIAN_POINT ( 'NONE',  ( 12.63749999999999929, -2.886751345948125991, -5.000000000000000000 ) ) ;
#22617 = CARTESIAN_POINT ( 'NONE',  ( 25.82812500061451644, -4.541064518000419881, 2.621784821874995952 ) ) ;
#22618 = CARTESIAN_POINT ( 'NONE',  ( 17.25000000000000000, 4.330127018922192761, -2.499999999999997780 ) ) ;
#22619 = CARTESIAN_POINT ( 'NONE',  ( 10.16250000122903252, 4.330127018922192761, -2.499999999999997780 ) ) ;
#22620 = CARTESIAN_POINT ( 'NONE',  ( 8.878125000614515372, 6.421520780324663323E-16, -5.243569643749999010 ) ) ;
#22621 = CARTESIAN_POINT ( 'NONE',  ( 8.512499999999999289, -5.773502691896255534, -1.060575238724906372E-15 ) ) ;
#22622 = DIRECTION ( 'NONE',  ( -0.000000000000000000, -1.000000000000000000, -0.000000000000000000 ) ) ;
#22623 = CARTESIAN_POINT ( 'NONE',  ( 4.243569643749999898, 14.68437500061451750, -30.00000000000000000 ) ) ;
#22624 = CARTESIAN_POINT ( 'NONE',  ( 28.95000000122903572, -2.886751345948125991, -5.000000000000000000 ) ) ;
#22625 = CARTESIAN_POINT ( 'NONE',  ( -3.756430356250000102, 13.76562499938548356, 30.00000000000000000 ) ) ;
#22626 = CARTESIAN_POINT ( 'NONE',  ( 8.550000000000002487, -4.330127018922190985, -2.500000000000001332 ) ) ;
#22627 = DIRECTION ( 'NONE',  ( -1.000000000000000000, -0.000000000000000000, -0.000000000000000000 ) ) ;
#22628 = ORIENTED_EDGE ( 'NONE', *, *, #3547, .T. ) ;
#22629 = CARTESIAN_POINT ( 'NONE',  ( 23.57812500061451289, -4.541064518000419881, 2.621784821874995952 ) ) ;
#22630 = CARTESIAN_POINT ( 'NONE',  ( 14.55000000122903181, -2.886751345948125991, -5.000000000000000000 ) ) ;
#22631 = CARTESIAN_POINT ( 'NONE',  ( 28.75312500061451715, 4.541064518000418104, -2.621784821874998173 ) ) ;
#22632 = CARTESIAN_POINT ( 'NONE',  ( 19.08750000122903145, 6.123233995736764310E-16, -4.999999999999998224 ) ) ;
#22633 = CARTESIAN_POINT ( 'NONE',  ( 19.80937500061451573, 4.541064518000418104, -2.621784821874998173 ) ) ;
#22634 = CARTESIAN_POINT ( 'NONE',  ( 17.20312500061451644, 0.000000000000000000, 5.243569643749999010 ) ) ;
#22635 = CARTESIAN_POINT ( 'NONE',  ( 2.121784821874999061, 12.00312500061459531, -33.67503911421598417 ) ) ;
#22636 = CARTESIAN_POINT ( 'NONE',  ( 7.228125000614517681, 4.541064518000418104, 2.621784821874999949 ) ) ;
#22637 = CARTESIAN_POINT ( 'NONE',  ( 28.01250000122903216, -4.330127018922190985, -2.500000000000001332 ) ) ;
#22638 = CARTESIAN_POINT ( 'NONE',  ( 21.08437500061451786, 5.824947211148865298E-16, -4.756430356249998326 ) ) ;
#22639 = CARTESIAN_POINT ( 'NONE',  ( 19.75312500061451360, 4.541064518000418104, -2.621784821874998173 ) ) ;
#22640 = FACE_OUTER_BOUND ( 'NONE', #36245, .T. ) ;
#22641 = CARTESIAN_POINT ( 'NONE',  ( 3.756430356250000102, 19.39062499938548356, 30.00000000000000000 ) ) ;
#22642 = CARTESIAN_POINT ( 'NONE',  ( 13.28437500061451715, -4.541064518000419881, 2.621784821874995952 ) ) ;
#22643 = CARTESIAN_POINT ( 'NONE',  ( 10.88437500061451679, 4.541064518000418104, 2.621784821874999949 ) ) ;
#22644 = CARTESIAN_POINT ( 'NONE',  ( 21.27187500061451786, 3.027376345333611329, 5.243569643749999010 ) ) ;
#22645 = ORIENTED_EDGE ( 'NONE', *, *, #45774, .F. ) ;
#22646 = CARTESIAN_POINT ( 'NONE',  ( 27.26249999999999929, 2.886751345948168623, 4.999999999999926281 ) ) ;
#22647 = CARTESIAN_POINT ( 'NONE',  ( 26.57812500061451644, 4.541064518000418104, 2.621784821874999949 ) ) ;
#22648 = EDGE_CURVE ( 'NONE', #493, #47295, #9808, .T. ) ;
#22649 = CARTESIAN_POINT ( 'NONE',  ( 23.27812500061451573, 6.421520780324663323E-16, -5.243569643749999010 ) ) ;
#22650 = DIRECTION ( 'NONE',  ( -1.000000000000000000, -0.000000000000000000, -0.000000000000000000 ) ) ;
#22651 = CARTESIAN_POINT ( 'NONE',  ( -3.999999999999999556, 17.26249999999999929, 27.69059892324149530 ) ) ;
#22652 = CARTESIAN_POINT ( 'NONE',  ( 3.946875000614517681, -3.027376345333610441, -5.243569643749999898 ) ) ;
#22653 = CARTESIAN_POINT ( 'NONE',  ( 10.98750000122903536, 6.123233995736764310E-16, -4.999999999999998224 ) ) ;
#22654 = CARTESIAN_POINT ( 'NONE',  ( 6.900000001229035007, -2.886751345948125991, -5.000000000000000000 ) ) ;
#22655 = CARTESIAN_POINT ( 'NONE',  ( 28.46250000122903145, -4.330127018922190985, -2.500000000000001332 ) ) ;
#22656 = CARTESIAN_POINT ( 'NONE',  ( 4.000000000000000000, 17.43124999877096570, 27.69059892324149530 ) ) ;
#22657 = CARTESIAN_POINT ( 'NONE',  ( 15.91875000122903216, 2.886751345948129099, -4.999999999999998224 ) ) ;
#22658 = CARTESIAN_POINT ( 'NONE',  ( 11.37187500061451750, 3.027376345333611329, 5.243569643749999010 ) ) ;
#22659 = CARTESIAN_POINT ( 'NONE',  ( 29.49375000122903145, 5.773502691896255534, 3.535250795749688401E-16 ) ) ;
#22660 = CARTESIAN_POINT ( 'NONE',  ( 19.30312500061451786, 4.541064518000418104, -2.621784821874998173 ) ) ;
#22661 = CARTESIAN_POINT ( 'NONE',  ( 13.20937500061451786, 0.000000000000000000, 5.243569643749999010 ) ) ;
#22662 = CARTESIAN_POINT ( 'NONE',  ( 3.815625000614518036, -6.054752690667223547, -1.112240025338166033E-15 ) ) ;
#22663 = CARTESIAN_POINT ( 'NONE',  ( 23.22187500061451715, -6.054752690667223547, -1.112240025338166033E-15 ) ) ;
#22664 = CARTESIAN_POINT ( 'NONE',  ( 10.92187500061451644, 3.027376345333611329, 5.243569643749999010 ) ) ;
#22665 = CARTESIAN_POINT ( 'NONE',  ( 5.315625000614516260, 3.027376345333613106, -5.243569643749998122 ) ) ;
#22666 = LINE ( 'NONE', #39681, #49796 ) ;
#22667 = CARTESIAN_POINT ( 'NONE',  ( 5.437500001229035540, -4.330127018922194537, 2.499999999999995559 ) ) ;
#22668 = CARTESIAN_POINT ( 'NONE',  ( 20.91562500061451502, -6.054752690667223547, -1.112240025338166033E-15 ) ) ;
#22669 = CARTESIAN_POINT ( 'NONE',  ( 8.775000001229033231, 2.886751345948129099, -4.999999999999998224 ) ) ;
#22670 = CARTESIAN_POINT ( 'NONE',  ( 17.99062500061451786, 6.054752690667223547, 3.707466751127219781E-16 ) ) ;
#22671 = CARTESIAN_POINT ( 'NONE',  ( 13.37812500061451715, 6.421520780324663323E-16, -5.243569643749999010 ) ) ;
#22672 = CARTESIAN_POINT ( 'NONE',  ( 26.48437500061451644, 5.824947211148865298E-16, -4.756430356249998326 ) ) ;
#22673 = CARTESIAN_POINT ( 'NONE',  ( 12.33750000000000036, 5.773502691896255534, 3.535250795749688894E-16 ) ) ;
#22674 = CARTESIAN_POINT ( 'NONE',  ( 9.075000001229033941, -5.773502691896255534, -1.060575238724906372E-15 ) ) ;
#22675 = CARTESIAN_POINT ( 'NONE',  ( 4.453125000614517326, 4.541064518000418104, -2.621784821874998173 ) ) ;
#22676 = AXIS2_PLACEMENT_3D ( 'NONE', #52561, #58810, #24834 ) ;
#22677 = CARTESIAN_POINT ( 'NONE',  ( 21.90000000122903145, 5.773502691896255534, 3.535250795749688894E-16 ) ) ;
#22678 = CARTESIAN_POINT ( 'NONE',  ( 26.13749999999999929, -2.886751345948125991, -5.000000000000000000 ) ) ;
#22679 = CARTESIAN_POINT ( 'NONE',  ( 2.121784821875001281, 10.55937500061451750, -26.32496088578401938 ) ) ;
#22680 = CARTESIAN_POINT ( 'NONE',  ( 21.30000000000000071, 4.330127018922192761, -2.499999999999997780 ) ) ;
#22681 = DIRECTION ( 'NONE',  ( 0.000000000000000000, 0.000000000000000000, -1.000000000000000000 ) ) ;
#22682 = CARTESIAN_POINT ( 'NONE',  ( 4.000000000000000000, 14.75000000000000178, 30.00000000000000000 ) ) ;
#22683 = CARTESIAN_POINT ( 'NONE',  ( 21.83437500061451786, -4.541064518000419881, 2.621784821874995952 ) ) ;
#22684 = CARTESIAN_POINT ( 'NONE',  ( 3.999999999999999112, 18.53750000122903430, 30.00000000000000000 ) ) ;
#22685 = CARTESIAN_POINT ( 'NONE',  ( 16.26562500061451289, 3.027376345333611329, 5.243569643749999010 ) ) ;
#22686 = CARTESIAN_POINT ( 'NONE',  ( 10.78125000122903288, -4.330127018922194537, 2.499999999999995559 ) ) ;
#22687 = CARTESIAN_POINT ( 'NONE',  ( -4.000000000000000000, 20.76874999877096428, 30.00000000000000000 ) ) ;
#22688 = CARTESIAN_POINT ( 'NONE',  ( 0.000000000000000000, 27.50000000000000000, 30.00000000000000000 ) ) ;
#22689 = CARTESIAN_POINT ( 'NONE',  ( 25.28437500061451715, 4.541064518000418104, 2.621784821874999949 ) ) ;
#22690 = CARTESIAN_POINT ( 'NONE',  ( 20.97187500061451715, 5.824947211148865298E-16, -4.756430356249998326 ) ) ;
#22691 = CARTESIAN_POINT ( 'NONE',  ( 11.42812500061451608, -4.541064518000419881, 2.621784821874995952 ) ) ;
#22692 = CARTESIAN_POINT ( 'NONE',  ( 9.946875000614516793, 6.054752690667223547, 3.707466751127219781E-16 ) ) ;
#22693 = ORIENTED_EDGE ( 'NONE', *, *, #72495, .T. ) ;
#22694 = CARTESIAN_POINT ( 'NONE',  ( 29.24062500061451431, 6.054752690667223547, 3.707466751127219781E-16 ) ) ;
#22695 = CARTESIAN_POINT ( 'NONE',  ( 21.85312500061451502, -4.541064518000417216, -2.621784821875001281 ) ) ;
#22696 = CARTESIAN_POINT ( 'NONE',  ( 0.000000000000000000, 20.00000000000000000, 30.00000000000000000 ) ) ;
#22697 = CARTESIAN_POINT ( 'NONE',  ( -3.999999999999997335, 12.95000000122903216, 32.30940107675850470 ) ) ;
#22698 = CARTESIAN_POINT ( 'NONE',  ( 12.90000000000000213, 0.000000000000000000, 4.999999999999998224 ) ) ;
#22699 = CARTESIAN_POINT ( 'NONE',  ( 22.46250000122903501, 0.000000000000000000, 4.999999999999998224 ) ) ;
#22700 = CARTESIAN_POINT ( 'NONE',  ( 16.49062500061451786, -3.027376345333610441, -5.243569643749999898 ) ) ;
#22701 = CARTESIAN_POINT ( 'NONE',  ( 12.49687500061451573, 4.119189519843966529, -2.378215178124998275 ) ) ;
#22702 = EDGE_LOOP ( 'NONE', ( #16159, #63518, #52925 ) ) ;
#22703 = CARTESIAN_POINT ( 'NONE',  ( 21.03750000000000142, -2.886751345948129988, 4.999999999999997335 ) ) ;
#22704 = CARTESIAN_POINT ( 'NONE',  ( 24.14999999999999858, 0.000000000000000000, 4.999999999999998224 ) ) ;
#22705 = CARTESIAN_POINT ( 'NONE',  ( 21.19687500061451502, 6.054752690667223547, 3.707466751127219781E-16 ) ) ;
#22706 = CARTESIAN_POINT ( 'NONE',  ( 25.26562500061451289, 3.027376345333611329, 5.243569643749999010 ) ) ;
#22707 = ORIENTED_EDGE ( 'NONE', *, *, #22854, .T. ) ;
#22708 = EDGE_CURVE ( 'NONE', #48448, #33629, #29952, .T. ) ;
#22709 = LINE ( 'NONE', #6093, #40729 ) ;
#22710 = CARTESIAN_POINT ( 'NONE',  ( 8.653125000614515727, 0.000000000000000000, 5.243569643749999010 ) ) ;
#22711 = CARTESIAN_POINT ( 'NONE',  ( 15.78749999999999964, -2.886751345948125991, -5.000000000000000000 ) ) ;
#22712 = CARTESIAN_POINT ( 'NONE',  ( -3.000416591977282496E-16, 17.44062500061451360, 25.09994784771203058 ) ) ;
#22713 = CARTESIAN_POINT ( 'NONE',  ( 4.134375000614517681, 4.541064518000418104, 2.621784821874999949 ) ) ;
#22714 = CARTESIAN_POINT ( 'NONE',  ( 26.52187500061451431, 3.027376345333613106, -5.243569643749998122 ) ) ;
#22715 = ORIENTED_EDGE ( 'NONE', *, *, #49507, .T. ) ;
#22716 = CARTESIAN_POINT ( 'NONE',  ( 23.39062500061451289, 6.054752690667223547, 3.707466751127219781E-16 ) ) ;
#22717 = CARTESIAN_POINT ( 'NONE',  ( 25.20937500061451431, 4.541064518000418104, -2.621784821874998173 ) ) ;
#22718 = CARTESIAN_POINT ( 'NONE',  ( -2.121784821874996840, 19.42812500061459247, -26.32496088578401583 ) ) ;
#22719 = CARTESIAN_POINT ( 'NONE',  ( 11.25000000000000000, -4.330127018922190985, -2.500000000000001332 ) ) ;
#22720 = CARTESIAN_POINT ( 'NONE',  ( 8.728125000614518569, -4.541064518000419881, 2.621784821874995952 ) ) ;
#22721 = DIRECTION ( 'NONE',  ( -0.000000000000000000, -1.000000000000000000, -0.000000000000000000 ) ) ;
#22722 = CARTESIAN_POINT ( 'NONE',  ( 13.35000000000000142, 0.000000000000000000, 4.999999999999998224 ) ) ;
#22723 = CARTESIAN_POINT ( 'NONE',  ( 27.40312500061451573, 4.541064518000418104, -2.621784821874998173 ) ) ;
#22724 = CARTESIAN_POINT ( 'NONE',  ( -3.999999999999997335, 18.23750000000000071, 32.30940107675850470 ) ) ;
#22725 = CARTESIAN_POINT ( 'NONE',  ( 11.85937500061451644, 0.000000000000000000, 4.756430356249998326 ) ) ;
#22726 = CARTESIAN_POINT ( 'NONE',  ( 3.328125000614516438, -4.541064518000419881, 2.621784821874995952 ) ) ;
#22727 = CARTESIAN_POINT ( 'NONE',  ( 18.79687500061451644, -3.027376345333610441, -5.243569643749999898 ) ) ;
#22728 = CARTESIAN_POINT ( 'NONE',  ( -2.121784821874996840, 14.53437500061451715, 33.67503911421598417 ) ) ;
#22729 = CARTESIAN_POINT ( 'NONE',  ( 19.95937500061451786, 0.000000000000000000, 5.243569643749999010 ) ) ;
#22730 = CARTESIAN_POINT ( 'NONE',  ( 29.33437500061451431, 4.541064518000418104, 2.621784821874999949 ) ) ;
#22731 = CARTESIAN_POINT ( 'NONE',  ( -4.243569643749999898, 19.82187500061451857, 27.54997392385601529 ) ) ;
#22732 = CARTESIAN_POINT ( 'NONE',  ( 10.64062500061451644, -3.027376345333610441, -5.243569643749999898 ) ) ;
#22733 = CARTESIAN_POINT ( 'NONE',  ( 2.662500001229036073, 0.000000000000000000, 4.999999999999998224 ) ) ;
#22734 = EDGE_CURVE ( 'NONE', #19796, #34387, #5515, .T. ) ;
#22735 = AXIS2_PLACEMENT_3D ( 'NONE', #65028, #54681, #14419 ) ;
#22736 = CARTESIAN_POINT ( 'NONE',  ( 5.821875000614519458, 3.027376345333613106, -5.243569643749998122 ) ) ;
#22737 = DIRECTION ( 'NONE',  ( -0.000000000000000000, -1.000000000000000000, -0.000000000000000000 ) ) ;
#22738 = CARTESIAN_POINT ( 'NONE',  ( 7.753125000614518036, 0.000000000000000000, 5.243569643749999010 ) ) ;
#22739 = CARTESIAN_POINT ( 'NONE',  ( 13.02187500061451608, 3.027376345333613106, -5.243569643749998122 ) ) ;
#22740 =( LENGTH_UNIT ( ) NAMED_UNIT ( * ) SI_UNIT ( .MILLI., .METRE. ) );
#22741 = CARTESIAN_POINT ( 'NONE',  ( 17.96250000122903501, 0.000000000000000000, 4.999999999999998224 ) ) ;
#22742 = CARTESIAN_POINT ( 'NONE',  ( 8.371875000614515727, -6.054752690667223547, -1.112240025338166033E-15 ) ) ;
#22743 = CARTESIAN_POINT ( 'NONE',  ( 9.965625000614517504, 3.027376345333611329, 5.243569643749999010 ) ) ;
#22744 = LINE ( 'NONE', #6489, #39876 ) ;
#22745 = CARTESIAN_POINT ( 'NONE',  ( 22.70625000122903003, 4.330127018922192761, -2.499999999999997780 ) ) ;
#22746 = CARTESIAN_POINT ( 'NONE',  ( 19.73437500061451644, 6.421520780324663323E-16, -5.243569643749999010 ) ) ;
#22747 = CARTESIAN_POINT ( 'NONE',  ( 9.075000001229033941, -5.773502691896255534, -1.060575238724906372E-15 ) ) ;
#22748 = CARTESIAN_POINT ( 'NONE',  ( 26.31562500061451715, -6.054752690667223547, -1.112240025338166033E-15 ) ) ;
#22750 = CARTESIAN_POINT ( 'NONE',  ( 13.00312500061451537, 4.541064518000418104, -2.621784821874998173 ) ) ;
#22749 =( BOUNDED_CURVE ( )  B_SPLINE_CURVE ( 2, ( #30341, #69148, #18138, #18507, #47327, #12253, #45884 ),
 .UNSPECIFIED., .F., .F. ) 
 B_SPLINE_CURVE_WITH_KNOTS ( ( 3, 2, 2, 3 ),
 ( 0.1400000000000000133, 0.1433333333333333404, 0.1466666666666666674, 0.1499999999999999944 ),
 .UNSPECIFIED. ) 
 CURVE ( )  GEOMETRIC_REPRESENTATION_ITEM ( )  RATIONAL_B_SPLINE_CURVE ( ( 1.000000000000000000, 0.8660254037844387076, 1.000000000000000000, 0.8660254037844387076, 1.000000000000000000, 0.8660254037844387076, 1.000000000000000000 ) ) 
 REPRESENTATION_ITEM ( '' )  );
#22751 = CARTESIAN_POINT ( 'NONE',  ( 28.73437500061451644, 6.421520780324663323E-16, -5.243569643749999010 ) ) ;
#22752 = CARTESIAN_POINT ( 'NONE',  ( 25.48125000122903216, 4.330127018922191873, 2.499999999999999556 ) ) ;
#22753 = CARTESIAN_POINT ( 'NONE',  ( 13.95000000122903572, -2.886751345948129988, 4.999999999999997335 ) ) ;
#22754 = CARTESIAN_POINT ( 'NONE',  ( 28.15312500061451573, -4.541064518000417216, -2.621784821875001281 ) ) ;
#22755 = CARTESIAN_POINT ( 'NONE',  ( 2.121784821875001281, 15.90312500061451573, -26.32496088578401938 ) ) ;
#22756 = CARTESIAN_POINT ( 'NONE',  ( 16.01250000122903216, 4.330127018922192761, -2.499999999999997780 ) ) ;
#22757 = CARTESIAN_POINT ( 'NONE',  ( 13.27500000000000213, 4.330127018922191873, 2.499999999999999556 ) ) ;
#22758 = CARTESIAN_POINT ( 'NONE',  ( 23.39062500061451289, 6.054752690667223547, 3.707466751127219781E-16 ) ) ;
#22759 = CARTESIAN_POINT ( 'NONE',  ( 8.821875000614518569, -6.054752690667223547, -1.112240025338166033E-15 ) ) ;
#22760 = CARTESIAN_POINT ( 'NONE',  ( 7.725000001229034297, -5.773502691896255534, -1.060575238724906372E-15 ) ) ;
#22761 = CARTESIAN_POINT ( 'NONE',  ( 16.76250000122903216, -4.330127018922190985, -2.500000000000001332 ) ) ;
#22762 = CARTESIAN_POINT ( 'NONE',  ( 12.10312500061451857, 4.541064518000418104, -2.621784821874998173 ) ) ;
#22763 = CARTESIAN_POINT ( 'NONE',  ( 15.59062500061451573, -3.027376345333610441, -5.243569643749999898 ) ) ;
#22764 =( BOUNDED_CURVE ( )  B_SPLINE_CURVE ( 3, ( #1063, #41658, #63095, #23930 ),
 .UNSPECIFIED., .F., .F. ) 
 B_SPLINE_CURVE_WITH_KNOTS ( ( 4, 4 ),
 ( 0.000000000000000000, 1.570796326794896780 ),
 .UNSPECIFIED. ) 
 CURVE ( )  GEOMETRIC_REPRESENTATION_ITEM ( )  RATIONAL_B_SPLINE_CURVE ( ( 1.000000000000000000, 0.8047378541243649375, 0.8047378541243649375, 1.000000000000000000 ) ) 
 REPRESENTATION_ITEM ( '' )  );
#22765 = CARTESIAN_POINT ( 'NONE',  ( 27.15000000122902790, -2.886751345948125991, -5.000000000000000000 ) ) ;
#22766 = CARTESIAN_POINT ( 'NONE',  ( 21.71249999999999858, 2.886751345948129099, -4.999999999999998224 ) ) ;
#22767 = CARTESIAN_POINT ( 'NONE',  ( 24.08437500061451786, -4.541064518000419881, 2.621784821874995952 ) ) ;
#22768 = CARTESIAN_POINT ( 'NONE',  ( -5.810221930991193690E-16, 12.35000000122903430, 26.00000000000000355 ) ) ;
#22769 = CARTESIAN_POINT ( 'NONE',  ( 10.12500000122903465, 2.886751345948129099, -4.999999999999998224 ) ) ;
#22770 = CARTESIAN_POINT ( 'NONE',  ( 27.72187500061451715, -6.054752690667223547, -1.112240025338166033E-15 ) ) ;
#22771 = CARTESIAN_POINT ( 'NONE',  ( 5.071875000614519458, 3.027376345333611329, 5.243569643749999010 ) ) ;
#22772 = CARTESIAN_POINT ( 'NONE',  ( 23.24062500061451786, -3.027376345333610441, -5.243569643749999898 ) ) ;
#22773 =( BOUNDED_CURVE ( )  B_SPLINE_CURVE ( 2, ( #34299, #57562, #46490, #12506, #68666, #68305, #69029 ),
 .UNSPECIFIED., .F., .F. ) 
 B_SPLINE_CURVE_WITH_KNOTS ( ( 3, 2, 2, 3 ),
 ( 0.8583333333333332815, 0.8611111111111111605, 0.8638888888888889284, 0.8666666666666666963 ),
 .UNSPECIFIED. ) 
 CURVE ( )  GEOMETRIC_REPRESENTATION_ITEM ( )  RATIONAL_B_SPLINE_CURVE ( ( 1.000000000000000000, 0.8660254037844387076, 1.000000000000000000, 0.8660254037844387076, 1.000000000000000000, 0.8660254037844387076, 1.000000000000000000 ) ) 
 REPRESENTATION_ITEM ( '' )  );
#22774 = CARTESIAN_POINT ( 'NONE',  ( -1.878215178124999163, 14.70312499938548356, 26.74683588394047007 ) ) ;
#22775 = CARTESIAN_POINT ( 'NONE',  ( 6.937499999999999112, 5.773502691896255534, 3.535250795749688401E-16 ) ) ;
#22776 = CARTESIAN_POINT ( 'NONE',  ( 9.646875000614516082, -3.027376345333614438, 5.243569643749998122 ) ) ;
#22777 = CARTESIAN_POINT ( 'NONE',  ( 12.95625000122903359, 0.000000000000000000, 4.999999999999998224 ) ) ;
#22778 = CARTESIAN_POINT ( 'NONE',  ( 4.059375000614519280, 4.541064518000418104, -2.621784821874998173 ) ) ;
#22779 = CARTESIAN_POINT ( 'NONE',  ( 6.046875000614519102, -3.027376345333614438, 5.243569643749998122 ) ) ;
#22780 = DIRECTION ( 'NONE',  ( -0.000000000000000000, -1.000000000000000000, -0.000000000000000000 ) ) ;
#22781 = CARTESIAN_POINT ( 'NONE',  ( 26.10937500061451644, 4.541064518000418104, -2.621784821874998173 ) ) ;
#22782 = CARTESIAN_POINT ( 'NONE',  ( 4.243569643749999898, 10.57812500061459637, 30.00000000000000000 ) ) ;
#22783 = CARTESIAN_POINT ( 'NONE',  ( 20.13749999999999929, -2.886751345948129988, 4.999999999999997335 ) ) ;
#22784 = VERTEX_POINT ( 'NONE', #41767 ) ;
#22785 = CARTESIAN_POINT ( 'NONE',  ( 27.89999999999999858, -4.330127018922190985, -2.500000000000001332 ) ) ;
#22786 = CARTESIAN_POINT ( 'NONE',  ( 28.62187500061451573, -6.054752690667223547, -1.112240025338166033E-15 ) ) ;
#22787 = VERTEX_POINT ( 'NONE', #21416 ) ;
#22788 = CARTESIAN_POINT ( 'NONE',  ( 15.85312500061451857, 0.000000000000000000, 5.243569643749999010 ) ) ;
#22789 = CARTESIAN_POINT ( 'NONE',  ( 7.415625000614516793, -6.054752690667223547, -1.112240025338166033E-15 ) ) ;
#22790 = CARTESIAN_POINT ( 'NONE',  ( 18.79687500061451289, 4.119189519843966529, -2.378215178124998275 ) ) ;
#22791 = CARTESIAN_POINT ( 'NONE',  ( 5.559375000614517504, 0.000000000000000000, 5.243569643749999010 ) ) ;
#22792 = CARTESIAN_POINT ( 'NONE',  ( 18.71250000122903145, 4.330127018922192761, -2.499999999999997780 ) ) ;
#22793 = CARTESIAN_POINT ( 'NONE',  ( 23.06250000000000355, 2.886751345948129099, -4.999999999999998224 ) ) ;
#22794 = CARTESIAN_POINT ( 'NONE',  ( -5.810221930991193690E-16, 14.03750000000000142, -34.00000000000000000 ) ) ;
#22795 = CARTESIAN_POINT ( 'NONE',  ( 6.309375000614517504, 4.541064518000418104, -2.621784821874998173 ) ) ;
#22796 = CARTESIAN_POINT ( 'NONE',  ( 11.82187500061451679, 3.027376345333611329, 5.243569643749999010 ) ) ;
#22797 = CARTESIAN_POINT ( 'NONE',  ( 21.45937500061451786, -4.541064518000417216, -2.621784821875001281 ) ) ;
#22798 = EDGE_CURVE ( 'NONE', #55986, #39550, #40043, .T. ) ;
#22799 = CARTESIAN_POINT ( 'NONE',  ( 1.592000809091587073E-14, 16.28750000000000142, 26.00000000000000000 ) ) ;
#22800 = VERTEX_POINT ( 'NONE', #60206 ) ;
#22801 = CARTESIAN_POINT ( 'NONE',  ( 5.034375000614519813, 4.541064518000418104, 2.621784821874999949 ) ) ;
#22802 = CARTESIAN_POINT ( 'NONE',  ( 6.496875000614517504, -3.027376345333614438, 5.243569643749998122 ) ) ;
#22803 = CARTESIAN_POINT ( 'NONE',  ( 19.53749999999999432, 5.773502691896255534, 3.535250795749688894E-16 ) ) ;
#22804 = CARTESIAN_POINT ( 'NONE',  ( 15.36562500061451608, 3.027376345333611329, 5.243569643749999010 ) ) ;
#22805 = CARTESIAN_POINT ( 'NONE',  ( 4.000000000000000000, 18.34999999999999787, 30.00000000000000000 ) ) ;
#22806 = CARTESIAN_POINT ( 'NONE',  ( 18.18750000000000355, 5.773502691896255534, 3.535250795749688401E-16 ) ) ;
#22807 = CARTESIAN_POINT ( 'NONE',  ( 21.19687500061451502, 5.492252693125287522, 3.363034840372157021E-16 ) ) ;
#22808 = CARTESIAN_POINT ( 'NONE',  ( 10.71562500061451928, 3.027376345333613106, -5.243569643749998122 ) ) ;
#22809 = CARTESIAN_POINT ( 'NONE',  ( 26.33437500061451431, -4.541064518000419881, 2.621784821874995952 ) ) ;
#22810 = CARTESIAN_POINT ( 'NONE',  ( 28.48125000122902861, 6.123233995736764310E-16, -4.999999999999998224 ) ) ;
#22811 = CARTESIAN_POINT ( 'NONE',  ( 27.83437500061451786, 6.421520780324663323E-16, -5.243569643749999010 ) ) ;
#22812 = CARTESIAN_POINT ( 'NONE',  ( 10.53750000000000320, 5.773502691896255534, 3.535250795749688894E-16 ) ) ;
#22813 = CARTESIAN_POINT ( 'NONE',  ( -3.999999999999999112, 15.16250000122903252, 30.00000000000000000 ) ) ;
#22814 = CARTESIAN_POINT ( 'NONE',  ( 8.437500001229034652, 4.330127018922191873, 2.499999999999999556 ) ) ;
#22815 = CARTESIAN_POINT ( 'NONE',  ( 20.22187500061451715, 3.027376345333613106, -5.243569643749998122 ) ) ;
#22816 = CARTESIAN_POINT ( 'NONE',  ( 13.54687500061451999, 6.054752690667223547, 3.707466751127219781E-16 ) ) ;
#22817 = CARTESIAN_POINT ( 'NONE',  ( 5.857864376269048101, 9.999999999999992895, 5.857864376269048101 ) ) ;
#22818 = ORIENTED_EDGE ( 'NONE', *, *, #59834, .T. ) ;
#22819 = CARTESIAN_POINT ( 'NONE',  ( 13.86562500061451431, 3.027376345333613106, -5.243569643749998122 ) ) ;
#22820 = CARTESIAN_POINT ( 'NONE',  ( 27.37500000122903288, 2.886751345948126879, 4.999999999999999112 ) ) ;
#22821 = CARTESIAN_POINT ( 'NONE',  ( 14.85937500061451644, 4.541064518000418104, -2.621784821874998173 ) ) ;
#22822 = CARTESIAN_POINT ( 'NONE',  ( 3.103125000614517237, 4.541064518000418104, -2.621784821874998173 ) ) ;
#22823 = CARTESIAN_POINT ( 'NONE',  ( 17.39062500061451644, -3.027376345333610441, -5.243569643749999898 ) ) ;
#22824 = CYLINDRICAL_SURFACE ( 'NONE', #22085, 4.000000000000000000 ) ;
#22825 = CARTESIAN_POINT ( 'NONE',  ( 25.73437500061451644, 4.541064518000418104, 2.621784821874999949 ) ) ;
#22826 = CARTESIAN_POINT ( 'NONE',  ( -2.121784821874999949, 10.72812500061451679, 26.32496088578401938 ) ) ;
#22827 = CARTESIAN_POINT ( 'NONE',  ( 15.60937500061451644, -4.541064518000417216, -2.621784821875001281 ) ) ;
#22828 = CARTESIAN_POINT ( 'NONE',  ( 14.47500000122903430, -5.773502691896255534, -1.060575238724906372E-15 ) ) ;
#22829 = CYLINDRICAL_SURFACE ( 'NONE', #20963, 4.999999999999998224 ) ;
#22830 = CARTESIAN_POINT ( 'NONE',  ( -2.121784821874999949, 16.63437500061451857, -33.67503911421598417 ) ) ;
#22831 = CARTESIAN_POINT ( 'NONE',  ( 19.28437500061451360, 6.421520780324663323E-16, -5.243569643749999010 ) ) ;
#22832 = CARTESIAN_POINT ( 'NONE',  ( 20.21250000122903145, 0.000000000000000000, 4.999999999999998224 ) ) ;
#22833 = CARTESIAN_POINT ( 'NONE',  ( 15.83437500061451608, 4.541064518000418104, 2.621784821874999949 ) ) ;
#22834 = CARTESIAN_POINT ( 'NONE',  ( -4.243569643749997233, 11.34687500061451892, 32.45002607614398471 ) ) ;
#22835 = CARTESIAN_POINT ( 'NONE',  ( 23.25000000122903288, 5.773502691896255534, 3.535250795749688894E-16 ) ) ;
#22836 = CARTESIAN_POINT ( 'NONE',  ( 14.54062500061451679, -3.027376345333614438, 5.243569643749998122 ) ) ;
#22837 = CARTESIAN_POINT ( 'NONE',  ( 29.50312500061451360, -4.541064518000417216, -2.621784821875001281 ) ) ;
#22838 = VERTEX_POINT ( 'NONE', #43973 ) ;
#22839 = ORIENTED_EDGE ( 'NONE', *, *, #35798, .F. ) ;
#22840 = CARTESIAN_POINT ( 'NONE',  ( 21.37499999999999645, 4.330127018922191873, 2.499999999999999556 ) ) ;
#22841 = CARTESIAN_POINT ( 'NONE',  ( -1.999999999999997113, 17.93750000122903288, 33.46410161513775705 ) ) ;
#22842 = CARTESIAN_POINT ( 'NONE',  ( 3.861486210907942418, 3.177525289277529197, 31.07754487038764424 ) ) ;
#22843 = CARTESIAN_POINT ( 'NONE',  ( 14.58750000122903323, 6.123233995736764310E-16, -4.999999999999998224 ) ) ;
#22844 = CARTESIAN_POINT ( 'NONE',  ( 19.49062500061451431, -3.027376345333614438, 5.243569643749998122 ) ) ;
#22845 = CARTESIAN_POINT ( 'NONE',  ( 22.82812500061451644, 6.421520780324663323E-16, -5.243569643749999010 ) ) ;
#22846 = CARTESIAN_POINT ( 'NONE',  ( 6.628125000614517148, 6.421520780324663323E-16, -5.243569643749999010 ) ) ;
#22847 = CARTESIAN_POINT ( 'NONE',  ( 29.02499999999999858, 4.330127018922191873, 2.499999999999999556 ) ) ;
#22848 = CARTESIAN_POINT ( 'NONE',  ( 9.496875000614517504, 5.492252693125287522, 3.363034840372157021E-16 ) ) ;
#22849 = CARTESIAN_POINT ( 'NONE',  ( 29.78437500061451715, 4.541064518000418104, 2.621784821874999949 ) ) ;
#22850 = CARTESIAN_POINT ( 'NONE',  ( -2.000000000000000000, 12.38750000122903394, -33.46410161513775705 ) ) ;
#22851 = CARTESIAN_POINT ( 'NONE',  ( -4.243569643749997233, 17.64687500061452141, -27.54997392385601174 ) ) ;
#22852 = CARTESIAN_POINT ( 'NONE',  ( 7.012500001229035718, 4.330127018922192761, -2.499999999999997780 ) ) ;
#22853 = CARTESIAN_POINT ( 'NONE',  ( 7.837499999999999467, 5.773502691896255534, 3.535250795749688894E-16 ) ) ;
#22854 = EDGE_CURVE ( 'NONE', #1482, #4916, #66492, .T. ) ;
#22855 = CARTESIAN_POINT ( 'NONE',  ( 3.450000001229036162, 5.773502691896255534, 3.535250795749688894E-16 ) ) ;
#22856 = CARTESIAN_POINT ( 'NONE',  ( 11.29687500061451644, 6.054752690667223547, 3.707466751127219781E-16 ) ) ;
#22857 = CARTESIAN_POINT ( 'NONE',  ( 12.44999999999999929, 0.000000000000000000, 4.999999999999998224 ) ) ;
#22858 = CARTESIAN_POINT ( 'NONE',  ( 4.096875000614518925, 6.054752690667223547, 3.707466751127219781E-16 ) ) ;
#22859 = CARTESIAN_POINT ( 'NONE',  ( 12.82500000122903394, 2.886751345948129099, -4.999999999999997335 ) ) ;
#22860 = CARTESIAN_POINT ( 'NONE',  ( 1.071796769724490783, 19.34509619066136565, 34.00000000000000000 ) ) ;
#22861 = CARTESIAN_POINT ( 'NONE',  ( 9.946875000614516793, 6.054752690667223547, 3.707466751127219781E-16 ) ) ;
#22862 = CARTESIAN_POINT ( 'NONE',  ( 14.22187500061451537, -6.054752690667223547, -1.112240025338166033E-15 ) ) ;
#22863 = CARTESIAN_POINT ( 'NONE',  ( 4.517629703274214314, -3.565318894049279930, 3.824686530321367517 ) ) ;
#22864 = CARTESIAN_POINT ( 'NONE',  ( 2.121784821875001281, 16.80312500061459247, 33.67503911421598417 ) ) ;
#22865 = CARTESIAN_POINT ( 'NONE',  ( 21.04687500061451644, -3.027376345333610441, -5.243569643749999898 ) ) ;
#22866 = CARTESIAN_POINT ( 'NONE',  ( 26.36250000122903003, 4.330127018922192761, -2.499999999999997780 ) ) ;
#22867 = CARTESIAN_POINT ( 'NONE',  ( 18.15937500061451715, -5.492252693125287522, -1.008910452111647106E-15 ) ) ;
#22868 = CARTESIAN_POINT ( 'NONE',  ( 23.54062500061451146, -3.027376345333614438, 5.243569643749998122 ) ) ;
#22869 = CARTESIAN_POINT ( 'NONE',  ( 16.41562500061451857, -6.054752690667223547, -1.112240025338166033E-15 ) ) ;
#22870 = CARTESIAN_POINT ( 'NONE',  ( 25.77187500061451431, -4.119189519843968306, 2.378215178124996054 ) ) ;
#22871 = CARTESIAN_POINT ( 'NONE',  ( 13.02187500061451608, 3.027376345333613106, -5.243569643749998122 ) ) ;
#22872 = CARTESIAN_POINT ( 'NONE',  ( 28.31250000000000000, -5.773502691896255534, -1.060575238724906372E-15 ) ) ;
#22873 = CARTESIAN_POINT ( 'NONE',  ( 25.38750000122903216, 6.123233995736764310E-16, -4.999999999999998224 ) ) ;
#22874 = VECTOR ( 'NONE', #13580, 1000.000000000000227 ) ;
#22875 = CARTESIAN_POINT ( 'NONE',  ( 4.134375000614517681, 4.541064518000418104, 2.621784821874999949 ) ) ;
#22876 = CARTESIAN_POINT ( 'NONE',  ( 13.99687500061451928, 6.054752690667223547, 3.707466751127219781E-16 ) ) ;
#22877 = CARTESIAN_POINT ( 'NONE',  ( 29.33437500061451431, 4.541064518000418104, 2.621784821874999949 ) ) ;
#22878 = CARTESIAN_POINT ( 'NONE',  ( 0.000000000000000000, 27.50000000000000000, 30.00000000000000000 ) ) ;
#22879 = DIRECTION ( 'NONE',  ( -1.000000000000000000, -0.000000000000000000, -0.000000000000000000 ) ) ;
#22880 = CARTESIAN_POINT ( 'NONE',  ( 23.48437500061451644, 4.541064518000418104, 2.621784821874999949 ) ) ;
#22881 = CARTESIAN_POINT ( 'NONE',  ( 13.65937500061451715, 0.000000000000000000, 5.243569643749999010 ) ) ;
#22882 = CARTESIAN_POINT ( 'NONE',  ( 1.878215178124997609, 16.72812499938548214, 33.25316411605952993 ) ) ;
#22883 = CARTESIAN_POINT ( 'NONE',  ( 25.57499999999999929, -4.330127018922194537, 2.499999999999995559 ) ) ;
#22884 = CARTESIAN_POINT ( 'NONE',  ( 3.750000001229034652, -2.886751345948125991, -5.000000000000000000 ) ) ;
#22885 = CARTESIAN_POINT ( 'NONE',  ( 28.73437500061451644, 5.824947211148865298E-16, -4.756430356249998326 ) ) ;
#22886 = CARTESIAN_POINT ( 'NONE',  ( 16.22812500061451857, 4.541064518000418104, 2.621784821874999949 ) ) ;
#22887 = CARTESIAN_POINT ( 'NONE',  ( 7.762500000000001954, 2.886751345948129099, -4.999999999999998224 ) ) ;
#22888 = CARTESIAN_POINT ( 'NONE',  ( 13.50000000122903288, -2.886751345948130876, 4.999999999999996447 ) ) ;
#22889 = CARTESIAN_POINT ( 'NONE',  ( 16.72500000000000142, 6.123233995736764310E-16, -4.999999999999998224 ) ) ;
#22890 = CARTESIAN_POINT ( 'NONE',  ( -2.121784821874999949, 13.87812500061451715, 26.32496088578401938 ) ) ;
#22891 = LINE ( 'NONE', #6652, #12453 ) ;
#22892 = CARTESIAN_POINT ( 'NONE',  ( 21.67500000122903359, -5.773502691896255534, -1.060575238724906372E-15 ) ) ;
#22893 = CARTESIAN_POINT ( 'NONE',  ( 2.695452854360187445, 9.631537354464013490, 24.63599347216290170 ) ) ;
#22894 = CARTESIAN_POINT ( 'NONE',  ( 26.14687500061451431, 6.054752690667223547, 3.707466751127219781E-16 ) ) ;
#22895 = EDGE_LOOP ( 'NONE', ( #45166, #71877, #31334, #60784 ) ) ;
#22896 = CARTESIAN_POINT ( 'NONE',  ( 21.21562500061451573, 3.027376345333611329, 5.243569643749999010 ) ) ;
#22897 = CARTESIAN_POINT ( 'NONE',  ( 21.30937500061451573, 0.000000000000000000, 5.243569643749999010 ) ) ;
#22898 = CARTESIAN_POINT ( 'NONE',  ( 7.124999999999999112, -4.330127018922194537, 2.499999999999995559 ) ) ;
#22899 = CARTESIAN_POINT ( 'NONE',  ( 10.26562500061451644, 3.027376345333613106, -5.243569643749998122 ) ) ;
#22900 = CARTESIAN_POINT ( 'NONE',  ( 23.35312500061451857, 4.541064518000418104, -2.621784821874998173 ) ) ;
#22901 = CARTESIAN_POINT ( 'NONE',  ( 12.04687500061451821, -3.027376345333610441, -5.243569643749999898 ) ) ;
#22902 = CARTESIAN_POINT ( 'NONE',  ( 17.14687500061451786, 6.054752690667223547, 3.707466751127219781E-16 ) ) ;
#22903 = CARTESIAN_POINT ( 'NONE',  ( 4.465851277537014496, 2.248593419656078840, -4.736966354317482697 ) ) ;
#22904 = CARTESIAN_POINT ( 'NONE',  ( 9.001249775931846008E-16, 17.66562500061451502, 34.90005215228797653 ) ) ;
#22905 = ADVANCED_FACE ( 'NONE', ( #48419 ), #38047, .F. ) ;
#22906 = CARTESIAN_POINT ( 'NONE',  ( 21.48750000122903003, 4.330127018922191873, 2.499999999999999556 ) ) ;
#22907 = CARTESIAN_POINT ( 'NONE',  ( 13.62187500061451750, 2.746126346562643317, 4.756430356249998326 ) ) ;
#22908 = CARTESIAN_POINT ( 'NONE',  ( 11.05312500061451608, -4.541064518000417216, -2.621784821875001281 ) ) ;
#22909 = CARTESIAN_POINT ( 'NONE',  ( 4.921875000614518214, 3.027376345333613106, -5.243569643749998122 ) ) ;
#22910 = CARTESIAN_POINT ( 'NONE',  ( 3.984375000614517326, 6.421520780324663323E-16, -5.243569643749999010 ) ) ;
#22911 =( BOUNDED_CURVE ( )  B_SPLINE_CURVE ( 2, ( #11021, #33187, #33542, #56093, #50551, #5484, #73079 ),
 .UNSPECIFIED., .F., .F. ) 
 B_SPLINE_CURVE_WITH_KNOTS ( ( 3, 2, 2, 3 ),
 ( 0.7500000000000000000, 0.7527777777777777679, 0.7555555555555555358, 0.7583333333333333037 ),
 .UNSPECIFIED. ) 
 CURVE ( )  GEOMETRIC_REPRESENTATION_ITEM ( )  RATIONAL_B_SPLINE_CURVE ( ( 1.000000000000000000, 0.8660254037844387076, 1.000000000000000000, 0.8660254037844387076, 1.000000000000000000, 0.8660254037844387076, 1.000000000000000000 ) ) 
 REPRESENTATION_ITEM ( '' )  );
#22912 = ORIENTED_EDGE ( 'NONE', *, *, #50906, .F. ) ;
#22913 = CARTESIAN_POINT ( 'NONE',  ( 26.55937500061451573, 4.541064518000418104, -2.621784821874998173 ) ) ;
#22914 = CARTESIAN_POINT ( 'NONE',  ( 16.11562500061451786, 3.027376345333613106, -5.243569643749998122 ) ) ;
#22915 = CARTESIAN_POINT ( 'NONE',  ( 26.88750000122903216, 4.330127018922191873, 2.499999999999999556 ) ) ;
#22916 = CARTESIAN_POINT ( 'NONE',  ( 27.96562500061451928, 3.027376345333611329, 5.243569643749999010 ) ) ;
#22917 = CARTESIAN_POINT ( 'NONE',  ( 21.87187500061451573, -6.054752690667223547, -1.112240025338166033E-15 ) ) ;
#22918 = CARTESIAN_POINT ( 'NONE',  ( 16.60312500061451857, 4.541064518000418104, -2.621784821874998173 ) ) ;
#22919 = CARTESIAN_POINT ( 'NONE',  ( 2.121784821875001281, 19.55937500061451573, 33.67503911421598417 ) ) ;
#22920 = CARTESIAN_POINT ( 'NONE',  ( 21.74062500061451431, -3.027376345333614438, 5.243569643749998122 ) ) ;
#22921 = CARTESIAN_POINT ( 'NONE',  ( 4.387500001229033053, 4.330127018922191873, 2.499999999999999556 ) ) ;
#22922 = ORIENTED_EDGE ( 'NONE', *, *, #26612, .F. ) ;
#22923 = CARTESIAN_POINT ( 'NONE',  ( 28.42499999999999716, 6.123233995736764310E-16, -4.999999999999998224 ) ) ;
#22924 = CARTESIAN_POINT ( 'NONE',  ( -1.999999999999997113, 13.32499999999999929, -26.53589838486224295 ) ) ;
#22925 = CARTESIAN_POINT ( 'NONE',  ( 3.756430356250000546, 17.74062499938548143, 27.83122392262697886 ) ) ;
#22926 = CARTESIAN_POINT ( 'NONE',  ( 28.52812500061451573, -4.541064518000419881, 2.621784821874995952 ) ) ;
#22927 = CARTESIAN_POINT ( 'NONE',  ( 10.90312500061451928, 0.000000000000000000, 5.243569643749999010 ) ) ;
#22928 = CARTESIAN_POINT ( 'NONE',  ( 23.28750000122903430, 4.330127018922191873, 2.499999999999999556 ) ) ;
#22929 = CARTESIAN_POINT ( 'NONE',  ( 12.64687500061451786, 6.054752690667223547, 3.707466751127219781E-16 ) ) ;
#22930 = CARTESIAN_POINT ( 'NONE',  ( 27.06562500061451004, 3.027376345333611329, 5.243569643749999010 ) ) ;
#22931 = CARTESIAN_POINT ( 'NONE',  ( 27.03750000000000142, -2.886751345948125991, -5.000000000000000000 ) ) ;
#22932 = CARTESIAN_POINT ( 'NONE',  ( 3.999999999999999112, 18.53750000122903430, -30.00000000000000000 ) ) ;
#22933 = CARTESIAN_POINT ( 'NONE',  ( 2.803125000614518747, 0.000000000000000000, 5.243569643749999010 ) ) ;
#22934 = CARTESIAN_POINT ( 'NONE',  ( 11.99062500061451608, -3.027376345333610441, -5.243569643749999898 ) ) ;
#22935 = ORIENTED_EDGE ( 'NONE', *, *, #46820, .T. ) ;
#22936 = CARTESIAN_POINT ( 'NONE',  ( 11.20312500061451644, 4.541064518000418104, -2.621784821874998173 ) ) ;
#22937 = AXIS2_PLACEMENT_3D ( 'NONE', #34491, #58098, #23404 ) ;
#22938 = CARTESIAN_POINT ( 'NONE',  ( 5.165625000614518569, -6.054752690667223547, -1.112240025338166033E-15 ) ) ;
#22939 = CARTESIAN_POINT ( 'NONE',  ( 17.44687500061451857, -2.746126346562642428, -4.756430356249999214 ) ) ;
#22940 = LINE ( 'NONE', #34754, #13759 ) ;
#22941 = CARTESIAN_POINT ( 'NONE',  ( 15.63749999999999751, -2.886751345948129988, 4.999999999999997335 ) ) ;
#22943 = CARTESIAN_POINT ( 'NONE',  ( 15.94687500061451502, -3.027376345333614438, 5.243569643749998122 ) ) ;
#22942 = AXIS2_PLACEMENT_3D ( 'NONE', #5991, #68779, #1546 ) ;
#22944 = CARTESIAN_POINT ( 'NONE',  ( 10.95000000122903394, -2.886751345948125991, -5.000000000000000000 ) ) ;
#22945 = CARTESIAN_POINT ( 'NONE',  ( 20.44687500061451857, -3.027376345333614438, 5.243569643749998122 ) ) ;
#22946 = CARTESIAN_POINT ( 'NONE',  ( 20.43749999999999645, 5.773502691896255534, 3.535250795749688894E-16 ) ) ;
#22947 = CARTESIAN_POINT ( 'NONE',  ( 21.90937500061451715, -4.541064518000417216, -2.621784821875001281 ) ) ;
#22948 = CARTESIAN_POINT ( 'NONE',  ( -2.121784821874999949, 15.22812500061451679, -33.67503911421598417 ) ) ;
#22949 = AXIS2_PLACEMENT_3D ( 'NONE', #53123, #36862, #8062 ) ;
#22950 = CARTESIAN_POINT ( 'NONE',  ( 1.592000809091587073E-14, 16.73750000000000071, 26.00000000000000000 ) ) ;
#22951 = CARTESIAN_POINT ( 'NONE',  ( 25.88437500061451502, -2.746126346562641984, -4.756430356249999214 ) ) ;
#22952 = CARTESIAN_POINT ( 'NONE',  ( 26.91562500061451146, 3.027376345333613106, -5.243569643749998122 ) ) ;
#22953 = CARTESIAN_POINT ( 'NONE',  ( 28.99687500061451573, -3.027376345333614438, 5.243569643749998122 ) ) ;
#22954 = ADVANCED_FACE ( 'NONE', ( #42871 ), #66127, .F. ) ;
#22955 =( BOUNDED_CURVE ( )  B_SPLINE_CURVE ( 2, ( #61950, #11354, #56415, #28337, #7254, #30145, #34964 ),
 .UNSPECIFIED., .F., .F. ) 
 B_SPLINE_CURVE_WITH_KNOTS ( ( 3, 2, 2, 3 ),
 ( 0.07999999999999998779, 0.08333333333333331483, 0.08666666666666664187, 0.08999999999999996891 ),
 .UNSPECIFIED. ) 
 CURVE ( )  GEOMETRIC_REPRESENTATION_ITEM ( )  RATIONAL_B_SPLINE_CURVE ( ( 1.000000000000000666, 0.8660254037844381525, 1.000000000000000000, 0.8660254037844387076, 1.000000000000000000, 0.8660254037844398178, 0.9999999999999988898 ) ) 
 REPRESENTATION_ITEM ( '' )  );
#22956 = CARTESIAN_POINT ( 'NONE',  ( 25.12499999999999645, -4.330127018922194537, 2.499999999999995559 ) ) ;
#22957 = CARTESIAN_POINT ( 'NONE',  ( 8.090625000614515727, 6.054752690667223547, 3.707466751127219781E-16 ) ) ;
#22958 = CARTESIAN_POINT ( 'NONE',  ( 24.75937500061451502, 2.746126346562643317, 4.756430356249998326 ) ) ;
#22959 = CARTESIAN_POINT ( 'NONE',  ( 20.22187500061451715, 3.027376345333613106, -5.243569643749998122 ) ) ;
#22960 = CARTESIAN_POINT ( 'NONE',  ( 10.99687500061451573, -4.119189519843965641, -2.378215178125001383 ) ) ;
#22961 = CARTESIAN_POINT ( 'NONE',  ( 5.953125000614519102, 0.000000000000000000, 5.243569643749999010 ) ) ;
#22962 = CARTESIAN_POINT ( 'NONE',  ( 10.05937500061451750, 0.000000000000000000, 5.243569643749999010 ) ) ;
#22963 = VERTEX_POINT ( 'NONE', #20685 ) ;
#22964 = CARTESIAN_POINT ( 'NONE',  ( 21.87187500061451573, -6.054752690667223547, -1.112240025338166033E-15 ) ) ;
#22965 = CARTESIAN_POINT ( 'NONE',  ( 8.231250001229033941, 6.123233995736764310E-16, -4.999999999999998224 ) ) ;
#22966 = CARTESIAN_POINT ( 'NONE',  ( 29.02499999999999858, 4.330127018922191873, 2.499999999999999556 ) ) ;
#22967 = CARTESIAN_POINT ( 'NONE',  ( 29.85937500061451644, 0.000000000000000000, 5.243569643749999010 ) ) ;
#22968 = CARTESIAN_POINT ( 'NONE',  ( 15.60000000122903607, 5.773502691896255534, 3.535250795749688894E-16 ) ) ;
#22969 = DIRECTION ( 'NONE',  ( -1.000000000000000000, -0.000000000000000000, -0.000000000000000000 ) ) ;
#22970 = CARTESIAN_POINT ( 'NONE',  ( 17.17500000000000071, 6.123233995736764310E-16, -4.999999999999998224 ) ) ;
#22971 = VERTEX_POINT ( 'NONE', #15875 ) ;
#22972 = CARTESIAN_POINT ( 'NONE',  ( 13.08750000000000036, -2.886751345948125991, -5.000000000000000000 ) ) ;
#22973 = CARTESIAN_POINT ( 'NONE',  ( 13.65937500061451537, -5.492252693125287522, -1.008910452111647106E-15 ) ) ;
#22974 = CARTESIAN_POINT ( 'NONE',  ( 23.39062500061451289, 6.054752690667223547, 3.707466751127219781E-16 ) ) ;
#22975 = CARTESIAN_POINT ( 'NONE',  ( 14.96250000000000036, 2.886751345948129099, -4.999999999999998224 ) ) ;
#22976 = CARTESIAN_POINT ( 'NONE',  ( 11.13750000122903216, 4.330127018922191873, 2.499999999999999556 ) ) ;
#22977 = CARTESIAN_POINT ( 'NONE',  ( 9.815625000614518925, 3.027376345333613106, -5.243569643749998122 ) ) ;
#22978 = CARTESIAN_POINT ( 'NONE',  ( 8.287499999999999645, 5.773502691896255534, 3.535250795749688894E-16 ) ) ;
#22979 = CARTESIAN_POINT ( 'NONE',  ( 1.138803498474273873E-14, 15.08749999999999858, 34.00000000000000000 ) ) ;
#22980 = CARTESIAN_POINT ( 'NONE',  ( 28.50000000122903288, -2.886751345948125991, -5.000000000000000000 ) ) ;
#22981 = CARTESIAN_POINT ( 'NONE',  ( 2.655984681222220721E-16, 18.15312499938548285, 25.66244784525396483 ) ) ;
#22982 = CARTESIAN_POINT ( 'NONE',  ( 7.012500000000001066, 2.886751345948126879, 4.999999999999999112 ) ) ;
#22983 = CARTESIAN_POINT ( 'NONE',  ( 45.00000000000000000, 0.000000000000000000, 0.000000000000000000 ) ) ;
#22984 = AXIS2_PLACEMENT_3D ( 'NONE', #56718, #68904, #62273 ) ;
#22985 = ORIENTED_EDGE ( 'NONE', *, *, #7045, .F. ) ;
#22986 = CARTESIAN_POINT ( 'NONE',  ( 22.75312500061451360, -4.541064518000417216, -2.621784821875001281 ) ) ;
#22987 = CARTESIAN_POINT ( 'NONE',  ( 29.09062500061451573, -3.027376345333610441, -5.243569643749999898 ) ) ;
#22988 = CARTESIAN_POINT ( 'NONE',  ( 29.59687500061451715, -3.027376345333610441, -5.243569643749999898 ) ) ;
#22989 = CARTESIAN_POINT ( 'NONE',  ( 18.98437500061451644, 4.541064518000418104, 2.621784821874999949 ) ) ;
#22990 = CARTESIAN_POINT ( 'NONE',  ( 16.67812500061451786, 4.541064518000418104, 2.621784821874999949 ) ) ;
#22991 = CARTESIAN_POINT ( 'NONE',  ( 2.121784821874999061, 11.10312500061459318, -33.67503911421598417 ) ) ;
#22992 = CARTESIAN_POINT ( 'NONE',  ( 5.765625000614519102, 3.027376345333613106, -5.243569643749998122 ) ) ;
#22993 = AXIS2_PLACEMENT_3D ( 'NONE', #11187, #22622, #23347 ) ;
#22994 = CARTESIAN_POINT ( 'NONE',  ( 2.878125000614517592, -4.541064518000419881, 2.621784821874995952 ) ) ;
#22995 = CARTESIAN_POINT ( 'NONE',  ( 20.97187500061451715, -5.492252693125287522, -1.008910452111647106E-15 ) ) ;
#22996 = CARTESIAN_POINT ( 'NONE',  ( 19.00312500061451715, 0.000000000000000000, 5.243569643749999010 ) ) ;
#22997 = CARTESIAN_POINT ( 'NONE',  ( 4.898587196589411843E-16, 20.00000000000000000, -26.00000000000000000 ) ) ;
#22998 = CARTESIAN_POINT ( 'NONE',  ( 4.387500001229033053, 4.330127018922191873, 2.499999999999999556 ) ) ;
#22999 = CARTESIAN_POINT ( 'NONE',  ( 12.68437500061451573, 4.541064518000418104, 2.621784821874999949 ) ) ;
#23000 = CARTESIAN_POINT ( 'NONE',  ( 11.52187500061451608, -6.054752690667223547, -1.112240025338166033E-15 ) ) ;
#23001 = CARTESIAN_POINT ( 'NONE',  ( 19.39687500061451786, 6.054752690667223547, 3.707466751127219781E-16 ) ) ;
#23002 = ORIENTED_EDGE ( 'NONE', *, *, #72525, .F. ) ;
#23003 = CARTESIAN_POINT ( 'NONE',  ( -4.513148444473918275, 8.924709038934331318, 26.04167052991142839 ) ) ;
#23004 = CARTESIAN_POINT ( 'NONE',  ( 24.02812500061451573, -4.541064518000419881, 2.621784821874995952 ) ) ;
#23005 = AXIS2_PLACEMENT_3D ( 'NONE', #66887, #38810, #28437 ) ;
#23006 = CARTESIAN_POINT ( 'NONE',  ( 17.97187500061451715, 3.027376345333613106, -5.243569643749998122 ) ) ;
#23007 = CARTESIAN_POINT ( 'NONE',  ( 24.85312500061451502, 0.000000000000000000, 5.243569643749999010 ) ) ;
#23008 = CARTESIAN_POINT ( 'NONE',  ( 3.999999999999998668, 12.16250000000000320, -32.30940107675850470 ) ) ;
#23009 = CARTESIAN_POINT ( 'NONE',  ( 3.999999999999998668, 17.56250000000000000, 27.69059892324149175 ) ) ;
#23010 = CARTESIAN_POINT ( 'NONE',  ( 5.484375000614518214, 4.541064518000418104, 2.621784821874999949 ) ) ;
#23011 = CARTESIAN_POINT ( 'NONE',  ( 11.13750000122903216, 4.330127018922191873, 2.499999999999999556 ) ) ;
#23012 = VECTOR ( 'NONE', #64511, 1000.000000000000000 ) ;
#23013 = CARTESIAN_POINT ( 'NONE',  ( 7.387500001229032165, 6.123233995736764310E-16, -4.999999999999998224 ) ) ;
#23014 = CARTESIAN_POINT ( 'NONE',  ( 8.484601909799253346E-16, 19.66249999999999787, -25.38119784648299770 ) ) ;
#23015 = CARTESIAN_POINT ( 'NONE',  ( 27.18750000122903288, 6.123233995736764310E-16, -4.999999999999998224 ) ) ;
#23016 = CARTESIAN_POINT ( 'NONE',  ( 4.000000000000000000, 18.29374999877096641, 30.00000000000000000 ) ) ;
#23017 = CARTESIAN_POINT ( 'NONE',  ( 16.85625000122903572, 4.330127018922192761, -2.499999999999997780 ) ) ;
#23018 = CARTESIAN_POINT ( 'NONE',  ( 10.43437500061451750, 4.541064518000418104, 2.621784821874999949 ) ) ;
#23019 = CARTESIAN_POINT ( 'NONE',  ( -1.071796769724492115, 17.71115380933863293, 34.00000000000000000 ) ) ;
#23020 = EDGE_CURVE ( 'NONE', #66787, #35925, #13035, .T. ) ;
#23021 = CARTESIAN_POINT ( 'NONE',  ( 16.34062500061451573, -3.027376345333614438, 5.243569643749998122 ) ) ;
#23022 = CARTESIAN_POINT ( 'NONE',  ( 12.53437500061451537, 6.421520780324663323E-16, -5.243569643749999010 ) ) ;
#23023 = CARTESIAN_POINT ( 'NONE',  ( 28.95000000122903572, -2.886751345948125991, -5.000000000000000000 ) ) ;
#23024 = CARTESIAN_POINT ( 'NONE',  ( 20.78437500061451715, 4.541064518000418104, 2.621784821874999949 ) ) ;
#23025 = CARTESIAN_POINT ( 'NONE',  ( 10.62187500061451928, -6.054752690667223547, -1.112240025338166033E-15 ) ) ;
#23026 = CARTESIAN_POINT ( 'NONE',  ( 3.069550706496567027, -3.946908300287443883, -3.323927455962977895 ) ) ;
#23027 = CARTESIAN_POINT ( 'NONE',  ( 11.88750000122903216, 6.123233995736764310E-16, -4.999999999999998224 ) ) ;
#23028 = CARTESIAN_POINT ( 'NONE',  ( 6.450000001229034829, -2.886751345948125991, -5.000000000000000000 ) ) ;
#23029 = CARTESIAN_POINT ( 'NONE',  ( 20.72812500061451502, 4.541064518000418104, 2.621784821874999949 ) ) ;
#23030 = ORIENTED_EDGE ( 'NONE', *, *, #13214, .T. ) ;
#23031 = CARTESIAN_POINT ( 'NONE',  ( 5.175000001229033586, 2.886751345948129099, -4.999999999999998224 ) ) ;
#23032 = CARTESIAN_POINT ( 'NONE',  ( 16.75312500061451715, 0.000000000000000000, 5.243569643749999010 ) ) ;
#23033 = CARTESIAN_POINT ( 'NONE',  ( 13.82812500061451466, 6.421520780324663323E-16, -5.243569643749999010 ) ) ;
#23034 = CARTESIAN_POINT ( 'NONE',  ( 25.17187500061451644, 2.746126346562645981, -4.756430356249997438 ) ) ;
#23035 = CARTESIAN_POINT ( 'NONE',  ( 14.02499999999999858, 6.123233995736764310E-16, -4.999999999999998224 ) ) ;
#23036 = CARTESIAN_POINT ( 'NONE',  ( 9.525000001229033231, -5.773502691896255534, -1.060575238724906372E-15 ) ) ;
#23037 = CARTESIAN_POINT ( 'NONE',  ( 6.778125000614518392, 4.541064518000418104, 2.621784821874999949 ) ) ;
#23038 = CARTESIAN_POINT ( 'NONE',  ( 19.31250000122903288, 0.000000000000000000, 4.999999999999998224 ) ) ;
#23039 = CARTESIAN_POINT ( 'NONE',  ( 27.48749999999999716, -2.886751345948125991, -5.000000000000000000 ) ) ;
#23040 = AXIS2_PLACEMENT_3D ( 'NONE', #45002, #72342, #34621 ) ;
#23041 = CARTESIAN_POINT ( 'NONE',  ( 9.001249775931846008E-16, 12.32187500061451857, -25.09994784771203058 ) ) ;
#23042 = CARTESIAN_POINT ( 'NONE',  ( 9.975000000000001421, 6.123233995736764310E-16, -4.999999999999998224 ) ) ;
#23043 = CARTESIAN_POINT ( 'NONE',  ( 65.00000000000000000, -6.363961030678960462, -6.363961030678893849 ) ) ;
#23044 = CARTESIAN_POINT ( 'NONE',  ( 18.60937500061451644, 0.000000000000000000, 5.243569643749999010 ) ) ;
#23045 = EDGE_CURVE ( 'NONE', #64545, #61968, #32480, .T. ) ;
#23046 = CARTESIAN_POINT ( 'NONE',  ( 29.77499999999999858, 6.123233995736764310E-16, -4.999999999999998224 ) ) ;
#23047 = CIRCLE ( 'NONE', #671, 1.500000000000000222 ) ;
#23048 = CARTESIAN_POINT ( 'NONE',  ( 16.94062500061451715, -3.027376345333610441, -5.243569643749999898 ) ) ;
#23049 = CARTESIAN_POINT ( 'NONE',  ( 9.806250001229033231, 0.000000000000000000, 4.999999999999998224 ) ) ;
#23050 = CARTESIAN_POINT ( 'NONE',  ( 65.00000000000000000, -1.494782592887706096, -8.874999999999992895 ) ) ;
#23051 = CARTESIAN_POINT ( 'NONE',  ( 29.44687500061451857, -3.027376345333614438, 5.243569643749998122 ) ) ;
#23052 = CARTESIAN_POINT ( 'NONE',  ( 27.23437500061451644, -4.541064518000419881, 2.621784821874995952 ) ) ;
#23053 = CARTESIAN_POINT ( 'NONE',  ( 18.68437500061452283, -2.746126346562641984, -4.756430356249999214 ) ) ;
#23054 = CARTESIAN_POINT ( 'NONE',  ( 12.96562500061451750, 3.027376345333613106, -5.243569643749998122 ) ) ;
#23055 = AXIS2_PLACEMENT_3D ( 'NONE', #63312, #29343, #51875 ) ;
#23056 = CARTESIAN_POINT ( 'NONE',  ( 10.58437500061451964, -4.541064518000419881, 2.621784821874995952 ) ) ;
#23057 = ORIENTED_EDGE ( 'NONE', *, *, #3230, .F. ) ;
#23058 = FACE_OUTER_BOUND ( 'NONE', #34611, .T. ) ;
#23059 = CARTESIAN_POINT ( 'NONE',  ( 20.35312500061451502, 0.000000000000000000, 5.243569643749999010 ) ) ;
#23060 = CARTESIAN_POINT ( 'NONE',  ( 27.89999999999999858, -4.330127018922190985, -2.500000000000001332 ) ) ;
#23061 = CARTESIAN_POINT ( 'NONE',  ( 20.88749999999999929, 5.773502691896255534, 3.535250795749688401E-16 ) ) ;
#23062 = CARTESIAN_POINT ( 'NONE',  ( 10.53750000000000320, 5.773502691896255534, 3.535250795749688894E-16 ) ) ;
#23063 = CARTESIAN_POINT ( 'NONE',  ( 22.61250000122903003, -4.330127018922190985, -2.500000000000001332 ) ) ;
#23064 = CARTESIAN_POINT ( 'NONE',  ( 15.62812500061451537, 6.421520780324663323E-16, -5.243569643749999010 ) ) ;
#23065 = CARTESIAN_POINT ( 'NONE',  ( 13.20937500061451431, -5.492252693125287522, -1.008910452111647106E-15 ) ) ;
#23066 = ORIENTED_EDGE ( 'NONE', *, *, #73012, .F. ) ;
#23067 = CARTESIAN_POINT ( 'NONE',  ( 19.53749999999999432, 5.773502691896255534, 3.535250795749688894E-16 ) ) ;
#23068 = CARTESIAN_POINT ( 'NONE',  ( 21.60000000000000142, -4.330127018922190985, -2.500000000000001332 ) ) ;
#23069 = CARTESIAN_POINT ( 'NONE',  ( 20.33437500061451786, 4.541064518000418104, 2.621784821874999949 ) ) ;
#23070 = CARTESIAN_POINT ( 'NONE',  ( 24.66562500061451502, 3.027376345333613106, -5.243569643749998122 ) ) ;
#23071 = ORIENTED_EDGE ( 'NONE', *, *, #53045, .F. ) ;
#23072 = CARTESIAN_POINT ( 'NONE',  ( 45.00000000000000000, 0.000000000000000000, 0.000000000000000000 ) ) ;
#23073 = CARTESIAN_POINT ( 'NONE',  ( 8.203125000614518214, 0.000000000000000000, 5.243569643749999010 ) ) ;
#23074 = CARTESIAN_POINT ( 'NONE',  ( 14.17500000000000071, 4.330127018922191873, 2.499999999999999556 ) ) ;
#23075 = CARTESIAN_POINT ( 'NONE',  ( 9.001249775931846008E-16, 17.21562500061451928, 34.90005215228797653 ) ) ;
#23076 = CARTESIAN_POINT ( 'NONE',  ( 29.57812500061451644, 6.421520780324663323E-16, -5.243569643749999010 ) ) ;
#23077 = CARTESIAN_POINT ( 'NONE',  ( 26.33437500061451431, -4.541064518000419881, 2.621784821874995952 ) ) ;
#23078 = ORIENTED_EDGE ( 'NONE', *, *, #49537, .T. ) ;
#23079 = CARTESIAN_POINT ( 'NONE',  ( 25.07812500061451644, 6.421520780324663323E-16, -5.243569643749999010 ) ) ;
#23080 = CARTESIAN_POINT ( 'NONE',  ( 24.19687500061451857, -3.027376345333610441, -5.243569643749999898 ) ) ;
#23081 = CARTESIAN_POINT ( 'NONE',  ( 4.243569643749999898, 19.09062500061459389, -27.54997392385601529 ) ) ;
#23082 = CARTESIAN_POINT ( 'NONE',  ( 11.66249999999999964, -5.773502691896255534, -1.060575238724906372E-15 ) ) ;
#23083 = CARTESIAN_POINT ( 'NONE',  ( 8.990625000614516082, 6.054752690667223547, 3.707466751127219781E-16 ) ) ;
#23084 = CARTESIAN_POINT ( 'NONE',  ( 28.09687500061451715, -2.746126346562646425, 4.756430356249996549 ) ) ;
#23085 = CARTESIAN_POINT ( 'NONE',  ( 28.90312500061451217, 0.000000000000000000, 5.243569643749999010 ) ) ;
#23086 = CARTESIAN_POINT ( 'NONE',  ( 26.91562500061451502, 3.027376345333612662, -5.243569643749998122 ) ) ;
#23087 = CARTESIAN_POINT ( 'NONE',  ( 12.56250000122903465, 0.000000000000000000, 4.999999999999998224 ) ) ;
#23088 = CARTESIAN_POINT ( 'NONE',  ( 12.00937500061451857, -4.119189519843965641, -2.378215178125001383 ) ) ;
#23089 = CARTESIAN_POINT ( 'NONE',  ( 19.54687500061451644, -3.027376345333614438, 5.243569643749998122 ) ) ;
#23090 = CARTESIAN_POINT ( 'NONE',  ( 2.121784821875001281, 14.60937500061451821, 33.67503911421598417 ) ) ;
#23091 = CARTESIAN_POINT ( 'NONE',  ( 19.69687500061451857, -3.027376345333610441, -5.243569643749999898 ) ) ;
#23092 = CARTESIAN_POINT ( 'NONE',  ( 28.32187500061451502, 3.027376345333613106, -5.243569643749998122 ) ) ;
#23093 = CARTESIAN_POINT ( 'NONE',  ( 4.243569643749999898, 16.93437500061451573, 30.00000000000000000 ) ) ;
#23094 = CARTESIAN_POINT ( 'NONE',  ( 9.140625000614518214, -3.027376345333614438, 5.243569643749998122 ) ) ;
#23095 = DIRECTION ( 'NONE',  ( 0.000000000000000000, 0.000000000000000000, 1.000000000000000000 ) ) ;
#23096 = CARTESIAN_POINT ( 'NONE',  ( 4.771875000614516971, -6.054752690667223547, -1.112240025338166033E-15 ) ) ;
#23097 = CARTESIAN_POINT ( 'NONE',  ( 1.626862140677534273E-15, 15.61250000000000071, -26.00000000000000355 ) ) ;
#23098 = CARTESIAN_POINT ( 'NONE',  ( 7.378125000614518036, -4.541064518000419881, 2.621784821874995952 ) ) ;
#23099 = CARTESIAN_POINT ( 'NONE',  ( 10.95937500061451964, 0.000000000000000000, 5.243569643749999010 ) ) ;
#23100 = CARTESIAN_POINT ( 'NONE',  ( 0.000000000000000000, 0.000000000000000000, 0.000000000000000000 ) ) ;
#23101 = CARTESIAN_POINT ( 'NONE',  ( 19.20000000122903572, 5.773502691896255534, 3.535250795749688894E-16 ) ) ;
#23102 = CARTESIAN_POINT ( 'NONE',  ( 5.371875000614516615, 3.027376345333613106, -5.243569643749998122 ) ) ;
#23103 = CARTESIAN_POINT ( 'NONE',  ( 7.040625000614517681, -3.027376345333610441, -5.243569643749999898 ) ) ;
#23104 = CARTESIAN_POINT ( 'NONE',  ( 5.428125000614517859, 4.541064518000418104, 2.621784821874999949 ) ) ;
#23105 = CARTESIAN_POINT ( 'NONE',  ( 23.98125000122903216, 6.123233995736764310E-16, -4.999999999999998224 ) ) ;
#23106 = CARTESIAN_POINT ( 'NONE',  ( 19.95937500061451786, 0.000000000000000000, 5.243569643749999010 ) ) ;
#23107 = CARTESIAN_POINT ( 'NONE',  ( 3.999999999999999112, 13.13750000122903394, 30.00000000000000000 ) ) ;
#23108 = ORIENTED_EDGE ( 'NONE', *, *, #47762, .F. ) ;
#23109 = CARTESIAN_POINT ( 'NONE',  ( 24.25312500061451715, 4.541064518000418104, -2.621784821874998173 ) ) ;
#23110 = CARTESIAN_POINT ( 'NONE',  ( 11.76562500061451644, 3.027376345333611329, 5.243569643749999010 ) ) ;
#23111 = CARTESIAN_POINT ( 'NONE',  ( 29.85937500061451644, 0.000000000000000000, 5.243569643749999010 ) ) ;
#23112 = CARTESIAN_POINT ( 'NONE',  ( 11.61562500061451608, 3.027376345333613106, -5.243569643749998122 ) ) ;
#23113 = CARTESIAN_POINT ( 'NONE',  ( 25.36875000122903145, 2.886751345948087355, -5.000000000000071054 ) ) ;
#23114 = CARTESIAN_POINT ( 'NONE',  ( 11.70000000122903216, -2.886751345948129988, 4.999999999999997335 ) ) ;
#23115 = EDGE_CURVE ( 'NONE', #72906, #42612, #22426, .T. ) ;
#23116 = CARTESIAN_POINT ( 'NONE',  ( 28.49062500061451431, -3.027376345333614438, 5.243569643749998122 ) ) ;
#23117 = CARTESIAN_POINT ( 'NONE',  ( 4.243569643749999010, 12.86562500061451608, -32.45002607614398471 ) ) ;
#23118 = CARTESIAN_POINT ( 'NONE',  ( 14.66250000122903252, 4.330127018922192761, -2.499999999999997780 ) ) ;
#23119 = AXIS2_PLACEMENT_3D ( 'NONE', #26256, #71321, #66141 ) ;
#23120 = CARTESIAN_POINT ( 'NONE',  ( 11.70000000000000284, -4.330127018922190985, -2.500000000000001332 ) ) ;
#23121 = CARTESIAN_POINT ( 'NONE',  ( 21.55312500061451431, 4.541064518000418104, -2.621784821874998173 ) ) ;
#23122 = CARTESIAN_POINT ( 'NONE',  ( 8.146875000614516082, 6.054752690667223547, 3.707466751127219781E-16 ) ) ;
#23123 = CARTESIAN_POINT ( 'NONE',  ( 7.462500001229035007, 4.330127018922192761, -2.499999999999997780 ) ) ;
#23124 = CARTESIAN_POINT ( 'NONE',  ( 15.60000000122903607, 5.773502691896255534, 3.535250795749688894E-16 ) ) ;
#23125 = CARTESIAN_POINT ( 'NONE',  ( 12.59062500061451573, 6.054752690667223547, 3.707466751127219781E-16 ) ) ;
#23126 =( BOUNDED_CURVE ( )  B_SPLINE_CURVE ( 2, ( #34143, #51149, #23060, #45615, #50788, #17512, #33789 ),
 .UNSPECIFIED., .F., .F. ) 
 B_SPLINE_CURVE_WITH_KNOTS ( ( 3, 2, 2, 3 ),
 ( 0.08999999999999996891, 0.09333333333333329596, 0.09666666666666662300, 0.09999999999999995004 ),
 .UNSPECIFIED. ) 
 CURVE ( )  GEOMETRIC_REPRESENTATION_ITEM ( )  RATIONAL_B_SPLINE_CURVE ( ( 1.000000000000001110, 0.8660254037844374864, 1.000000000000000000, 0.8660254037844387076, 1.000000000000000000, 0.8660254037844409281, 0.9999999999999977796 ) ) 
 REPRESENTATION_ITEM ( '' )  );
#23127 = CARTESIAN_POINT ( 'NONE',  ( 16.30312500061451786, 0.000000000000000000, 5.243569643749999010 ) ) ;
#23128 = CARTESIAN_POINT ( 'NONE',  ( 26.10000000122903430, -2.886751345948129988, 4.999999999999997335 ) ) ;
#23129 = CARTESIAN_POINT ( 'NONE',  ( 20.06250000000000000, 2.886751345948126879, 4.999999999999999112 ) ) ;
#23130 = CARTESIAN_POINT ( 'NONE',  ( 22.24687500061451217, -3.027376345333614438, 5.243569643749998122 ) ) ;
#23131 = CARTESIAN_POINT ( 'NONE',  ( 4.648177544792955741E-15, 13.73749999999999716, 33.99999999999999289 ) ) ;
#23132 = CARTESIAN_POINT ( 'NONE',  ( 9.562500001229032875, -4.330127018922190985, -2.500000000000001332 ) ) ;
#23133 = CARTESIAN_POINT ( 'NONE',  ( 8.371875000614515727, -6.054752690667223547, -1.112240025338166033E-15 ) ) ;
#23134 = CARTESIAN_POINT ( 'NONE',  ( 27.94687500061451502, 6.054752690667223547, 3.707466751127219781E-16 ) ) ;
#23135 = EDGE_CURVE ( 'NONE', #45736, #70526, #27620, .T. ) ;
#23136 = CARTESIAN_POINT ( 'NONE',  ( 3.534375000614518036, 6.421520780324663323E-16, -5.243569643749999010 ) ) ;
#23137 = CARTESIAN_POINT ( 'NONE',  ( 23.69062500061451004, -3.027376345333610441, -5.243569643749999898 ) ) ;
#23138 = CARTESIAN_POINT ( 'NONE',  ( -3.756430356250000102, 15.22812499938548392, 30.00000000000000000 ) ) ;
#23139 = CARTESIAN_POINT ( 'NONE',  ( 4.625252677371872068, -1.901857634188764745, -4.625252677371872068 ) ) ;
#23140 = CARTESIAN_POINT ( 'NONE',  ( 8.221875000614518925, 3.027376345333611329, 5.243569643749999010 ) ) ;
#23141 = CARTESIAN_POINT ( 'NONE',  ( 4.993151921736298959, -0.2997683513397194077, 5.126451599955896832 ) ) ;
#23142 = CARTESIAN_POINT ( 'NONE',  ( 27.32812500061451644, 6.421520780324663323E-16, -5.243569643749999010 ) ) ;
#23143 = CARTESIAN_POINT ( 'NONE',  ( 7.584375000614516082, 6.421520780324663323E-16, -5.243569643749999010 ) ) ;
#23144 = CARTESIAN_POINT ( 'NONE',  ( 6.600000000000001421, 0.000000000000000000, 4.999999999999998224 ) ) ;
#23145 = PRODUCT ( 'knob', 'knob', '', ( #15650 ) ) ;
#23146 = CARTESIAN_POINT ( 'NONE',  ( 25.35937500061451644, 0.000000000000000000, 5.243569643749999010 ) ) ;
#23147 = CARTESIAN_POINT ( 'NONE',  ( 29.08125000122903003, 4.330127018922191873, 2.499999999999999556 ) ) ;
#23148 = CARTESIAN_POINT ( 'NONE',  ( 19.04999999999999716, 4.330127018922192761, -2.499999999999997780 ) ) ;
#23149 = ORIENTED_EDGE ( 'NONE', *, *, #43888, .T. ) ;
#23150 = CARTESIAN_POINT ( 'NONE',  ( 27.15000000000000213, 4.330127018922192761, -2.499999999999997780 ) ) ;
#23151 = CARTESIAN_POINT ( 'NONE',  ( 27.98437500061451289, 4.541064518000418104, 2.621784821874999949 ) ) ;
#23152 = ORIENTED_EDGE ( 'NONE', *, *, #59010, .F. ) ;
#23153 = CARTESIAN_POINT ( 'NONE',  ( 15.62812500061451537, 6.421520780324663323E-16, -5.243569643749999010 ) ) ;
#23154 = CARTESIAN_POINT ( 'NONE',  ( 9.290625000614515017, -3.027376345333610441, -5.243569643749999898 ) ) ;
#23155 = CARTESIAN_POINT ( 'NONE',  ( 18.00937500061451502, 2.746126346562643317, 4.756430356249998326 ) ) ;
#23156 = CARTESIAN_POINT ( 'NONE',  ( 5.034375000614519813, 4.541064518000418104, 2.621784821874999949 ) ) ;
#23157 = CARTESIAN_POINT ( 'NONE',  ( 17.66250000122903430, -4.330127018922190985, -2.500000000000001332 ) ) ;
#23158 = CARTESIAN_POINT ( 'NONE',  ( 21.52499999999999858, -4.330127018922194537, 2.499999999999995559 ) ) ;
#23159 = CARTESIAN_POINT ( 'NONE',  ( 29.17500000000000071, -4.330127018922194537, 2.499999999999995559 ) ) ;
#23160 = CARTESIAN_POINT ( 'NONE',  ( 5.671875000614519102, -6.054752690667223547, -1.112240025338166033E-15 ) ) ;
#23161 = CARTESIAN_POINT ( 'NONE',  ( 12.72187500061451537, 3.027376345333611329, 5.243569643749999010 ) ) ;
#23162 = CARTESIAN_POINT ( 'NONE',  ( 22.80937500061451573, -4.541064518000417216, -2.621784821875001281 ) ) ;
#23163 = ORIENTED_EDGE ( 'NONE', *, *, #13474, .F. ) ;
#23164 = CARTESIAN_POINT ( 'NONE',  ( 3.421875000614516882, -6.054752690667223547, -1.112240025338166033E-15 ) ) ;
#23165 =( BOUNDED_CURVE ( )  B_SPLINE_CURVE ( 2, ( #40110, #43003, #20082, #53724, #48918, #2385, #31922 ),
 .UNSPECIFIED., .F., .F. ) 
 B_SPLINE_CURVE_WITH_KNOTS ( ( 3, 2, 2, 3 ),
 ( 0.4833333333333333925, 0.4861111111111111605, 0.4888888888888888729, 0.4916666666666666408 ),
 .UNSPECIFIED. ) 
 CURVE ( )  GEOMETRIC_REPRESENTATION_ITEM ( )  RATIONAL_B_SPLINE_CURVE ( ( 0.9999999999999973355, 0.8660254037844413721, 1.000000000000000000, 0.8660254037844387076, 1.000000000000000000, 0.8660254037844387076, 1.000000000000000000 ) ) 
 REPRESENTATION_ITEM ( '' )  );
#23166 = CARTESIAN_POINT ( 'NONE',  ( 7.584375000614516082, 6.421520780324663323E-16, -5.243569643749999010 ) ) ;
#23167 = CARTESIAN_POINT ( 'NONE',  ( 18.41250000000000142, -5.773502691896255534, -1.060575238724906372E-15 ) ) ;
#23168 = CARTESIAN_POINT ( 'NONE',  ( 16.37812500061451715, -4.541064518000419881, 2.621784821874995952 ) ) ;
#23169 = CARTESIAN_POINT ( 'NONE',  ( 4.000000000000000000, 19.70000000000000284, 30.00000000000000000 ) ) ;
#23170 = CARTESIAN_POINT ( 'NONE',  ( 24.93750000122903288, 6.123233995736764310E-16, -4.999999999999998224 ) ) ;
#23171 = CARTESIAN_POINT ( 'NONE',  ( 21.08437500061451786, 5.824947211148865298E-16, -4.756430356249998326 ) ) ;
#23172 = CARTESIAN_POINT ( 'NONE',  ( 11.12812500061451715, 6.421520780324663323E-16, -5.243569643749999010 ) ) ;
#23173 = CARTESIAN_POINT ( 'NONE',  ( 25.62187500061451573, 3.027376345333613106, -5.243569643749998122 ) ) ;
#23174 = CARTESIAN_POINT ( 'NONE',  ( -3.999999999999999112, 19.62500000122903288, 27.69059892324149885 ) ) ;
#23175 = CARTESIAN_POINT ( 'NONE',  ( 25.50937500061451502, -4.541064518000417216, -2.621784821875001281 ) ) ;
#23176 = CARTESIAN_POINT ( 'NONE',  ( 6.637500000000001066, -2.886751345948129988, 4.999999999999997335 ) ) ;
#23177 = CARTESIAN_POINT ( 'NONE',  ( -1.999999999999997113, 12.98750000122903359, 33.46410161513775705 ) ) ;
#23178 = CARTESIAN_POINT ( 'NONE',  ( 9.375000001229036428, 2.886751345948126879, 4.999999999999999112 ) ) ;
#23179 = CARTESIAN_POINT ( 'NONE',  ( 20.48437500061451289, -4.541064518000419881, 2.621784821874995952 ) ) ;
#23180 = CARTESIAN_POINT ( 'NONE',  ( 10.73437500061451644, 6.421520780324663323E-16, -5.243569643749999010 ) ) ;
#23181 = CARTESIAN_POINT ( 'NONE',  ( -2.081578678577455488, 4.574985540471381285, -33.45664977638282522 ) ) ;
#23182 = ORIENTED_EDGE ( 'NONE', *, *, #15334, .T. ) ;
#23183 = CARTESIAN_POINT ( 'NONE',  ( 15.06562500061451537, -6.054752690667223547, -1.112240025338166033E-15 ) ) ;
#23184 = CARTESIAN_POINT ( 'NONE',  ( 25.57500000122903216, 2.886751345948126879, 4.999999999999999112 ) ) ;
#23185 = CARTESIAN_POINT ( 'NONE',  ( 13.32187500061451502, -6.054752690667223547, -1.112240025338166033E-15 ) ) ;
#23186 = CARTESIAN_POINT ( 'NONE',  ( 3.242103837493086330E-14, 12.80000000122903536, 26.00000000000000711 ) ) ;
#23187 = CARTESIAN_POINT ( 'NONE',  ( 17.87812500061451715, 6.421520780324663323E-16, -5.243569643749999010 ) ) ;
#23188 = DIRECTION ( 'NONE',  ( 0.000000000000000000, 0.000000000000000000, 1.000000000000000000 ) ) ;
#23189 = CARTESIAN_POINT ( 'NONE',  ( 26.40937500061451715, -4.541064518000417216, -2.621784821875001281 ) ) ;
#23190 = CARTESIAN_POINT ( 'NONE',  ( -2.121784821874996840, 10.87812500061451715, 33.67503911421598417 ) ) ;
#23191 = CARTESIAN_POINT ( 'NONE',  ( 11.51250000122903216, 4.330127018922192761, -2.499999999999997780 ) ) ;
#23192 = CARTESIAN_POINT ( 'NONE',  ( 7.846875000614518036, -2.746126346562646425, 4.756430356249996549 ) ) ;
#23193 = CARTESIAN_POINT ( 'NONE',  ( -4.243569643749999898, 18.05937500061451928, -30.00000000000000000 ) ) ;
#23194 = CARTESIAN_POINT ( 'NONE',  ( 17.97187500061451715, 3.027376345333613106, -5.243569643749998122 ) ) ;
#23195 = CARTESIAN_POINT ( 'NONE',  ( 20.66250000122903074, 0.000000000000000000, 4.999999999999998224 ) ) ;
#23196 =( BOUNDED_CURVE ( )  B_SPLINE_CURVE ( 2, ( #35708, #13529, #7635, #41267, #24984, #30173, #13905 ),
 .UNSPECIFIED., .F., .F. ) 
 B_SPLINE_CURVE_WITH_KNOTS ( ( 3, 2, 2, 3 ),
 ( 0.9400000000000001688, 0.9433333333333335791, 0.9466666666666667673, 0.9500000000000000666 ),
 .UNSPECIFIED. ) 
 CURVE ( )  GEOMETRIC_REPRESENTATION_ITEM ( )  RATIONAL_B_SPLINE_CURVE ( ( 0.9999999999999911182, 0.8660254037844475894, 1.000000000000000000, 0.8660254037844387076, 1.000000000000000000, 0.8660254037844342667, 1.000000000000004441 ) ) 
 REPRESENTATION_ITEM ( '' )  );
#23197 = CARTESIAN_POINT ( 'NONE',  ( 14.52187500061451608, 3.027376345333611329, 5.243569643749999010 ) ) ;
#23198 = CARTESIAN_POINT ( 'NONE',  ( -2.121784821874999949, 19.72812500061451857, -33.67503911421598417 ) ) ;
#23199 = CARTESIAN_POINT ( 'NONE',  ( 23.10000000122903074, -2.886751345948125991, -5.000000000000000000 ) ) ;
#23200 = AXIS2_PLACEMENT_3D ( 'NONE', #23300, #62466, #40667 ) ;
#23201 = CARTESIAN_POINT ( 'NONE',  ( 14.95312500061451644, 0.000000000000000000, 5.243569643749999010 ) ) ;
#23202 = CARTESIAN_POINT ( 'NONE',  ( 25.50000000000000000, 0.000000000000000000, 4.999999999999998224 ) ) ;
#23203 = ORIENTED_EDGE ( 'NONE', *, *, #45494, .F. ) ;
#23204 = ORIENTED_EDGE ( 'NONE', *, *, #41428, .F. ) ;
#23205 = CARTESIAN_POINT ( 'NONE',  ( 20.32499999999999929, 6.123233995736764310E-16, -4.999999999999998224 ) ) ;
#23206 = CARTESIAN_POINT ( 'NONE',  ( -3.137519842735245283E-14, 14.37500000122903288, 34.00000000000000000 ) ) ;
#23207 = CARTESIAN_POINT ( 'NONE',  ( 0.5511252142286459099, 4.971455555459576736, 33.96427100478815220 ) ) ;
#23208 = CARTESIAN_POINT ( 'NONE',  ( 14.77500000122903501, 2.886751345948126879, 4.999999999999999112 ) ) ;
#23209 = CARTESIAN_POINT ( 'NONE',  ( 20.20312500061451644, 4.541064518000418104, -2.621784821874998173 ) ) ;
#23210 = CARTESIAN_POINT ( 'NONE',  ( 24.10312500061451502, -4.541064518000417216, -2.621784821875001281 ) ) ;
#23211 = CARTESIAN_POINT ( 'NONE',  ( 4.190625000614518925, -3.027376345333614438, 5.243569643749998122 ) ) ;
#23212 = CARTESIAN_POINT ( 'NONE',  ( 28.76249999999999929, -5.773502691896255534, -1.060575238724906372E-15 ) ) ;
#23213 = CARTESIAN_POINT ( 'NONE',  ( -1.071796769724491005, 10.12009619066136956, -34.00000000000000000 ) ) ;
#23214 =( BOUNDED_CURVE ( )  B_SPLINE_CURVE ( 2, ( #36290, #21116, #30743, #59909, #9315, #58804, #8214, #20747, #20008 ),
 .UNSPECIFIED., .F., .F. ) 
 B_SPLINE_CURVE_WITH_KNOTS ( ( 3, 2, 2, 2, 3 ),
 ( 0.4456521739130435145, 0.4492753623188405765, 0.4565217391304347561, 0.4637681159420289911, 0.4673913043478261087 ),
 .UNSPECIFIED. ) 
 CURVE ( )  GEOMETRIC_REPRESENTATION_ITEM ( )  RATIONAL_B_SPLINE_CURVE ( ( 0.9330127018922194093, 0.9330127018922198534, 1.000000000000000000, 0.8660254037844387076, 1.000000000000000000, 0.8660254037844387076, 1.000000000000000000, 0.9330127018922188542, 0.9330127018922194093 ) ) 
 REPRESENTATION_ITEM ( '' )  );
#23215 = CARTESIAN_POINT ( 'NONE',  ( 8.746875000614515727, -2.746126346562646425, 4.756430356249996549 ) ) ;
#23216 = CARTESIAN_POINT ( 'NONE',  ( 29.52187500061451431, -6.054752690667223547, -1.112240025338166033E-15 ) ) ;
#23217 = CARTESIAN_POINT ( 'NONE',  ( -1.999999999999997113, 10.73750000122903536, -26.53589838486224295 ) ) ;
#23218 = CARTESIAN_POINT ( 'NONE',  ( -2.121784821874999949, 18.88437500061451857, -33.67503911421598417 ) ) ;
#23219 = CARTESIAN_POINT ( 'NONE',  ( 6.787500001229032520, -4.330127018922194537, 2.499999999999995559 ) ) ;
#23220 = CARTESIAN_POINT ( 'NONE',  ( 9.225000000000001421, 4.330127018922191873, 2.499999999999999556 ) ) ;
#23221 = EDGE_CURVE ( 'NONE', #48240, #30519, #44234, .T. ) ;
#23222 = CARTESIAN_POINT ( 'NONE',  ( 3.600000001229033408, -2.886751345948129988, 4.999999999999997335 ) ) ;
#23223 = CARTESIAN_POINT ( 'NONE',  ( 12.60937500061451821, 4.541064518000418104, -2.621784821874998173 ) ) ;
#23224 = CARTESIAN_POINT ( 'NONE',  ( 3.985236265425895485, -3.020202436759538589, 3.985236265425895485 ) ) ;
#23225 = CARTESIAN_POINT ( 'NONE',  ( 3.609375000614516882, 4.541064518000418104, -2.621784821874998173 ) ) ;
#23226 = CYLINDRICAL_SURFACE ( 'NONE', #47946, 4.000000000000000000 ) ;
#23227 = CARTESIAN_POINT ( 'NONE',  ( 29.43750000122903288, 6.123233995736764310E-16, -4.999999999999998224 ) ) ;
#23228 = CARTESIAN_POINT ( 'NONE',  ( 10.92187500061451644, 3.027376345333611329, 5.243569643749999010 ) ) ;
#23229 = CARTESIAN_POINT ( 'NONE',  ( 13.95937500061451786, 4.541064518000418104, -2.621784821874998173 ) ) ;
#23230 = CARTESIAN_POINT ( 'NONE',  ( 3.516709882973403367, -4.011040265794256321, 3.052674468439771527 ) ) ;
#23231 = VECTOR ( 'NONE', #5818, 1000.000000000000000 ) ;
#23232 = CARTESIAN_POINT ( 'NONE',  ( 6.712500000000000355, -5.773502691896255534, -1.060575238724906372E-15 ) ) ;
#23233 = AXIS2_PLACEMENT_3D ( 'NONE', #35669, #1349, #40505 ) ;
#23234 = CARTESIAN_POINT ( 'NONE',  ( -2.121784821874996840, 17.17812500061459247, 33.67503911421598417 ) ) ;
#23235 = CARTESIAN_POINT ( 'NONE',  ( 22.39687500061451075, -3.027376345333610441, -5.243569643749999898 ) ) ;
#23236 = CARTESIAN_POINT ( 'NONE',  ( 2.816105206925325177, -4.131560564441517869, 3.074222403557641758 ) ) ;
#23237 = CARTESIAN_POINT ( 'NONE',  ( 27.03750000122903430, -4.330127018922194537, 2.499999999999995559 ) ) ;
#23238 = CARTESIAN_POINT ( 'NONE',  ( 17.82187500061451502, 5.824947211148865298E-16, -4.756430356249998326 ) ) ;
#23239 = CARTESIAN_POINT ( 'NONE',  ( 22.90312500061451573, 4.541064518000418104, -2.621784821874998173 ) ) ;
#23240 = CARTESIAN_POINT ( 'NONE',  ( 14.57812500061451644, -4.541064518000419881, 2.621784821874995952 ) ) ;
#23241 = CARTESIAN_POINT ( 'NONE',  ( 26.14687500061451431, 0.000000000000000000, 4.756430356249998326 ) ) ;
#23242 = CARTESIAN_POINT ( 'NONE',  ( 12.15937500061451892, 4.541064518000418104, -2.621784821874998173 ) ) ;
#23243 = CARTESIAN_POINT ( 'NONE',  ( 29.09999999999999787, 0.000000000000000000, 4.999999999999998224 ) ) ;
#23244 = CARTESIAN_POINT ( 'NONE',  ( 24.86250000122903359, -4.330127018922190985, -2.500000000000001332 ) ) ;
#23245 = DIRECTION ( 'NONE',  ( -0.000000000000000000, -1.000000000000000000, -0.000000000000000000 ) ) ;
#23246 = CARTESIAN_POINT ( 'NONE',  ( 12.30937500061451573, 0.000000000000000000, 5.243569643749999010 ) ) ;
#23247 = CARTESIAN_POINT ( 'NONE',  ( 28.02187500061451431, 3.027376345333611329, 5.243569643749999010 ) ) ;
#23248 = LINE ( 'NONE', #45799, #53696 ) ;
#23249 = DIRECTION ( 'NONE',  ( 1.000000000000000000, 0.000000000000000000, 0.000000000000000000 ) ) ;
#23250 = CARTESIAN_POINT ( 'NONE',  ( 23.07187500061451857, 3.027376345333611329, 5.243569643749999010 ) ) ;
#23251 = CARTESIAN_POINT ( 'NONE',  ( 15.30937500061451750, 4.541064518000418104, -2.621784821874998173 ) ) ;
#23252 = CARTESIAN_POINT ( 'NONE',  ( -3.756430356249999214, 18.79062499938548214, 27.83122392262697531 ) ) ;
#23253 = CARTESIAN_POINT ( 'NONE',  ( 26.62500000000000000, 6.123233995736764310E-16, -4.999999999999998224 ) ) ;
#23254 = CARTESIAN_POINT ( 'NONE',  ( 2.700000001229035718, -2.886751345948129988, 4.999999999999997335 ) ) ;
#23255 = CARTESIAN_POINT ( 'NONE',  ( 28.35937500061451289, 4.119189519843966529, -2.378215178124998275 ) ) ;
#23256 = CARTESIAN_POINT ( 'NONE',  ( 16.11562500061451786, 3.027376345333613106, -5.243569643749998122 ) ) ;
#23257 = CARTESIAN_POINT ( 'NONE',  ( 8.062500000000000000, -5.773502691896255534, -1.060575238724906372E-15 ) ) ;
#23258 = CARTESIAN_POINT ( 'NONE',  ( 15.59999999999999964, 0.000000000000000000, 4.999999999999998224 ) ) ;
#23259 = CARTESIAN_POINT ( 'NONE',  ( 16.05000000000000071, 0.000000000000000000, 4.999999999999998224 ) ) ;
#23260 = CARTESIAN_POINT ( 'NONE',  ( 9.001249775931846008E-16, 12.26562500061451644, 34.90005215228797653 ) ) ;
#23261 = LINE ( 'NONE', #39914, #6554 ) ;
#23262 = CARTESIAN_POINT ( 'NONE',  ( 27.64687500061452141, -3.027376345333614438, 5.243569643749998122 ) ) ;
#23263 = VERTEX_POINT ( 'NONE', #56054 ) ;
#23264 = CARTESIAN_POINT ( 'NONE',  ( 22.56562500061451715, 3.027376345333611329, 5.243569643749999010 ) ) ;
#23265 = CARTESIAN_POINT ( 'NONE',  ( 23.22187500061451715, -6.054752690667223547, -1.112240025338166033E-15 ) ) ;
#23266 = CARTESIAN_POINT ( 'NONE',  ( 4.987500000000002487, -2.886751345948125991, -5.000000000000000000 ) ) ;
#23267 = CARTESIAN_POINT ( 'NONE',  ( 7.453125000614516438, -4.541064518000417216, -2.621784821875001281 ) ) ;
#23268 = CARTESIAN_POINT ( 'NONE',  ( 24.47812500061451502, -4.541064518000419881, 2.621784821874995952 ) ) ;
#23269 = CARTESIAN_POINT ( 'NONE',  ( 12.00937500061451857, -4.541064518000417216, -2.621784821875001281 ) ) ;
#23270 = CARTESIAN_POINT ( 'NONE',  ( 15.64687500061451608, -3.027376345333610441, -5.243569643749999898 ) ) ;
#23271 = CARTESIAN_POINT ( 'NONE',  ( 4.243569643749999898, 16.87812500061451715, 30.00000000000000000 ) ) ;
#23272 = CARTESIAN_POINT ( 'NONE',  ( 18.45000000122903216, -2.886751345948129988, 4.999999999999997335 ) ) ;
#23273 = CARTESIAN_POINT ( 'NONE',  ( 14.89687500061451786, 5.492252693125287522, 3.363034840372157021E-16 ) ) ;
#23274 = CARTESIAN_POINT ( 'NONE',  ( 9.815625000614517148, 3.027376345333612662, -5.243569643749998122 ) ) ;
#23275 = CARTESIAN_POINT ( 'NONE',  ( 6.496875000614517504, -3.027376345333614438, 5.243569643749998122 ) ) ;
#23276 = CARTESIAN_POINT ( 'NONE',  ( 4.246875000614519280, -3.027376345333614438, 5.243569643749998122 ) ) ;
#23277 = VERTEX_POINT ( 'NONE', #44973 ) ;
#23278 = CARTESIAN_POINT ( 'NONE',  ( 24.53437500061451715, -4.541064518000419881, 2.621784821874995952 ) ) ;
#23279 = CARTESIAN_POINT ( 'NONE',  ( 17.57812500061451644, 4.541064518000418104, 2.621784821874999949 ) ) ;
#23280 = CARTESIAN_POINT ( 'NONE',  ( 26.58750000122903145, -4.330127018922194537, 2.499999999999995559 ) ) ;
#23281 = EDGE_CURVE ( 'NONE', #31980, #32613, #22955, .T. ) ;
#23282 = CARTESIAN_POINT ( 'NONE',  ( 28.67812500061451431, 6.421520780324663323E-16, -5.243569643749999010 ) ) ;
#23283 = CARTESIAN_POINT ( 'NONE',  ( 22.13437500061451502, 4.541064518000418104, 2.621784821874999949 ) ) ;
#23284 = CARTESIAN_POINT ( 'NONE',  ( 17.99062500061451786, 6.054752690667223547, 3.707466751127219781E-16 ) ) ;
#23285 = CARTESIAN_POINT ( 'NONE',  ( 4.243569643749999898, 19.18437500061451928, 30.00000000000000000 ) ) ;
#23286 = ADVANCED_FACE ( 'NONE', ( #46418 ), #2434, .T. ) ;
#23287 = CARTESIAN_POINT ( 'NONE',  ( 22.60312500061451857, 0.000000000000000000, 5.243569643749999010 ) ) ;
#23288 = CARTESIAN_POINT ( 'NONE',  ( 2.850000001229036073, -2.886751345948125991, -5.000000000000000000 ) ) ;
#23289 = ORIENTED_EDGE ( 'NONE', *, *, #61121, .T. ) ;
#23290 = CARTESIAN_POINT ( 'NONE',  ( 26.84999999999999787, 0.000000000000000000, 4.999999999999998224 ) ) ;
#23291 = CARTESIAN_POINT ( 'NONE',  ( -3.999999999999999556, 12.31250000000000000, -32.30940107675850470 ) ) ;
#23292 = CARTESIAN_POINT ( 'NONE',  ( -1.878215178125001827, 18.45312499938548356, 33.25316411605952283 ) ) ;
#23293 = CARTESIAN_POINT ( 'NONE',  ( 28.37812500061451715, 4.541064518000418104, 2.621784821874999949 ) ) ;
#23294 = CARTESIAN_POINT ( 'NONE',  ( 10.49062500061451431, -3.027376345333614438, 5.243569643749998122 ) ) ;
#23295 = CARTESIAN_POINT ( 'NONE',  ( 21.56250000122903288, 0.000000000000000000, 4.999999999999998224 ) ) ;
#23296 = CARTESIAN_POINT ( 'NONE',  ( 27.55312500061451786, 0.000000000000000000, 5.243569643749999010 ) ) ;
#23297 = CARTESIAN_POINT ( 'NONE',  ( 28.23750000000000426, -2.886751345948129988, 4.999999999999997335 ) ) ;
#23298 = CARTESIAN_POINT ( 'NONE',  ( 1.999999999999998668, 17.71250000122903501, -33.46410161513775705 ) ) ;
#23299 = EDGE_CURVE ( 'NONE', #71417, #9906, #55574, .T. ) ;
#23300 = CARTESIAN_POINT ( 'NONE',  ( 30.00000000000000000, 0.000000000000000000, 0.000000000000000000 ) ) ;
#23301 = CARTESIAN_POINT ( 'NONE',  ( 10.94062500061451537, -3.027376345333614438, 5.243569643749998122 ) ) ;
#23302 = ORIENTED_EDGE ( 'NONE', *, *, #62588, .F. ) ;
#23303 = CARTESIAN_POINT ( 'NONE',  ( 6.815625000614517148, 3.027376345333611329, 5.243569643749999010 ) ) ;
#23304 = CARTESIAN_POINT ( 'NONE',  ( 6.028125000614517504, -4.541064518000419881, 2.621784821874995952 ) ) ;
#23305 = CARTESIAN_POINT ( 'NONE',  ( 17.03437500061451715, 5.824947211148865298E-16, -4.756430356249998326 ) ) ;
#23306 = EDGE_CURVE ( 'NONE', #35963, #5936, #59092, .T. ) ;
#23307 = CARTESIAN_POINT ( 'NONE',  ( 2.737500001229034474, -4.330127018922194537, 2.499999999999995559 ) ) ;
#23308 = CARTESIAN_POINT ( 'NONE',  ( 14.88750000000000107, -2.886751345948125991, -5.000000000000000000 ) ) ;
#23309 = CARTESIAN_POINT ( 'NONE',  ( 15.42187500061451821, 3.027376345333611329, 5.243569643749999010 ) ) ;
#23310 = CARTESIAN_POINT ( 'NONE',  ( 12.07500000122903216, 2.886751345948126879, 4.999999999999999112 ) ) ;
#23311 = CARTESIAN_POINT ( 'NONE',  ( 18.34687500061451715, -3.027376345333610441, -5.243569643749999898 ) ) ;
#23312 = CARTESIAN_POINT ( 'NONE',  ( 16.72500000000000142, 6.123233995736764310E-16, -4.999999999999998224 ) ) ;
#23313 = CARTESIAN_POINT ( 'NONE',  ( 21.60937500061451644, 4.541064518000418104, -2.621784821874998173 ) ) ;
#23314 = CARTESIAN_POINT ( 'NONE',  ( 4.243569643749999010, 15.11562500061451608, -32.45002607614398471 ) ) ;
#23315 = CARTESIAN_POINT ( 'NONE',  ( 45.00000000000000000, 4.500000000000000888, -3.500000000000000000 ) ) ;
#23316 = CARTESIAN_POINT ( 'NONE',  ( 26.78437500061451360, -2.746126346562641984, -4.756430356249999214 ) ) ;
#23317 = CARTESIAN_POINT ( 'NONE',  ( 4.169580978743460342, 2.759455464706926708, 4.458747374224691029 ) ) ;
#23318 = CARTESIAN_POINT ( 'NONE',  ( 26.20312500061451644, 0.000000000000000000, 5.243569643749999010 ) ) ;
#23319 = DIRECTION ( 'NONE',  ( -1.000000000000000000, -0.000000000000000000, -0.000000000000000000 ) ) ;
#23320 = CARTESIAN_POINT ( 'NONE',  ( 27.94687500061451502, 6.054752690667223547, 3.707466751127219781E-16 ) ) ;
#23321 = EDGE_CURVE ( 'NONE', #21751, #71509, #17954, .T. ) ;
#23322 = CARTESIAN_POINT ( 'NONE',  ( 23.51249999999999574, 2.886751345948129099, -4.999999999999998224 ) ) ;
#23323 = CARTESIAN_POINT ( 'NONE',  ( 6.703125000614516438, 4.541064518000418104, -2.621784821874998173 ) ) ;
#23324 = CARTESIAN_POINT ( 'NONE',  ( 23.82187500061451502, 4.119189519843966529, 2.378215178124999607 ) ) ;
#23325 = CARTESIAN_POINT ( 'NONE',  ( 19.05937500061451928, 0.000000000000000000, 5.243569643749999010 ) ) ;
#23326 = CARTESIAN_POINT ( 'NONE',  ( 10.28437500061451715, 5.492252693125287522, 3.363034840372157021E-16 ) ) ;
#23327 = CARTESIAN_POINT ( 'NONE',  ( 5.915625000614515905, 3.027376345333611329, 5.243569643749999010 ) ) ;
#23328 = CARTESIAN_POINT ( 'NONE',  ( 11.85937500061451644, 0.000000000000000000, 5.243569643749999010 ) ) ;
#23329 = VERTEX_POINT ( 'NONE', #58932 ) ;
#23330 = CARTESIAN_POINT ( 'NONE',  ( 22.05937500061451573, 4.541064518000418104, -2.621784821874998173 ) ) ;
#23331 = CARTESIAN_POINT ( 'NONE',  ( 21.73125000122903216, 6.123233995736764310E-16, -4.999999999999998224 ) ) ;
#23332 = CARTESIAN_POINT ( 'NONE',  ( 29.09999999999999787, 0.000000000000000000, 4.999999999999998224 ) ) ;
#23333 = CARTESIAN_POINT ( 'NONE',  ( 28.80937500061451573, 4.541064518000418104, -2.621784821874998173 ) ) ;
#23334 = VECTOR ( 'NONE', #32395, 1000.000000000000000 ) ;
#23335 = FACE_OUTER_BOUND ( 'NONE', #35526, .T. ) ;
#23336 = CARTESIAN_POINT ( 'NONE',  ( 10.80000000000000071, -4.330127018922190985, -2.500000000000001332 ) ) ;
#23337 = VERTEX_POINT ( 'NONE', #40516 ) ;
#23338 = CARTESIAN_POINT ( 'NONE',  ( 11.10000000000000142, 0.000000000000000000, 4.999999999999998224 ) ) ;
#23339 = CARTESIAN_POINT ( 'NONE',  ( 11.63437500061451502, 5.492252693125287522, 3.363034840372157021E-16 ) ) ;
#23340 = CARTESIAN_POINT ( 'NONE',  ( 24.40312500061451573, 0.000000000000000000, 5.243569643749999010 ) ) ;
#23341 = CARTESIAN_POINT ( 'NONE',  ( 13.61250000000000071, 2.886751345948129099, -4.999999999999998224 ) ) ;
#23342 =( BOUNDED_CURVE ( )  B_SPLINE_CURVE ( 2, ( #34371, #17734, #11852, #12570, #35104, #52462, #52823 ),
 .UNSPECIFIED., .F., .F. ) 
 B_SPLINE_CURVE_WITH_KNOTS ( ( 3, 2, 2, 3 ),
 ( 0.009999999999999979391, 0.01333333333333330643, 0.01666666666666663174, 0.01999999999999995878 ),
 .UNSPECIFIED. ) 
 CURVE ( )  GEOMETRIC_REPRESENTATION_ITEM ( )  RATIONAL_B_SPLINE_CURVE ( ( 1.000000000000000888, 0.8660254037844378194, 1.000000000000000000, 0.8660254037844387076, 1.000000000000000000, 0.8660254037844403729, 0.9999999999999983347 ) ) 
 REPRESENTATION_ITEM ( '' )  );
#23343 = CARTESIAN_POINT ( 'NONE',  ( 10.12500000122903465, 2.886751345948129099, -4.999999999999998224 ) ) ;
#23344 = CARTESIAN_POINT ( 'NONE',  ( 8.728125000614518569, -4.541064518000419881, 2.621784821874995952 ) ) ;
#23345 = CARTESIAN_POINT ( 'NONE',  ( 24.00000000000000000, 4.330127018922192761, -2.499999999999997780 ) ) ;
#23346 = CARTESIAN_POINT ( 'NONE',  ( 20.31562500061451715, 3.027376345333611329, 5.243569643749999010 ) ) ;
#23347 = DIRECTION ( 'NONE',  ( 0.000000000000000000, 0.000000000000000000, -1.000000000000000000 ) ) ;
#23348 = CARTESIAN_POINT ( 'NONE',  ( 28.31250000122903288, 0.000000000000000000, 4.999999999999998224 ) ) ;
#23349 = CARTESIAN_POINT ( 'NONE',  ( 1.878215178124997609, 16.16562499938548569, 33.25316411605952993 ) ) ;
#23350 = CARTESIAN_POINT ( 'NONE',  ( 6.750000000000002665, -4.330127018922190985, -2.500000000000001332 ) ) ;
#23351 = VERTEX_POINT ( 'NONE', #8339 ) ;
#23352 = CARTESIAN_POINT ( 'NONE',  ( 20.87812500061451715, -4.541064518000419881, 2.621784821874995952 ) ) ;
#23353 = CARTESIAN_POINT ( 'NONE',  ( 29.16562500061451502, 3.027376345333613106, -5.243569643749998122 ) ) ;
#23354 = DIRECTION ( 'NONE',  ( -1.000000000000000000, -0.000000000000000000, -0.000000000000000000 ) ) ;
#23355 = CARTESIAN_POINT ( 'NONE',  ( 18.53437500061451715, 4.541064518000418104, 2.621784821874999949 ) ) ;
#23356 = CARTESIAN_POINT ( 'NONE',  ( 16.00312500061451715, -4.541064518000417216, -2.621784821875001281 ) ) ;
#23357 = CARTESIAN_POINT ( 'NONE',  ( 1.626862140677534273E-15, 12.01250000000000107, 34.00000000000000000 ) ) ;
#23358 = CARTESIAN_POINT ( 'NONE',  ( 4.565625000614516260, 3.027376345333611329, 5.243569643749999010 ) ) ;
#23359 = CARTESIAN_POINT ( 'NONE',  ( 28.68750000122903288, 4.330127018922191873, 2.499999999999999556 ) ) ;
#23360 = CARTESIAN_POINT ( 'NONE',  ( 22.54687500061451644, 5.492252693125287522, 3.363034840372157021E-16 ) ) ;
#23361 = CARTESIAN_POINT ( 'NONE',  ( 18.36562500061451431, 3.027376345333612662, -5.243569643749998122 ) ) ;
#23362 = CARTESIAN_POINT ( 'NONE',  ( 3.999999999999999112, 13.92500000000000071, 30.00000000000000000 ) ) ;
#23363 = CARTESIAN_POINT ( 'NONE',  ( 3.825000001229032609, 2.886751345948129099, -4.999999999999998224 ) ) ;
#23364 = CARTESIAN_POINT ( 'NONE',  ( 13.92187500061451644, 3.027376345333613106, -5.243569643749998122 ) ) ;
#23365 = CARTESIAN_POINT ( 'NONE',  ( 12.83437500061451786, -4.541064518000419881, 2.621784821874995952 ) ) ;
#23366 = CARTESIAN_POINT ( 'NONE',  ( 19.99687500061451573, -3.027376345333614438, 5.243569643749998122 ) ) ;
#23367 = ORIENTED_EDGE ( 'NONE', *, *, #63206, .F. ) ;
#23368 = CARTESIAN_POINT ( 'NONE',  ( -5.798826918071312342, 8.147596131390990593, 28.40867891430389847 ) ) ;
#23369 = CARTESIAN_POINT ( 'NONE',  ( 24.81562500061451715, 3.027376345333611329, 5.243569643749999010 ) ) ;
#23370 = CARTESIAN_POINT ( 'NONE',  ( 17.85937500061451999, -4.541064518000417216, -2.621784821875001281 ) ) ;
#23371 = CARTESIAN_POINT ( 'NONE',  ( 23.20312500061451644, -4.541064518000417216, -2.621784821875001281 ) ) ;
#23372 = CARTESIAN_POINT ( 'NONE',  ( 30.00000000000000000, 0.000000000000000000, 0.000000000000000000 ) ) ;
#23373 = CARTESIAN_POINT ( 'NONE',  ( 3.999999999999999112, 15.72500000000000320, 30.00000000000000000 ) ) ;
#23374 = CARTESIAN_POINT ( 'NONE',  ( 28.90312500061451217, 0.000000000000000000, 5.243569643749999010 ) ) ;
#23375 = CARTESIAN_POINT ( 'NONE',  ( 10.20000000122903572, 5.773502691896255534, 3.535250795749688894E-16 ) ) ;
#23376 = CARTESIAN_POINT ( 'NONE',  ( 6.787500001229032520, -4.330127018922194537, 2.499999999999995559 ) ) ;
#23377 = CARTESIAN_POINT ( 'NONE',  ( -2.828200636599751609E-16, 19.88749999999999929, -34.61880215351700230 ) ) ;
#23378 = CARTESIAN_POINT ( 'NONE',  ( 28.05000000122903359, -2.886751345948125991, -5.000000000000000000 ) ) ;
#23379 = CARTESIAN_POINT ( 'NONE',  ( -3.999999999999999556, 19.38124999877096499, 27.69059892324149175 ) ) ;
#23380 = CARTESIAN_POINT ( 'NONE',  ( 16.10625000122903216, 0.000000000000000000, 4.999999999999998224 ) ) ;
#23381 = CARTESIAN_POINT ( 'NONE',  ( 8.784375000614518925, -4.541064518000419881, 2.621784821874995952 ) ) ;
#23382 = CARTESIAN_POINT ( 'NONE',  ( -3.137519842735245283E-14, 14.71250000000000213, -26.00000000000000711 ) ) ;
#23383 = CARTESIAN_POINT ( 'NONE',  ( 17.39062500061451644, -3.027376345333610441, -5.243569643749999898 ) ) ;
#23384 = CARTESIAN_POINT ( 'NONE',  ( 11.97187500061451892, -6.054752690667223547, -1.112240025338166033E-15 ) ) ;
#23385 = CARTESIAN_POINT ( 'NONE',  ( 28.57500000122903572, 2.886751345948129099, -4.999999999999998224 ) ) ;
#23386 = CARTESIAN_POINT ( 'NONE',  ( 19.80937500061451573, 4.541064518000418104, -2.621784821874998173 ) ) ;
#23387 = CARTESIAN_POINT ( 'NONE',  ( 8.409375000614518925, -4.541064518000417216, -2.621784821875001281 ) ) ;
#23388 = CARTESIAN_POINT ( 'NONE',  ( 3.928125000614516527, 6.421520780324663323E-16, -5.243569643749999010 ) ) ;
#23389 = EDGE_CURVE ( 'NONE', #45611, #55464, #35682, .T. ) ;
#23390 = CARTESIAN_POINT ( 'NONE',  ( 7.453125000614516438, -4.541064518000417216, -2.621784821875001281 ) ) ;
#23391 = CARTESIAN_POINT ( 'NONE',  ( 19.30312500061451786, 4.541064518000418104, -2.621784821874998173 ) ) ;
#23392 = ORIENTED_EDGE ( 'NONE', *, *, #37730, .T. ) ;
#23393 = CARTESIAN_POINT ( 'NONE',  ( 4.837500001229035895, 4.330127018922191873, 2.499999999999999556 ) ) ;
#23394 = CARTESIAN_POINT ( 'NONE',  ( 14.35312500061451679, 4.541064518000418104, -2.621784821874998173 ) ) ;
#23395 = CARTESIAN_POINT ( 'NONE',  ( 12.70312500061451821, 0.000000000000000000, 5.243569643749999010 ) ) ;
#23396 = CARTESIAN_POINT ( 'NONE',  ( 24.08437500061451786, -4.119189519843968306, 2.378215178124996054 ) ) ;
#23397 = CARTESIAN_POINT ( 'NONE',  ( 13.27500000000000213, 4.330127018922191873, 2.499999999999999556 ) ) ;
#23398 = CARTESIAN_POINT ( 'NONE',  ( 7.950000001229033053, 5.773502691896255534, 3.535250795749688894E-16 ) ) ;
#23399 = CARTESIAN_POINT ( 'NONE',  ( 6.665625000614515905, 3.027376345333613106, -5.243569643749998122 ) ) ;
#23400 =( BOUNDED_CURVE ( )  B_SPLINE_CURVE ( 2, ( #7712, #30246, #52779, #47238, #64217, #36151, #8078 ),
 .UNSPECIFIED., .F., .F. ) 
 B_SPLINE_CURVE_WITH_KNOTS ( ( 3, 2, 2, 3 ),
 ( 0.4750000000000000333, 0.4777777777777778567, 0.4805555555555556246, 0.4833333333333333925 ),
 .UNSPECIFIED. ) 
 CURVE ( )  GEOMETRIC_REPRESENTATION_ITEM ( )  RATIONAL_B_SPLINE_CURVE ( ( 0.9999999999999973355, 0.8660254037844413721, 1.000000000000000000, 0.8660254037844387076, 1.000000000000000000, 0.8660254037844360431, 1.000000000000002665 ) ) 
 REPRESENTATION_ITEM ( '' )  );
#23401 = CARTESIAN_POINT ( 'NONE',  ( 19.20000000122903572, 5.773502691896255534, 3.535250795749688894E-16 ) ) ;
#23402 = CARTESIAN_POINT ( 'NONE',  ( 24.75000000000000000, -4.330127018922190985, -2.500000000000001332 ) ) ;
#23403 = CARTESIAN_POINT ( 'NONE',  ( 2.121784821875001281, 11.45937500061451786, -26.32496088578401938 ) ) ;
#23404 = DIRECTION ( 'NONE',  ( 0.000000000000000000, 0.000000000000000000, -1.000000000000000000 ) ) ;
#23405 = CARTESIAN_POINT ( 'NONE',  ( 3.487500001229035362, 4.330127018922191873, 2.499999999999999556 ) ) ;
#23406 = ADVANCED_FACE ( 'NONE', ( #23870 ), #18313, .F. ) ;
#23407 = CARTESIAN_POINT ( 'NONE',  ( -1.071796769724475906, 11.35759618943233562, -34.00000000000000711 ) ) ;
#23408 = CARTESIAN_POINT ( 'NONE',  ( -1.071796769724475906, 13.15759618943233100, 25.99999999999999289 ) ) ;
#23409 = CARTESIAN_POINT ( 'NONE',  ( 18.68437500061451928, -4.541064518000419881, 2.621784821874995952 ) ) ;
#23410 = CARTESIAN_POINT ( 'NONE',  ( 30.00000000000000000, 6.123233995736764310E-16, -4.999999999999998224 ) ) ;
#23411 = CARTESIAN_POINT ( 'NONE',  ( 15.10312500061451502, -4.541064518000417216, -2.621784821875001281 ) ) ;
#23412 = CARTESIAN_POINT ( 'NONE',  ( 9.618750001229031454, 2.886751345948129099, -4.999999999999998224 ) ) ;
#23413 = DIRECTION ( 'NONE',  ( -0.000000000000000000, -1.000000000000000000, -0.000000000000000000 ) ) ;
#23414 = CARTESIAN_POINT ( 'NONE',  ( 29.78437500061451715, 4.541064518000418104, 2.621784821874999949 ) ) ;
#23415 = CARTESIAN_POINT ( 'NONE',  ( 26.07187500061451857, 3.027376345333613106, -5.243569643749998122 ) ) ;
#23416 = CARTESIAN_POINT ( 'NONE',  ( 19.02187500061451431, -4.119189519843968306, 2.378215178124996054 ) ) ;
#23417 = CARTESIAN_POINT ( 'NONE',  ( 12.02812500061451573, 6.421520780324663323E-16, -5.243569643749999010 ) ) ;
#23418 = CARTESIAN_POINT ( 'NONE',  ( 11.70937500061451608, 4.541064518000418104, -2.621784821874998173 ) ) ;
#23419 = ORIENTED_EDGE ( 'NONE', *, *, #47483, .F. ) ;
#23420 = CARTESIAN_POINT ( 'NONE',  ( 2.964777361493091679, -4.026176250088806086, -3.359304602455296607 ) ) ;
#23421 = CARTESIAN_POINT ( 'NONE',  ( 21.06562500061451715, 3.027376345333613106, -5.243569643749998122 ) ) ;
#23422 = CARTESIAN_POINT ( 'NONE',  ( 2.393811435568372112E-14, 18.63124999877096855, 34.00000000000000000 ) ) ;
#23423 = CARTESIAN_POINT ( 'NONE',  ( 20.32499999999999929, 6.123233995736764310E-16, -4.999999999999998224 ) ) ;
#23424 = EDGE_CURVE ( 'NONE', #40395, #493, #41597, .T. ) ;
#23425 = CARTESIAN_POINT ( 'NONE',  ( 10.16249999999999964, 2.886751345948126879, 4.999999999999999112 ) ) ;
#23426 = CARTESIAN_POINT ( 'NONE',  ( 20.92500000122903714, 2.886751345948129099, -4.999999999999998224 ) ) ;
#23427 = CARTESIAN_POINT ( 'NONE',  ( 15.02812500061451750, -4.541064518000419881, 2.621784821874995952 ) ) ;
#23428 = CARTESIAN_POINT ( 'NONE',  ( 10.02187500061451431, -4.119189519843968306, 2.378215178124996054 ) ) ;
#23429 = ORIENTED_EDGE ( 'NONE', *, *, #7307, .T. ) ;
#23430 = CARTESIAN_POINT ( 'NONE',  ( 18.52499999999999858, 6.123233995736764310E-16, -4.999999999999998224 ) ) ;
#23431 = CARTESIAN_POINT ( 'NONE',  ( 22.50000000000000000, -4.330127018922190985, -2.500000000000001332 ) ) ;
#23432 = CARTESIAN_POINT ( 'NONE',  ( 20.03437500061451715, -4.541064518000419881, 2.621784821874995952 ) ) ;
#23433 = CARTESIAN_POINT ( 'NONE',  ( 24.81562500061451715, 3.027376345333611329, 5.243569643749999010 ) ) ;
#23434 = ORIENTED_EDGE ( 'NONE', *, *, #56915, .F. ) ;
#23435 = CARTESIAN_POINT ( 'NONE',  ( -3.999999999999999112, 16.96250000122903145, 30.00000000000000000 ) ) ;
#23436 = CARTESIAN_POINT ( 'NONE',  ( 9.178125000614517859, -4.541064518000419881, 2.621784821874995952 ) ) ;
#23437 = CARTESIAN_POINT ( 'NONE',  ( -3.999999999999999112, 18.93124999877096570, 27.69059892324149530 ) ) ;
#23438 = CARTESIAN_POINT ( 'NONE',  ( 14.92500000000000071, 6.123233995736764310E-16, -4.999999999999998224 ) ) ;
#23439 = CARTESIAN_POINT ( 'NONE',  ( 4.243569643749999898, 16.42812500061451786, 30.00000000000000000 ) ) ;
#23440 = CARTESIAN_POINT ( 'NONE',  ( 29.65312500061451573, 4.541064518000418104, -2.621784821874998173 ) ) ;
#23441 = CARTESIAN_POINT ( 'NONE',  ( 1.878215178124997609, 13.91562499938548392, 33.25316411605952993 ) ) ;
#23442 = CARTESIAN_POINT ( 'NONE',  ( 27.04687500061451644, 6.054752690667223547, 3.707466751127219781E-16 ) ) ;
#23443 = ORIENTED_EDGE ( 'NONE', *, *, #71959, .T. ) ;
#23444 = CARTESIAN_POINT ( 'NONE',  ( 23.84062500061451928, 6.054752690667223547, 3.707466751127219781E-16 ) ) ;
#23445 = CARTESIAN_POINT ( 'NONE',  ( 24.75937500061451502, 4.541064518000418104, -2.621784821874998173 ) ) ;
#23446 = CARTESIAN_POINT ( 'NONE',  ( -3.000416591977282496E-16, 18.79062500061459318, -34.90005215228797653 ) ) ;
#23447 = CARTESIAN_POINT ( 'NONE',  ( 12.03749999999999964, -2.886751345948129988, 4.999999999999997335 ) ) ;
#23448 = CARTESIAN_POINT ( 'NONE',  ( 9.140625000614518214, -3.027376345333614438, 5.243569643749998122 ) ) ;
#23449 = CARTESIAN_POINT ( 'NONE',  ( 28.77187500061451431, 2.746126346562645981, -4.756430356249997438 ) ) ;
#23450 = CARTESIAN_POINT ( 'NONE',  ( 29.20312500061451644, 4.541064518000418104, -2.621784821874998173 ) ) ;
#23451 = CARTESIAN_POINT ( 'NONE',  ( 26.50312500061451360, 4.541064518000418104, -2.621784821874998173 ) ) ;
#23453 = EDGE_CURVE ( 'NONE', #29842, #46076, #30512, .T. ) ;
#23452 = CARTESIAN_POINT ( 'NONE',  ( 28.20937500061451431, 2.746126346562645981, -4.756430356249997438 ) ) ;
#23454 = CARTESIAN_POINT ( 'NONE',  ( 13.20937500061451786, 0.000000000000000000, 4.756430356249998326 ) ) ;
#23455 = CARTESIAN_POINT ( 'NONE',  ( 20.33437500061451786, 4.541064518000418104, 2.621784821874999949 ) ) ;
#23456 = CARTESIAN_POINT ( 'NONE',  ( -3.000416591977282496E-16, 12.99687500061451750, 25.09994784771203058 ) ) ;
#23457 = CARTESIAN_POINT ( 'NONE',  ( 20.25937500061451857, 4.541064518000418104, -2.621784821874998173 ) ) ;
#23458 = CARTESIAN_POINT ( 'NONE',  ( 26.78437500061451360, -4.541064518000419881, 2.621784821874995952 ) ) ;
#23459 = CARTESIAN_POINT ( 'NONE',  ( 2.121784821875001281, 16.40937500061452070, 33.67503911421598417 ) ) ;
#23460 = CARTESIAN_POINT ( 'NONE',  ( 6.553125000614518747, -4.541064518000417216, -2.621784821875001281 ) ) ;
#23461 = CARTESIAN_POINT ( 'NONE',  ( -2.556497649636125342E-15, 19.21250000000000213, 34.00000000000000000 ) ) ;
#23462 = CARTESIAN_POINT ( 'NONE',  ( 3.609375000614516882, 4.541064518000418104, -2.621784821874998173 ) ) ;
#23463 = DIRECTION ( 'NONE',  ( 0.000000000000000000, 0.000000000000000000, 1.000000000000000000 ) ) ;
#23464 = CARTESIAN_POINT ( 'NONE',  ( 5.690625000614516260, -3.027376345333610441, -5.243569643749999898 ) ) ;
#23465 = CARTESIAN_POINT ( 'NONE',  ( 9.121875000614517504, 3.027376345333611329, 5.243569643749999010 ) ) ;
#23466 =( NAMED_UNIT ( * ) PLANE_ANGLE_UNIT ( ) SI_UNIT ( $, .RADIAN. ) );
#23467 = CARTESIAN_POINT ( 'NONE',  ( 18.37500000122903288, 2.886751345948126879, 4.999999999999999112 ) ) ;
#23468 = CARTESIAN_POINT ( 'NONE',  ( 6.309375000614517504, 4.541064518000418104, -2.621784821874998173 ) ) ;
#23469 = CARTESIAN_POINT ( 'NONE',  ( 7.528125000614515727, 6.421520780324663323E-16, -5.243569643749999010 ) ) ;
#23470 = CARTESIAN_POINT ( 'NONE',  ( 4.844509297411973670, 1.237226603047926421, -5.095516945469514170 ) ) ;
#23471 = CARTESIAN_POINT ( 'NONE',  ( 22.81875000122903074, 2.886751345948126879, 4.999999999999999112 ) ) ;
#23472 = CARTESIAN_POINT ( 'NONE',  ( 17.82187500061451502, -6.054752690667223547, -1.112240025338166033E-15 ) ) ;
#23473 = CARTESIAN_POINT ( 'NONE',  ( 0.000000000000000000, 20.00000000000000000, -30.00000000000000000 ) ) ;
#23474 = VERTEX_POINT ( 'NONE', #64484 ) ;
#23475 = CARTESIAN_POINT ( 'NONE',  ( 24.21562500061451573, 3.027376345333613106, -5.243569643749998122 ) ) ;
#23476 = CARTESIAN_POINT ( 'NONE',  ( 10.82812500061451644, 4.541064518000418104, 2.621784821874999949 ) ) ;
#23477 = CARTESIAN_POINT ( 'NONE',  ( 26.52187500061451431, 3.027376345333612662, -5.243569643749998122 ) ) ;
#23478 = CARTESIAN_POINT ( 'NONE',  ( 10.56562500061451715, -6.054752690667223547, -1.112240025338166033E-15 ) ) ;
#23479 = CARTESIAN_POINT ( 'NONE',  ( 4.243569643749999898, 10.63437500061451857, -30.00000000000000000 ) ) ;
#23480 = CARTESIAN_POINT ( 'NONE',  ( 13.08750000122903323, -4.330127018922194537, 2.499999999999995559 ) ) ;
#23481 = CARTESIAN_POINT ( 'NONE',  ( 26.46562500061451573, 3.027376345333613106, -5.243569643749998122 ) ) ;
#23482 = CARTESIAN_POINT ( 'NONE',  ( 4.243569643749999898, 11.92812500061451608, -30.00000000000000000 ) ) ;
#23483 = CARTESIAN_POINT ( 'NONE',  ( 13.53750000122903430, -4.330127018922194537, 2.499999999999995559 ) ) ;
#23484 = CARTESIAN_POINT ( 'NONE',  ( 11.10000000000000142, 0.000000000000000000, 4.999999999999998224 ) ) ;
#23485 = CARTESIAN_POINT ( 'NONE',  ( 21.21562500061451573, 3.027376345333611329, 5.243569643749999010 ) ) ;
#23486 = CARTESIAN_POINT ( 'NONE',  ( 5.709375000614517859, -4.541064518000417216, -2.621784821875001281 ) ) ;
#23487 = CARTESIAN_POINT ( 'NONE',  ( 19.57500000000000284, 4.330127018922191873, 2.499999999999999556 ) ) ;
#23488 = CARTESIAN_POINT ( 'NONE',  ( 9.000000001229034652, -2.886751345948129988, 4.999999999999997335 ) ) ;
#23489 = CARTESIAN_POINT ( 'NONE',  ( 16.91250000122903430, 4.330127018922192761, -2.499999999999997780 ) ) ;
#23490 = CARTESIAN_POINT ( 'NONE',  ( 13.30312500061451786, -4.541064518000417216, -2.621784821875001281 ) ) ;
#23491 = CARTESIAN_POINT ( 'NONE',  ( 15.74062500061451608, 6.054752690667223547, 3.707466751127219781E-16 ) ) ;
#23492 = CARTESIAN_POINT ( 'NONE',  ( 26.81250000122903288, 4.330127018922192761, -2.499999999999997780 ) ) ;
#23493 = CARTESIAN_POINT ( 'NONE',  ( 19.98749999999999716, 5.773502691896255534, 3.535250795749688894E-16 ) ) ;
#23494 = CARTESIAN_POINT ( 'NONE',  ( 23.59687500061451715, -3.027376345333614438, 5.243569643749998122 ) ) ;
#23495 = CARTESIAN_POINT ( 'NONE',  ( 22.29375000122903216, 5.773502691896255534, 3.535250795749688401E-16 ) ) ;
#23496 = CARTESIAN_POINT ( 'NONE',  ( 10.35000000122903074, -2.886751345948129988, 4.999999999999997335 ) ) ;
#23497 = CARTESIAN_POINT ( 'NONE',  ( 9.496875000614517504, 6.054752690667223547, 3.707466751127219781E-16 ) ) ;
#23498 = CARTESIAN_POINT ( 'NONE',  ( 25.62187500061451573, 3.027376345333613106, -5.243569643749998122 ) ) ;
#23499 = CARTESIAN_POINT ( 'NONE',  ( 3.721875000614518036, 3.027376345333611329, 5.243569643749999010 ) ) ;
#23500 = CARTESIAN_POINT ( 'NONE',  ( 24.17812500061451786, 6.421520780324663323E-16, -5.243569643749999010 ) ) ;
#23501 = CARTESIAN_POINT ( 'NONE',  ( 26.25937500061451857, 0.000000000000000000, 5.243569643749999010 ) ) ;
#23502 = CARTESIAN_POINT ( 'NONE',  ( 2.655984681222220721E-16, 17.36562499938548498, 25.66244784525396483 ) ) ;
#23503 = CARTESIAN_POINT ( 'NONE',  ( 3.193392017337676414, -3.847432258030384578, 3.242174253483891544 ) ) ;
#23504 = CARTESIAN_POINT ( 'NONE',  ( 6.909375000614518036, 0.000000000000000000, 5.243569643749999010 ) ) ;
#23505 = CARTESIAN_POINT ( 'NONE',  ( -1.394453263437886801E-15, 19.32500000122903216, 33.99999999999999289 ) ) ;
#23506 = CARTESIAN_POINT ( 'NONE',  ( 28.22812500061451502, 6.421520780324663323E-16, -5.243569643749999010 ) ) ;
#23507 = CARTESIAN_POINT ( 'NONE',  ( 6.534375000614517148, -4.541064518000419881, 2.621784821874995952 ) ) ;
#23508 = CARTESIAN_POINT ( 'NONE',  ( 25.72499999999999787, 6.123233995736764310E-16, -4.999999999999998224 ) ) ;
#23509 = CARTESIAN_POINT ( 'NONE',  ( 11.17500000000000071, -4.330127018922194537, 2.499999999999995559 ) ) ;
#23510 = CARTESIAN_POINT ( 'NONE',  ( 18.26249999999999929, 2.886751345948126879, 4.999999999999999112 ) ) ;
#23511 = VERTEX_POINT ( 'NONE', #29426 ) ;
#23512 = CARTESIAN_POINT ( 'NONE',  ( 27.86249999999999716, -5.773502691896255534, -1.060575238724906372E-15 ) ) ;
#23513 = CARTESIAN_POINT ( 'NONE',  ( 29.07187500061451502, -6.054752690667223547, -1.112240025338166033E-15 ) ) ;
#23514 = ORIENTED_EDGE ( 'NONE', *, *, #4619, .T. ) ;
#23515 = CARTESIAN_POINT ( 'NONE',  ( 15.66562500061451857, 3.027376345333613106, -5.243569643749998122 ) ) ;
#23516 = CARTESIAN_POINT ( 'NONE',  ( 6.553125000614518747, -4.541064518000417216, -2.621784821875001281 ) ) ;
#23517 = CARTESIAN_POINT ( 'NONE',  ( 19.73437500061451289, 5.492252693125287522, 3.363034840372157021E-16 ) ) ;
#23518 = CARTESIAN_POINT ( 'NONE',  ( 4.771875000614516971, -6.054752690667223547, -1.112240025338166033E-15 ) ) ;
#23519 = CARTESIAN_POINT ( 'NONE',  ( 14.81250000122903288, 0.000000000000000000, 4.999999999999998224 ) ) ;
#23520 = CARTESIAN_POINT ( 'NONE',  ( 21.41250000000000497, 2.886751345948126879, 4.999999999999999112 ) ) ;
#23521 = CARTESIAN_POINT ( 'NONE',  ( 29.43750000000000000, 5.773502691896255534, 3.535250795749688894E-16 ) ) ;
#23522 = CARTESIAN_POINT ( 'NONE',  ( 4.321875000614517681, -6.054752690667223547, -1.112240025338166033E-15 ) ) ;
#23523 = CARTESIAN_POINT ( 'NONE',  ( 8.184375000614515727, 4.541064518000418104, 2.621784821874999949 ) ) ;
#23524 = CARTESIAN_POINT ( 'NONE',  ( 20.89687500061452141, -3.027376345333614438, 5.243569643749998122 ) ) ;
#23525 = CARTESIAN_POINT ( 'NONE',  ( 4.898587196589411843E-16, 20.00000000000000000, 33.99999999999999289 ) ) ;
#23526 = ORIENTED_EDGE ( 'NONE', *, *, #27624, .F. ) ;
#23527 = CARTESIAN_POINT ( 'NONE',  ( 2.971875000614517592, -6.054752690667223547, -1.112240025338166033E-15 ) ) ;
#23528 = CARTESIAN_POINT ( 'NONE',  ( 5.512499999999999289, 2.886751345948129099, -4.999999999999998224 ) ) ;
#23529 = CARTESIAN_POINT ( 'NONE',  ( 6.384375000614516793, 4.541064518000418104, 2.621784821874999949 ) ) ;
#23530 = CARTESIAN_POINT ( 'NONE',  ( 18.63749999999999929, 5.773502691896255534, 3.535250795749688894E-16 ) ) ;
#23531 = CARTESIAN_POINT ( 'NONE',  ( 15.59062500061451573, -3.027376345333610441, -5.243569643749999898 ) ) ;
#23532 = CARTESIAN_POINT ( 'NONE',  ( 1.999999999999997335, 19.62500000000000000, 33.46410161513775705 ) ) ;
#23533 = CARTESIAN_POINT ( 'NONE',  ( 4.169580978743460342, 2.759455464706926708, 4.458747374224691029 ) ) ;
#23534 = CARTESIAN_POINT ( 'NONE',  ( 20.37187500061451573, 2.746126346562643317, 4.756430356249998326 ) ) ;
#23535 = CARTESIAN_POINT ( 'NONE',  ( 10.22812500061451679, 6.421520780324663323E-16, -5.243569643749999010 ) ) ;
#23536 = CARTESIAN_POINT ( 'NONE',  ( 27.23437500061451644, -4.541064518000419881, 2.621784821874995952 ) ) ;
#23537 = CARTESIAN_POINT ( 'NONE',  ( 2.121784821875001281, 19.55937500061451573, 33.67503911421598417 ) ) ;
#23538 = CARTESIAN_POINT ( 'NONE',  ( 26.85937500061451644, -4.541064518000417216, -2.621784821875001281 ) ) ;
#23539 = CARTESIAN_POINT ( 'NONE',  ( 7.612500000000000711, -5.773502691896255534, -1.060575238724906372E-15 ) ) ;
#23540 = CARTESIAN_POINT ( 'NONE',  ( -3.999999999999999112, 13.36250000122903359, 30.00000000000000000 ) ) ;
#23541 = CARTESIAN_POINT ( 'NONE',  ( 14.42812500061451786, 4.541064518000418104, 2.621784821874999949 ) ) ;
#23542 = CARTESIAN_POINT ( 'NONE',  ( 7.575000001229033053, 2.886751345948126879, 4.999999999999999112 ) ) ;
#23543 = CARTESIAN_POINT ( 'NONE',  ( 18.34687500061451715, -3.027376345333610441, -5.243569643749999898 ) ) ;
#23544 = CARTESIAN_POINT ( 'NONE',  ( 12.45937500061451786, -4.541064518000417216, -2.621784821875001281 ) ) ;
#23545 = CARTESIAN_POINT ( 'NONE',  ( 4.898587196589411843E-16, 20.00000000000000000, -26.00000000000000000 ) ) ;
#23546 = ORIENTED_EDGE ( 'NONE', *, *, #20108, .F. ) ;
#23547 = CARTESIAN_POINT ( 'NONE',  ( 14.12812500061451715, -4.541064518000419881, 2.621784821874995952 ) ) ;
#23548 = CARTESIAN_POINT ( 'NONE',  ( 26.32500000122903216, 2.886751345948129099, -4.999999999999998224 ) ) ;
#23549 = CARTESIAN_POINT ( 'NONE',  ( 13.35937500061451821, -4.541064518000417216, -2.621784821875001281 ) ) ;
#23550 = CIRCLE ( 'NONE', #61307, 14.99999999999999822 ) ;
#23551 = DIRECTION ( 'NONE',  ( -1.000000000000000000, -0.000000000000000000, -0.000000000000000000 ) ) ;
#23552 = CARTESIAN_POINT ( 'NONE',  ( 15.06562500061451537, -6.054752690667223547, -1.112240025338166033E-15 ) ) ;
#23553 = DIRECTION ( 'NONE',  ( -0.000000000000000000, -0.000000000000000000, -1.000000000000000000 ) ) ;
#23554 = CARTESIAN_POINT ( 'NONE',  ( 23.93437500061451573, 4.541064518000418104, 2.621784821874999949 ) ) ;
#23555 = CARTESIAN_POINT ( 'NONE',  ( -1.473776270879187500, 9.816672227264547246, 25.95083297442941017 ) ) ;
#23556 = EDGE_CURVE ( 'NONE', #18169, #9094, #56005, .T. ) ;
#23557 = CARTESIAN_POINT ( 'NONE',  ( 10.98750000122903536, 6.123233995736764310E-16, -4.999999999999998224 ) ) ;
#23558 = CARTESIAN_POINT ( 'NONE',  ( 7.696875000614516793, 5.492252693125287522, 3.363034840372157021E-16 ) ) ;
#23559 = CARTESIAN_POINT ( 'NONE',  ( 20.66250000122903074, 0.000000000000000000, 4.999999999999998224 ) ) ;
#23560 = CARTESIAN_POINT ( 'NONE',  ( 2.121784821875001281, 17.30937500061451573, -26.32496088578401938 ) ) ;
#23561 =( BOUNDED_CURVE ( )  B_SPLINE_CURVE ( 2, ( #60780, #10912, #38999, #48988, #67083, #66335, #55983 ),
 .UNSPECIFIED., .F., .F. ) 
 B_SPLINE_CURVE_WITH_KNOTS ( ( 3, 2, 2, 3 ),
 ( 0.8166666666666666519, 0.8194444444444444198, 0.8222222222222222987, 0.8250000000000000666 ),
 .UNSPECIFIED. ) 
 CURVE ( )  GEOMETRIC_REPRESENTATION_ITEM ( )  RATIONAL_B_SPLINE_CURVE ( ( 1.000000000000000000, 0.8660254037844387076, 1.000000000000000000, 0.8660254037844387076, 1.000000000000000000, 0.8660254037844333785, 1.000000000000005329 ) ) 
 REPRESENTATION_ITEM ( '' )  );
#23562 = CARTESIAN_POINT ( 'NONE',  ( 17.37187500061451573, -6.054752690667223547, -1.112240025338166033E-15 ) ) ;
#23563 = CARTESIAN_POINT ( 'NONE',  ( 19.76250000122903216, 0.000000000000000000, 4.999999999999998224 ) ) ;
#23564 = ADVANCED_FACE ( 'NONE', ( #63400 ), #12785, .F. ) ;
#23565 = CARTESIAN_POINT ( 'NONE',  ( 15.79687500061451821, 6.054752690667223547, 3.707466751127219781E-16 ) ) ;
#23566 = CARTESIAN_POINT ( 'NONE',  ( 4.243569643749999898, 10.18437500061451750, 30.00000000000000000 ) ) ;
#23567 = CARTESIAN_POINT ( 'NONE',  ( 19.01250000122903216, -4.330127018922190985, -2.500000000000001332 ) ) ;
#23568 = CARTESIAN_POINT ( 'NONE',  ( 15.21562500061451750, 3.027376345333613106, -5.243569643749998122 ) ) ;
#23569 = CARTESIAN_POINT ( 'NONE',  ( 29.57812500061451644, 6.421520780324663323E-16, -5.243569643749999010 ) ) ;
#23570 = VERTEX_POINT ( 'NONE', #18678 ) ;
#23571 = EDGE_LOOP ( 'NONE', ( #32221, #47998, #9586, #64772 ) ) ;
#23572 = CARTESIAN_POINT ( 'NONE',  ( 18.33749999999999858, -2.886751345948129988, 4.999999999999997335 ) ) ;
#23573 = CARTESIAN_POINT ( 'NONE',  ( 5.810221930991193690E-16, 14.41249999999999787, 26.00000000000000000 ) ) ;
#23574 = CARTESIAN_POINT ( 'NONE',  ( 2.485350534231654862, 4.344988454211105022, 33.14460541871455490 ) ) ;
#23575 = CARTESIAN_POINT ( 'NONE',  ( 15.75000000122902932, -2.886751345948129988, 4.999999999999997335 ) ) ;
#23576 = CARTESIAN_POINT ( 'NONE',  ( 27.72187500061451715, -6.054752690667223547, -1.112240025338166033E-15 ) ) ;
#23577 = CARTESIAN_POINT ( 'NONE',  ( 20.46562500061451928, -6.054752690667223547, -1.112240025338166033E-15 ) ) ;
#23578 = CARTESIAN_POINT ( 'NONE',  ( 21.96562500061451573, 3.027376345333613106, -5.243569643749998122 ) ) ;
#23579 = CARTESIAN_POINT ( 'NONE',  ( 3.590625000614518836, 6.054752690667223547, 3.707466751127219781E-16 ) ) ;
#23580 = CARTESIAN_POINT ( 'NONE',  ( 28.04999999999999716, 4.330127018922192761, -2.499999999999997780 ) ) ;
#23581 = CARTESIAN_POINT ( 'NONE',  ( 4.000000000000000000, 11.75000000122903643, 32.30940107675849760 ) ) ;
#23582 = CARTESIAN_POINT ( 'NONE',  ( 8.784375000614518925, -4.119189519843968306, 2.378215178124996054 ) ) ;
#23583 = CARTESIAN_POINT ( 'NONE',  ( 11.15625000122903288, 0.000000000000000000, 4.999999999999998224 ) ) ;
#23584 = CARTESIAN_POINT ( 'NONE',  ( -3.999999999999997335, 12.50000000122903465, -27.69059892324149175 ) ) ;
#23585 = CARTESIAN_POINT ( 'NONE',  ( -4.243569643749999898, 16.67187500061451644, -32.45002607614398471 ) ) ;
#23586 = CARTESIAN_POINT ( 'NONE',  ( 5.100000001229034297, -2.886751345948125991, -5.000000000000000000 ) ) ;
#23587 = CARTESIAN_POINT ( 'NONE',  ( 5.062500000000000888, 2.886751345948129099, -4.999999999999998224 ) ) ;
#23588 = CARTESIAN_POINT ( 'NONE',  ( 3.337500001229034563, 6.123233995736764310E-16, -4.999999999999998224 ) ) ;
#23589 = CARTESIAN_POINT ( 'NONE',  ( 9.909375000614517148, 4.541064518000418104, -2.621784821874998173 ) ) ;
#23590 = CARTESIAN_POINT ( 'NONE',  ( 23.81250000122903288, 0.000000000000000000, 4.999999999999998224 ) ) ;
#23591 = CYLINDRICAL_SURFACE ( 'NONE', #68081, 4.999999999999998224 ) ;
#23592 = FACE_OUTER_BOUND ( 'NONE', #7733, .T. ) ;
#23593 = CARTESIAN_POINT ( 'NONE',  ( -1.071796769724490561, 19.57009619066136707, -34.00000000000000000 ) ) ;
#23594 = CARTESIAN_POINT ( 'NONE',  ( 6.609375000614519102, -4.541064518000417216, -2.621784821875001281 ) ) ;
#23595 = CARTESIAN_POINT ( 'NONE',  ( 12.45937500061451786, -4.541064518000417216, -2.621784821875001281 ) ) ;
#23596 = CARTESIAN_POINT ( 'NONE',  ( 5.587500000000003020, 5.773502691896255534, 3.535250795749688894E-16 ) ) ;
#23597 =( BOUNDED_CURVE ( )  B_SPLINE_CURVE ( 2, ( #35631, #46731, #2034, #24545, #953, #63702, #69623, #13093, #58152 ),
 .UNSPECIFIED., .F., .F. ) 
 B_SPLINE_CURVE_WITH_KNOTS ( ( 3, 2, 2, 2, 3 ),
 ( 0.3586956521739130821, 0.3623188405797101441, 0.3695652173913043237, 0.3768115942028985588, 0.3804347826086956763 ),
 .UNSPECIFIED. ) 
 CURVE ( )  GEOMETRIC_REPRESENTATION_ITEM ( )  RATIONAL_B_SPLINE_CURVE ( ( 0.9330127018922194093, 0.9330127018922198534, 1.000000000000000000, 0.8660254037844387076, 1.000000000000000000, 0.8660254037844387076, 1.000000000000000000, 0.9330127018922188542, 0.9330127018922194093 ) ) 
 REPRESENTATION_ITEM ( '' )  );
#23598 = CARTESIAN_POINT ( 'NONE',  ( -4.243569643749999898, 17.51562500061459460, 27.54997392385601529 ) ) ;
#23599 = CARTESIAN_POINT ( 'NONE',  ( 21.42187500061451644, -6.054752690667223547, -1.112240025338166033E-15 ) ) ;
#23600 = DIRECTION ( 'NONE',  ( 0.000000000000000000, 0.000000000000000000, -1.000000000000000000 ) ) ;
#23601 = CARTESIAN_POINT ( 'NONE',  ( 26.51250000122903216, 0.000000000000000000, 4.999999999999998224 ) ) ;
#23602 = CARTESIAN_POINT ( 'NONE',  ( 16.73437500061451644, -2.746126346562646425, 4.756430356249996549 ) ) ;
#23603 = CARTESIAN_POINT ( 'NONE',  ( 22.19062500061451715, -3.027376345333614438, 5.243569643749998122 ) ) ;
#23604 = CARTESIAN_POINT ( 'NONE',  ( 13.67812500061451786, -4.541064518000419881, 2.621784821874995952 ) ) ;
#23605 = CARTESIAN_POINT ( 'NONE',  ( 27.23437500061450933, -2.746126346562642428, -4.756430356249999214 ) ) ;
#23606 = CARTESIAN_POINT ( 'NONE',  ( 11.37187500061451750, 3.027376345333611329, 5.243569643749999010 ) ) ;
#23607 = CARTESIAN_POINT ( 'NONE',  ( 28.19999999999999929, 0.000000000000000000, 4.999999999999998224 ) ) ;
#23608 = CARTESIAN_POINT ( 'NONE',  ( 21.52500000122903145, 2.886751345948126879, 4.999999999999999112 ) ) ;
#23609 = CARTESIAN_POINT ( 'NONE',  ( 28.87499999999999645, 6.123233995736764310E-16, -4.999999999999998224 ) ) ;
#23610 = CARTESIAN_POINT ( 'NONE',  ( 12.45937500061451786, -4.541064518000417216, -2.621784821875001281 ) ) ;
#23611 = CARTESIAN_POINT ( 'NONE',  ( 28.10625000122902861, 4.330127018922192761, -2.499999999999997780 ) ) ;
#23612 = CARTESIAN_POINT ( 'NONE',  ( 34.99999999999999289, -3.142333204958820020E-14, -9.000000000000000000 ) ) ;
#23613 = CARTESIAN_POINT ( 'NONE',  ( 22.92187500061451644, 3.027376345333613106, -5.243569643749998122 ) ) ;
#23614 = CARTESIAN_POINT ( 'NONE',  ( 13.13437500061451857, 4.541064518000418104, 2.621784821874999949 ) ) ;
#23615 = CARTESIAN_POINT ( 'NONE',  ( 2.655984681222220721E-16, 18.71562499938548285, 25.66244784525396483 ) ) ;
#23616 = CARTESIAN_POINT ( 'NONE',  ( 25.50000000000000000, 0.000000000000000000, 4.999999999999998224 ) ) ;
#23617 = CARTESIAN_POINT ( 'NONE',  ( 2.828200636599751609E-16, 13.51250000000000107, 25.38119784648299415 ) ) ;
#23618 = CARTESIAN_POINT ( 'NONE',  ( 26.59687500061451360, 5.492252693125287522, 3.363034840372157021E-16 ) ) ;
#23619 = CARTESIAN_POINT ( 'NONE',  ( 16.94062500061451715, -3.027376345333610441, -5.243569643749999898 ) ) ;
#23620 = CARTESIAN_POINT ( 'NONE',  ( 6.637500000000001066, -2.886751345948129988, 4.999999999999997335 ) ) ;
#23621 = CARTESIAN_POINT ( 'NONE',  ( 3.999999999999998668, 13.62500000122903465, 27.69059892324149530 ) ) ;
#23622 = CARTESIAN_POINT ( 'NONE',  ( 14.88750000000000107, -2.886751345948125991, -5.000000000000000000 ) ) ;
#23623 = CARTESIAN_POINT ( 'NONE',  ( 2.121784821875001281, 11.40312500061451750, 33.67503911421598417 ) ) ;
#23624 =( BOUNDED_CURVE ( )  B_SPLINE_CURVE ( 2, ( #4114, #15532, #54711, #27735, #21810, #16268, #38823, #10007, #49541 ),
 .UNSPECIFIED., .F., .F. ) 
 B_SPLINE_CURVE_WITH_KNOTS ( ( 3, 2, 2, 2, 3 ),
 ( 0.2500000000000000000, 0.2536231884057971175, 0.2608695652173912971, 0.2681159420289855322, 0.2717391304347826497 ),
 .UNSPECIFIED. ) 
 CURVE ( )  GEOMETRIC_REPRESENTATION_ITEM ( )  RATIONAL_B_SPLINE_CURVE ( ( 0.9330127018922194093, 0.9330127018922190762, 1.000000000000000000, 0.8660254037844387076, 1.000000000000000000, 0.8660254037844387076, 1.000000000000000000, 0.9330127018922188542, 0.9330127018922194093 ) ) 
 REPRESENTATION_ITEM ( '' )  );
#23625 = CARTESIAN_POINT ( 'NONE',  ( 45.00000000000000000, 0.000000000000000000, 0.000000000000000000 ) ) ;
#23626 = CARTESIAN_POINT ( 'NONE',  ( 23.59687500061451715, -3.027376345333614438, 5.243569643749998122 ) ) ;
#23627 = VERTEX_POINT ( 'NONE', #41241 ) ;
#23628 = CARTESIAN_POINT ( 'NONE',  ( 21.51562500061451644, 3.027376345333613106, -5.243569643749998122 ) ) ;
#23629 = CARTESIAN_POINT ( 'NONE',  ( 20.97187500061451715, -6.054752690667223547, -1.112240025338166033E-15 ) ) ;
#23630 = CARTESIAN_POINT ( 'NONE',  ( 4.724999999999999645, 4.330127018922191873, 2.499999999999999556 ) ) ;
#23631 = CARTESIAN_POINT ( 'NONE',  ( 6.178125000614518747, 6.421520780324663323E-16, -5.243569643749999010 ) ) ;
#23632 = CARTESIAN_POINT ( 'NONE',  ( 21.10312500061451502, 4.541064518000418104, -2.621784821874998173 ) ) ;
#23633 = CARTESIAN_POINT ( 'NONE',  ( 12.27187500061451786, 3.027376345333611329, 5.243569643749999010 ) ) ;
#23634 = CARTESIAN_POINT ( 'NONE',  ( 16.99687500061451573, -3.027376345333610441, -5.243569643749999898 ) ) ;
#23635 = CARTESIAN_POINT ( 'NONE',  ( -2.121784821874996840, 17.62812500061451715, 33.67503911421598417 ) ) ;
#23636 = CARTESIAN_POINT ( 'NONE',  ( 19.31250000122903288, 0.000000000000000000, 4.999999999999998224 ) ) ;
#23637 = CARTESIAN_POINT ( 'NONE',  ( 14.48437500061451821, 4.119189519843966529, 2.378215178124999607 ) ) ;
#23638 = CARTESIAN_POINT ( 'NONE',  ( 10.19062500061451715, -3.027376345333610441, -5.243569643749999898 ) ) ;
#23639 = CARTESIAN_POINT ( 'NONE',  ( 5.446875000614518569, 6.054752690667223547, 3.707466751127219781E-16 ) ) ;
#23640 = CARTESIAN_POINT ( 'NONE',  ( 5.746875000614517504, -3.027376345333610441, -5.243569643749999898 ) ) ;
#23641 = CARTESIAN_POINT ( 'NONE',  ( 25.99687500061451928, -3.027376345333610441, -5.243569643749999898 ) ) ;
#23642 = CARTESIAN_POINT ( 'NONE',  ( 16.75312500061451715, 0.000000000000000000, 5.243569643749999010 ) ) ;
#23643 = CARTESIAN_POINT ( 'NONE',  ( 27.45000000122903572, -2.886751345948129988, 4.999999999999997335 ) ) ;
#23644 = EDGE_CURVE ( 'NONE', #46924, #26808, #7608, .T. ) ;
#23645 = CARTESIAN_POINT ( 'NONE',  ( 24.47812500061451502, -4.541064518000419881, 2.621784821874995952 ) ) ;
#23646 = CARTESIAN_POINT ( 'NONE',  ( 22.35937500061451644, -4.541064518000417216, -2.621784821875001281 ) ) ;
#23647 = CARTESIAN_POINT ( 'NONE',  ( 17.72812500061451502, -4.541064518000419881, 2.621784821874995952 ) ) ;
#23648 = CARTESIAN_POINT ( 'NONE',  ( -3.000416591977282496E-16, 17.49687500061451573, 25.09994784771203058 ) ) ;
#23649 =( BOUNDED_CURVE ( )  B_SPLINE_CURVE ( 2, ( #48134, #36675, #65483, #9342, #24854, #26331, #64382, #30411, #25597 ),
 .UNSPECIFIED., .F., .F. ) 
 B_SPLINE_CURVE_WITH_KNOTS ( ( 3, 2, 2, 2, 3 ),
 ( 0.4891304347826087029, 0.4927536231884058204, 0.5000000000000000000, 0.5072463768115942351, 0.5108695652173913526 ),
 .UNSPECIFIED. ) 
 CURVE ( )  GEOMETRIC_REPRESENTATION_ITEM ( )  RATIONAL_B_SPLINE_CURVE ( ( 0.9330127018922194093, 0.9330127018922194093, 1.000000000000000000, 0.8660254037844387076, 1.000000000000000000, 0.8660254037844387076, 1.000000000000000000, 0.9330127018922182991, 0.9330127018922192983 ) ) 
 REPRESENTATION_ITEM ( '' )  );
#23650 = CARTESIAN_POINT ( 'NONE',  ( 21.32812500061451644, -4.541064518000419881, 2.621784821874995952 ) ) ;
#23651 = CARTESIAN_POINT ( 'NONE',  ( 11.38125000122903252, 6.123233995736764310E-16, -4.999999999999998224 ) ) ;
#23652 = ORIENTED_EDGE ( 'NONE', *, *, #17853, .F. ) ;
#23653 = CARTESIAN_POINT ( 'NONE',  ( 25.46249999999999858, 2.886751345948126879, 4.999999999999999112 ) ) ;
#23654 = CARTESIAN_POINT ( 'NONE',  ( 8.484601909799253346E-16, 12.91249999999999964, -25.38119784648299770 ) ) ;
#23655 = CARTESIAN_POINT ( 'NONE',  ( -3.756430356250000102, 20.62812499938548072, 30.00000000000000000 ) ) ;
#23656 = CARTESIAN_POINT ( 'NONE',  ( 29.76562500061451644, 3.027376345333611329, 5.243569643749999010 ) ) ;
#23657 = CARTESIAN_POINT ( 'NONE',  ( 10.60312500061451679, -4.541064518000417216, -2.621784821875001281 ) ) ;
#23658 = CARTESIAN_POINT ( 'NONE',  ( 23.06250000122903288, -4.330127018922190985, -2.500000000000001332 ) ) ;
#23659 = CARTESIAN_POINT ( 'NONE',  ( 26.80312500061451431, -4.541064518000417216, -2.621784821875001281 ) ) ;
#23660 = CARTESIAN_POINT ( 'NONE',  ( 26.96249999999999858, -5.773502691896255534, -1.060575238724906372E-15 ) ) ;
#23661 = CARTESIAN_POINT ( 'NONE',  ( 8.484601909799253346E-16, 16.17500000122903003, -25.38119784648299770 ) ) ;
#23662 = CARTESIAN_POINT ( 'NONE',  ( 29.72812500061451502, 4.541064518000418104, 2.621784821874999949 ) ) ;
#23663 = CARTESIAN_POINT ( 'NONE',  ( 11.61562500061451608, 3.027376345333613106, -5.243569643749998122 ) ) ;
#23664 = EDGE_LOOP ( 'NONE', ( #30910, #51367, #27739, #53940 ) ) ;
#23665 = CARTESIAN_POINT ( 'NONE',  ( 25.22812500061451502, 4.541064518000418104, 2.621784821874999949 ) ) ;
#23666 = CARTESIAN_POINT ( 'NONE',  ( 7.565625000614518036, 3.027376345333613106, -5.243569643749998122 ) ) ;
#23667 = CARTESIAN_POINT ( 'NONE',  ( 6.703125000614516438, 4.541064518000418104, -2.621784821874998173 ) ) ;
#23668 = CARTESIAN_POINT ( 'NONE',  ( 16.13437500061451502, 5.824947211148865298E-16, -4.756430356249998326 ) ) ;
#23669 = CARTESIAN_POINT ( 'NONE',  ( 4.640987789384291240, -1.860506746819186041, 4.902426613311977377 ) ) ;
#23670 = CARTESIAN_POINT ( 'NONE',  ( 16.23750000000000071, -2.886751345948125991, -5.000000000000000000 ) ) ;
#23671 = CARTESIAN_POINT ( 'NONE',  ( 15.08437500061451786, -4.541064518000419881, 2.621784821874995952 ) ) ;
#23672 = CARTESIAN_POINT ( 'NONE',  ( 12.45000000122903394, 5.773502691896255534, 3.535250795749688894E-16 ) ) ;
#23673 = CARTESIAN_POINT ( 'NONE',  ( 16.02187500061451786, -6.054752690667223547, -1.112240025338166033E-15 ) ) ;
#23674 = CARTESIAN_POINT ( 'NONE',  ( 18.11250000000000071, 2.886751345948129099, -4.999999999999998224 ) ) ;
#23675 = CARTESIAN_POINT ( 'NONE',  ( 20.25937500061451857, 4.541064518000418104, -2.621784821874998173 ) ) ;
#23676 = CARTESIAN_POINT ( 'NONE',  ( 9.001249775931846008E-16, 14.06562500061451715, -25.09994784771203058 ) ) ;
#23677 = CARTESIAN_POINT ( 'NONE',  ( 45.00000000000000000, 0.000000000000000000, 0.000000000000000000 ) ) ;
#23678 = CARTESIAN_POINT ( 'NONE',  ( 23.10937500061451644, -5.492252693125287522, -1.008910452111647106E-15 ) ) ;
#23679 = CARTESIAN_POINT ( 'NONE',  ( 1.626862140677534470E-15, 13.23124999877096819, 34.00000000000000000 ) ) ;
#23680 = CARTESIAN_POINT ( 'NONE',  ( 25.15312500061451217, 4.541064518000418104, -2.621784821874998173 ) ) ;
#23681 = CARTESIAN_POINT ( 'NONE',  ( 27.45937500061451786, 4.541064518000418104, -2.621784821874998173 ) ) ;
#23682 = CARTESIAN_POINT ( 'NONE',  ( 24.41250000000000142, 2.886751345948129099, -4.999999999999998224 ) ) ;
#23683 = CARTESIAN_POINT ( 'NONE',  ( 7.678125000614516082, 4.541064518000418104, 2.621784821874999949 ) ) ;
#23684 = CARTESIAN_POINT ( 'NONE',  ( 26.07187500061451146, 4.119189519843966529, 2.378215178124999607 ) ) ;
#23685 = CARTESIAN_POINT ( 'NONE',  ( 19.24687500061452283, -3.027376345333610441, -5.243569643749999898 ) ) ;
#23686 = CARTESIAN_POINT ( 'NONE',  ( 10.02187500061451431, -4.119189519843968306, 2.378215178124996054 ) ) ;
#23687 = CARTESIAN_POINT ( 'NONE',  ( 6.328125000614515550, 4.541064518000418104, 2.621784821874999949 ) ) ;
#23688 = CARTESIAN_POINT ( 'NONE',  ( 8.221875000614518925, 3.027376345333611329, 5.243569643749999010 ) ) ;
#23689 = ORIENTED_EDGE ( 'NONE', *, *, #49936, .F. ) ;
#23690 = CARTESIAN_POINT ( 'NONE',  ( 19.84687500061451360, 6.054752690667223547, 3.707466751127219781E-16 ) ) ;
#23691 = CYLINDRICAL_SURFACE ( 'NONE', #4261, 4.999999999999998224 ) ;
#23692 = CARTESIAN_POINT ( 'NONE',  ( 26.09999999999999787, -4.330127018922190985, -2.500000000000001332 ) ) ;
#23693 = CARTESIAN_POINT ( 'NONE',  ( 29.67187500061451644, 3.027376345333613106, -5.243569643749998122 ) ) ;
#23694 = CARTESIAN_POINT ( 'NONE',  ( 34.99999999999999289, 6.363961030679004871, 4.863961030678849440 ) ) ;
#23695 = LINE ( 'NONE', #1918, #55121 ) ;
#23696 = ORIENTED_EDGE ( 'NONE', *, *, #30226, .T. ) ;
#23697 = CARTESIAN_POINT ( 'NONE',  ( 10.42500000000000071, 6.123233995736764310E-16, -4.999999999999998224 ) ) ;
#23698 = CARTESIAN_POINT ( 'NONE',  ( 10.77187500061451608, 4.119189519843966529, 2.378215178124999607 ) ) ;
#23699 = CARTESIAN_POINT ( 'NONE',  ( 25.45312500061451644, -4.541064518000417216, -2.621784821875001281 ) ) ;
#23700 = CARTESIAN_POINT ( 'NONE',  ( 13.35000000000000142, 0.000000000000000000, 4.999999999999998224 ) ) ;
#23701 = CARTESIAN_POINT ( 'NONE',  ( 10.61250000122903536, 4.330127018922192761, -2.499999999999997780 ) ) ;
#23702 = CARTESIAN_POINT ( 'NONE',  ( 9.478125000614515017, 4.541064518000418104, 2.621784821874999949 ) ) ;
#23703 = CARTESIAN_POINT ( 'NONE',  ( 22.31250000000000000, 2.886751345948126879, 4.999999999999999112 ) ) ;
#23704 = CARTESIAN_POINT ( 'NONE',  ( 20.69062500061451715, 6.054752690667223547, 3.707466751127219781E-16 ) ) ;
#23705 = CARTESIAN_POINT ( 'NONE',  ( 26.25000000122903288, -2.886751345948125991, -5.000000000000000000 ) ) ;
#23706 = CARTESIAN_POINT ( 'NONE',  ( -3.756430356250000990, 17.40312499938548285, 32.16877607737301048 ) ) ;
#23707 = CARTESIAN_POINT ( 'NONE',  ( 8.287499999999999645, 5.773502691896255534, 3.535250795749688894E-16 ) ) ;
#23708 = ORIENTED_EDGE ( 'NONE', *, *, #798, .F. ) ;
#23709 = CARTESIAN_POINT ( 'NONE',  ( 23.05312500061451431, 0.000000000000000000, 5.243569643749999010 ) ) ;
#23710 = CARTESIAN_POINT ( 'NONE',  ( 29.69062500061451715, 6.054752690667223547, 3.707466751127219781E-16 ) ) ;
#23711 = CARTESIAN_POINT ( 'NONE',  ( 26.18437500061451573, 4.541064518000418104, 2.621784821874999949 ) ) ;
#23712 = CARTESIAN_POINT ( 'NONE',  ( 18.00937500061451502, 4.541064518000418104, -2.621784821874998173 ) ) ;
#23713 = ADVANCED_FACE ( 'NONE', ( #27812 ), #61412, .F. ) ;
#23714 = CARTESIAN_POINT ( 'NONE',  ( 13.26562500061451644, -6.054752690667223547, -1.112240025338166033E-15 ) ) ;
#23715 = CARTESIAN_POINT ( 'NONE',  ( 12.28125000122903110, 6.123233995736764310E-16, -4.999999999999998224 ) ) ;
#23716 = CARTESIAN_POINT ( 'NONE',  ( 25.61250000122903359, 0.000000000000000000, 4.999999999999998224 ) ) ;
#23717 = CARTESIAN_POINT ( 'NONE',  ( 21.57187500061451502, 2.746126346562645981, -4.756430356249997438 ) ) ;
#23718 = CARTESIAN_POINT ( 'NONE',  ( 15.70312500061451644, 4.541064518000418104, -2.621784821874998173 ) ) ;
#23719 = CARTESIAN_POINT ( 'NONE',  ( 30.00000000000000000, 0.000000000000000000, 0.000000000000000000 ) ) ;
#23720 = CARTESIAN_POINT ( 'NONE',  ( 2.925000001229034918, 2.886751345948129099, -4.999999999999998224 ) ) ;
#23721 = CARTESIAN_POINT ( 'NONE',  ( 11.93437500061451573, -4.541064518000419881, 2.621784821874995952 ) ) ;
#23722 = CARTESIAN_POINT ( 'NONE',  ( 11.55937500061451928, -4.541064518000417216, -2.621784821875001281 ) ) ;
#23723 = CARTESIAN_POINT ( 'NONE',  ( 18.98437500061451644, 4.541064518000418104, 2.621784821874999949 ) ) ;
#23724 = VERTEX_POINT ( 'NONE', #33341 ) ;
#23725 = CARTESIAN_POINT ( 'NONE',  ( 30.00000000000000000, 6.123233995736764310E-16, -4.999999999999998224 ) ) ;
#23726 = CARTESIAN_POINT ( 'NONE',  ( 24.62812500061451715, 6.421520780324663323E-16, -5.243569643749999010 ) ) ;
#23727 = CARTESIAN_POINT ( 'NONE',  ( 19.95937500061451786, 0.000000000000000000, 5.243569643749999010 ) ) ;
#23728 = CARTESIAN_POINT ( 'NONE',  ( 24.81562500061451715, 3.027376345333611329, 5.243569643749999010 ) ) ;
#23729 = CARTESIAN_POINT ( 'NONE',  ( -4.000000000000000888, 17.20624999877096428, 32.30940107675850470 ) ) ;
#23730 = CARTESIAN_POINT ( 'NONE',  ( -3.999999999999997335, 14.63750000000000107, 32.30940107675850470 ) ) ;
#23731 = CARTESIAN_POINT ( 'NONE',  ( 29.76562500061451644, 3.027376345333611329, 5.243569643749999010 ) ) ;
#23732 = CARTESIAN_POINT ( 'NONE',  ( 9.825000001229033941, 2.886751345948126879, 4.999999999999999112 ) ) ;
#23733 = CARTESIAN_POINT ( 'NONE',  ( 4.762500001229033941, 4.330127018922192761, -2.499999999999997780 ) ) ;
#23734 = CARTESIAN_POINT ( 'NONE',  ( 28.46249999999999858, 2.886751345948129099, -4.999999999999997335 ) ) ;
#23735 = CARTESIAN_POINT ( 'NONE',  ( 27.22500000122903430, 2.886751345948129099, -4.999999999999998224 ) ) ;
#23736 = CARTESIAN_POINT ( 'NONE',  ( 2.828200636599751609E-16, 20.65624999877096712, 25.38119784648299415 ) ) ;
#23737 = CARTESIAN_POINT ( 'NONE',  ( 15.76875000122903181, -5.773502691896255534, -1.060575238724906372E-15 ) ) ;
#23738 = CARTESIAN_POINT ( 'NONE',  ( 10.58437500061451964, -4.541064518000419881, 2.621784821874995952 ) ) ;
#23739 = CARTESIAN_POINT ( 'NONE',  ( 24.52499999999999858, 4.330127018922191873, 2.499999999999999556 ) ) ;
#23740 = CARTESIAN_POINT ( 'NONE',  ( 17.76562500061451644, -6.054752690667223547, -1.112240025338166033E-15 ) ) ;
#23741 = CARTESIAN_POINT ( 'NONE',  ( 10.39687500061451786, 6.054752690667223547, 3.707466751127219781E-16 ) ) ;
#23742 = CARTESIAN_POINT ( 'NONE',  ( 28.27500000122903145, 2.886751345948126879, 4.999999999999999112 ) ) ;
#23743 = CARTESIAN_POINT ( 'NONE',  ( 19.35937500061451644, 4.541064518000418104, -2.621784821874998173 ) ) ;
#23744 = CARTESIAN_POINT ( 'NONE',  ( 8.484375000614518214, 6.421520780324663323E-16, -5.243569643749999010 ) ) ;
#23745 = CARTESIAN_POINT ( 'NONE',  ( 14.88750000122903394, -4.330127018922194537, 2.499999999999995559 ) ) ;
#23746 = LINE ( 'NONE', #46294, #28538 ) ;
#23747 = CARTESIAN_POINT ( 'NONE',  ( 8.165625000614516793, 3.027376345333611329, 5.243569643749999010 ) ) ;
#23748 = CARTESIAN_POINT ( 'NONE',  ( 18.44062500061451715, 6.054752690667223547, 3.707466751127219781E-16 ) ) ;
#23749 = ORIENTED_EDGE ( 'NONE', *, *, #54007, .F. ) ;
#23750 = CARTESIAN_POINT ( 'NONE',  ( 5.400000001229032343, -2.886751345948129988, 4.999999999999997335 ) ) ;
#23751 = CARTESIAN_POINT ( 'NONE',  ( 15.14062500061451644, -3.027376345333610441, -5.243569643749999898 ) ) ;
#23752 = CARTESIAN_POINT ( 'NONE',  ( 13.75312500061451715, -4.541064518000417216, -2.621784821875001281 ) ) ;
#23753 = CARTESIAN_POINT ( 'NONE',  ( 24.49687500061451573, -2.746126346562646425, 4.756430356249996549 ) ) ;
#23754 = CARTESIAN_POINT ( 'NONE',  ( 14.47499999999999964, 6.123233995736764310E-16, -4.999999999999998224 ) ) ;
#23755 = CARTESIAN_POINT ( 'NONE',  ( 10.08750000122903323, 6.123233995736764310E-16, -4.999999999999998224 ) ) ;
#23756 = CARTESIAN_POINT ( 'NONE',  ( 5.615625000614517859, -6.054752690667223547, -1.112240025338166033E-15 ) ) ;
#23757 = CARTESIAN_POINT ( 'NONE',  ( 18.00000000122903288, -2.886751345948129988, 4.999999999999997335 ) ) ;
#23758 = CARTESIAN_POINT ( 'NONE',  ( 24.67500000000000071, -4.330127018922194537, 2.499999999999995559 ) ) ;
#23759 = CARTESIAN_POINT ( 'NONE',  ( 2.121784821875001281, 11.00937500061451857, -26.32496088578401938 ) ) ;
#23760 = CARTESIAN_POINT ( 'NONE',  ( 12.50625000122903430, 0.000000000000000000, 4.999999999999998224 ) ) ;
#23761 = FACE_OUTER_BOUND ( 'NONE', #8853, .T. ) ;
#23762 = CARTESIAN_POINT ( 'NONE',  ( 28.38750000122903216, -4.330127018922194537, 2.499999999999995559 ) ) ;
#23763 = CARTESIAN_POINT ( 'NONE',  ( 7.320879633048903241E-15, 17.75000000122903288, 26.00000000000000355 ) ) ;
#23764 = CARTESIAN_POINT ( 'NONE',  ( 18.45937500061451431, 4.541064518000418104, -2.621784821874998173 ) ) ;
#23765 = AXIS2_PLACEMENT_3D ( 'NONE', #23100, #68190, #46012 ) ;
#23766 = CARTESIAN_POINT ( 'NONE',  ( 23.04375000122903216, -2.886751345948153968, -4.999999999999952038 ) ) ;
#23767 = EDGE_CURVE ( 'NONE', #33656, #47420, #18517, .T. ) ;
#23768 = CARTESIAN_POINT ( 'NONE',  ( 14.46562500061451750, 3.027376345333611329, 5.243569643749999010 ) ) ;
#23769 = CARTESIAN_POINT ( 'NONE',  ( 8.456250001229033586, 0.000000000000000000, 4.999999999999998224 ) ) ;
#23770 = CYLINDRICAL_SURFACE ( 'NONE', #62519, 5.999999999999998224 ) ;
#23771 = CARTESIAN_POINT ( 'NONE',  ( 25.80937500061451928, 0.000000000000000000, 5.243569643749999010 ) ) ;
#23772 = CARTESIAN_POINT ( 'NONE',  ( 17.59687500061451360, 0.000000000000000000, 4.756430356249998326 ) ) ;
#23773 = CARTESIAN_POINT ( 'NONE',  ( 13.52812500061451750, 4.541064518000418104, 2.621784821874999949 ) ) ;
#23774 = CARTESIAN_POINT ( 'NONE',  ( 16.69687500061451502, 6.054752690667223547, 3.707466751127219781E-16 ) ) ;
#23775 = VERTEX_POINT ( 'NONE', #44445 ) ;
#23776 = CARTESIAN_POINT ( 'NONE',  ( 26.99062500061451431, 6.054752690667223547, 3.707466751127219781E-16 ) ) ;
#23777 = CARTESIAN_POINT ( 'NONE',  ( 20.69062500061451715, 6.054752690667223547, 3.707466751127219781E-16 ) ) ;
#23778 = CARTESIAN_POINT ( 'NONE',  ( 3.101989702391181769, 3.921444007319114355, -3.480999103934488748 ) ) ;
#23779 = ADVANCED_FACE ( 'NONE', ( #67340 ), #60303, .F. ) ;
#23780 = CARTESIAN_POINT ( 'NONE',  ( 65.00000000000000000, 1.494782592887643924, -8.875000000000003553 ) ) ;
#23781 = CARTESIAN_POINT ( 'NONE',  ( 10.65000000000000036, 0.000000000000000000, 4.999999999999998224 ) ) ;
#23782 = CARTESIAN_POINT ( 'NONE',  ( 18.48750000122903359, -4.330127018922194537, 2.499999999999995559 ) ) ;
#23783 = CARTESIAN_POINT ( 'NONE',  ( 6.937500001229033764, 6.123233995736764310E-16, -4.999999999999998224 ) ) ;
#23784 = CARTESIAN_POINT ( 'NONE',  ( 10.95937500061451431, -5.492252693125287522, -1.008910452111647106E-15 ) ) ;
#23785 = ORIENTED_EDGE ( 'NONE', *, *, #14641, .T. ) ;
#23786 = CARTESIAN_POINT ( 'NONE',  ( 17.25000000000000000, 4.330127018922192761, -2.499999999999997780 ) ) ;
#23787 = ADVANCED_FACE ( 'NONE', ( #16700 ), #39258, .F. ) ;
#23788 = CARTESIAN_POINT ( 'NONE',  ( 20.66250000000000142, -5.773502691896255534, -1.060575238724906372E-15 ) ) ;
#23789 = CARTESIAN_POINT ( 'NONE',  ( 19.58437500061451786, -4.541064518000419881, 2.621784821874995952 ) ) ;
#23790 = CARTESIAN_POINT ( 'NONE',  ( 24.29062500061451502, 6.054752690667223547, 3.707466751127219781E-16 ) ) ;
#23791 = ORIENTED_EDGE ( 'NONE', *, *, #70383, .F. ) ;
#23792 = CARTESIAN_POINT ( 'NONE',  ( 19.87500000000000000, 6.123233995736764310E-16, -4.999999999999998224 ) ) ;
#23793 = CARTESIAN_POINT ( 'NONE',  ( 7.753125000614518036, 0.000000000000000000, 5.243569643749999010 ) ) ;
#23794 = CARTESIAN_POINT ( 'NONE',  ( 3.234375000614516438, 4.541064518000418104, 2.621784821874999949 ) ) ;
#23795 = CARTESIAN_POINT ( 'NONE',  ( 15.56250000000000000, 2.886751345948126879, 4.999999999999999112 ) ) ;
#23796 = CARTESIAN_POINT ( 'NONE',  ( -2.121784821874999949, 16.57812500061451644, 26.32496088578401938 ) ) ;
#23797 = CARTESIAN_POINT ( 'NONE',  ( 28.49062500061451431, -3.027376345333614438, 5.243569643749998122 ) ) ;
#23798 = CARTESIAN_POINT ( 'NONE',  ( 9.562500000000001776, 2.886751345948129099, -4.999999999999998224 ) ) ;
#23799 = CARTESIAN_POINT ( 'NONE',  ( 3.756430356249998770, 16.65312499938548285, 32.16877607737302469 ) ) ;
#23800 = CARTESIAN_POINT ( 'NONE',  ( 25.24687500061451573, 6.054752690667223547, 3.707466751127219781E-16 ) ) ;
#23801 = ORIENTED_EDGE ( 'NONE', *, *, #2612, .F. ) ;
#23802 = CARTESIAN_POINT ( 'NONE',  ( 22.60312500061451857, 0.000000000000000000, 5.243569643749999010 ) ) ;
#23803 = CARTESIAN_POINT ( 'NONE',  ( 23.07187500061451857, 3.027376345333611329, 5.243569643749999010 ) ) ;
#23804 = CARTESIAN_POINT ( 'NONE',  ( 9.001249775931846008E-16, 16.76562500061459460, -25.09994784771203058 ) ) ;
#23805 = CARTESIAN_POINT ( 'NONE',  ( 11.58750000000000036, -2.886751345948129988, 4.999999999999997335 ) ) ;
#23806 = CARTESIAN_POINT ( 'NONE',  ( 5.390625000614518214, 6.054752690667223547, 3.707466751127219781E-16 ) ) ;
#23807 = CARTESIAN_POINT ( 'NONE',  ( 28.73437500061451644, 5.824947211148865298E-16, -4.756430356249998326 ) ) ;
#23808 = CARTESIAN_POINT ( 'NONE',  ( 23.12812500061451360, -4.541064518000419881, 2.621784821874995952 ) ) ;
#23809 = CARTESIAN_POINT ( 'NONE',  ( 27.87187500061451217, 4.119189519843966529, 2.378215178124999607 ) ) ;
#23810 = CARTESIAN_POINT ( 'NONE',  ( 12.83437500061451786, -4.119189519843968306, 2.378215178124996054 ) ) ;
#23811 = CARTESIAN_POINT ( 'NONE',  ( 18.19687500061451502, -3.027376345333614438, 5.243569643749998122 ) ) ;
#23812 = CARTESIAN_POINT ( 'NONE',  ( 4.243569643749999898, 12.88437500061451857, 30.00000000000000000 ) ) ;
#23813 = CARTESIAN_POINT ( 'NONE',  ( 18.49687500061452283, 6.054752690667223547, 3.707466751127219781E-16 ) ) ;
#23814 = CARTESIAN_POINT ( 'NONE',  ( 26.40937500061451715, -4.541064518000417216, -2.621784821875001281 ) ) ;
#23815 = CARTESIAN_POINT ( 'NONE',  ( -4.243569643749999898, 16.67187500061451644, 27.54997392385601529 ) ) ;
#23816 = CARTESIAN_POINT ( 'NONE',  ( 7.040625000614517681, -3.027376345333610441, -5.243569643749999898 ) ) ;
#23817 = CARTESIAN_POINT ( 'NONE',  ( -1.071796769724487453, 18.10759618943233207, -34.00000000000000000 ) ) ;
#23818 = CARTESIAN_POINT ( 'NONE',  ( 4.659375000614518925, 0.000000000000000000, 5.243569643749999010 ) ) ;
#23819 = CARTESIAN_POINT ( 'NONE',  ( 25.83750000122903501, 6.123233995736764310E-16, -4.999999999999998224 ) ) ;
#23820 = CARTESIAN_POINT ( 'NONE',  ( 6.028125000614517504, -4.541064518000419881, 2.621784821874995952 ) ) ;
#23821 = CARTESIAN_POINT ( 'NONE',  ( 10.43437500061451750, 4.541064518000418104, 2.621784821874999949 ) ) ;
#23822 = CARTESIAN_POINT ( 'NONE',  ( 15.52500000122903323, 2.886751345948129099, -4.999999999999998224 ) ) ;
#23823 = CARTESIAN_POINT ( 'NONE',  ( 5.409375000614516260, 4.541064518000418104, -2.621784821874998173 ) ) ;
#23824 = CARTESIAN_POINT ( 'NONE',  ( 7.790625000614518569, -3.027376345333614438, 5.243569643749998122 ) ) ;
#23825 = CARTESIAN_POINT ( 'NONE',  ( 5.053125000614517859, 0.000000000000000000, 5.243569643749999010 ) ) ;
#23826 = CARTESIAN_POINT ( 'NONE',  ( 24.58125000122903003, 4.330127018922191873, 2.499999999999999556 ) ) ;
#23827 = CARTESIAN_POINT ( 'NONE',  ( 17.78437500061451715, -4.541064518000419881, 2.621784821874995952 ) ) ;
#23828 = CARTESIAN_POINT ( 'NONE',  ( -1.071796769724491005, 10.45759618943233527, 26.00000000000000355 ) ) ;
#23829 = ORIENTED_EDGE ( 'NONE', *, *, #55670, .F. ) ;
#23830 = CARTESIAN_POINT ( 'NONE',  ( 24.96562500061451573, -6.054752690667223547, -1.112240025338166033E-15 ) ) ;
#23831 = CARTESIAN_POINT ( 'NONE',  ( 8.915625000614515017, 3.027376345333613106, -5.243569643749998122 ) ) ;
#23832 = EDGE_CURVE ( 'NONE', #39133, #57884, #47571, .T. ) ;
#23833 = CARTESIAN_POINT ( 'NONE',  ( 26.37187500061451573, -6.054752690667223547, -1.112240025338166033E-15 ) ) ;
#23834 = CARTESIAN_POINT ( 'NONE',  ( 9.890625000614516438, 6.054752690667223547, 3.707466751127219781E-16 ) ) ;
#23835 = DIRECTION ( 'NONE',  ( 0.000000000000000000, 1.000000000000000000, -0.000000000000000000 ) ) ;
#23836 = CARTESIAN_POINT ( 'NONE',  ( 9.637500001229033941, 6.123233995736764310E-16, -4.999999999999998224 ) ) ;
#23837 =( BOUNDED_CURVE ( )  B_SPLINE_CURVE ( 2, ( #21600, #11618, #39704, #44154, #66683, #16058, #10527, #12691, #28967 ),
 .UNSPECIFIED., .F., .F. ) 
 B_SPLINE_CURVE_WITH_KNOTS ( ( 3, 2, 2, 2, 3 ),
 ( 0.4673913043478261087, 0.4710144927536231707, 0.4782608695652174058, 0.4855072463768115854, 0.4891304347826087029 ),
 .UNSPECIFIED. ) 
 CURVE ( )  GEOMETRIC_REPRESENTATION_ITEM ( )  RATIONAL_B_SPLINE_CURVE ( ( 0.9330127018922194093, 0.9330127018922198534, 1.000000000000000000, 0.8660254037844387076, 1.000000000000000000, 0.8660254037844387076, 1.000000000000000000, 0.9330127018922194093, 0.9330127018922194093 ) ) 
 REPRESENTATION_ITEM ( '' )  );
#23838 = CARTESIAN_POINT ( 'NONE',  ( 24.40312500061451573, 0.000000000000000000, 5.243569643749999010 ) ) ;
#23839 = AXIS2_PLACEMENT_3D ( 'NONE', #16923, #5497, #11033 ) ;
#23840 = CARTESIAN_POINT ( 'NONE',  ( -4.243569643749997233, 13.99062500061451786, -27.54997392385601174 ) ) ;
#23841 = CARTESIAN_POINT ( 'NONE',  ( 12.90000000122903145, 5.773502691896255534, 3.535250795749688894E-16 ) ) ;
#23842 = CARTESIAN_POINT ( 'NONE',  ( 21.85312500061451502, -4.541064518000417216, -2.621784821875001281 ) ) ;
#23843 = CARTESIAN_POINT ( 'NONE',  ( 11.51250000000000107, 2.886751345948126879, 4.999999999999999112 ) ) ;
#23844 = CARTESIAN_POINT ( 'NONE',  ( 20.91562500061451502, -6.054752690667223547, -1.112240025338166033E-15 ) ) ;
#23845 = CARTESIAN_POINT ( 'NONE',  ( 6.159375000614517148, -4.541064518000417216, -2.621784821875001281 ) ) ;
#23846 = CARTESIAN_POINT ( 'NONE',  ( 19.94999999999999929, 4.330127018922192761, -2.499999999999997780 ) ) ;
#23847 = CARTESIAN_POINT ( 'NONE',  ( 6.750000001229033764, -2.886751345948129988, 4.999999999999997335 ) ) ;
#23848 = CARTESIAN_POINT ( 'NONE',  ( 16.50000000122903288, 5.773502691896255534, 3.535250795749688894E-16 ) ) ;
#23849 = CARTESIAN_POINT ( 'NONE',  ( 12.77812500061451750, -4.541064518000419881, 2.621784821874995952 ) ) ;
#23850 = CARTESIAN_POINT ( 'NONE',  ( 16.64062500061451289, 6.054752690667223547, 3.707466751127219781E-16 ) ) ;
#23851 = CARTESIAN_POINT ( 'NONE',  ( 25.65000000122903145, -2.886751345948129988, 4.999999999999997335 ) ) ;
#23852 = CARTESIAN_POINT ( 'NONE',  ( 20.02500000000000213, 4.330127018922191873, 2.499999999999999556 ) ) ;
#23853 = CARTESIAN_POINT ( 'NONE',  ( 22.88437500061451857, 6.421520780324663323E-16, -5.243569643749999010 ) ) ;
#23854 = CARTESIAN_POINT ( 'NONE',  ( 22.36875000122903145, 2.886751345948098901, 5.000000000000047073 ) ) ;
#23855 = CARTESIAN_POINT ( 'NONE',  ( 11.02500000122903501, 2.886751345948129099, -4.999999999999998224 ) ) ;
#23856 = CARTESIAN_POINT ( 'NONE',  ( 9.046875000614518214, 6.054752690667223547, 3.707466751127219781E-16 ) ) ;
#23857 = CARTESIAN_POINT ( 'NONE',  ( 25.02187500061451431, -6.054752690667223547, -1.112240025338166033E-15 ) ) ;
#23858 = CARTESIAN_POINT ( 'NONE',  ( 3.834375000614519635, -4.541064518000419881, 2.621784821874995952 ) ) ;
#23859 = CARTESIAN_POINT ( 'NONE',  ( 22.11562500061451786, 3.027376345333611329, 5.243569643749999010 ) ) ;
#23860 = CARTESIAN_POINT ( 'NONE',  ( 25.95937500061451431, -4.541064518000417216, -2.621784821875001281 ) ) ;
#23861 = CARTESIAN_POINT ( 'NONE',  ( 2.655984681222220721E-16, 18.26562499938548356, 25.66244784525396483 ) ) ;
#23862 = CARTESIAN_POINT ( 'NONE',  ( 18.00000000000000355, -4.330127018922190985, -2.500000000000001332 ) ) ;
#23863 = CARTESIAN_POINT ( 'NONE',  ( 6.759375000614516793, 4.541064518000418104, -2.621784821874998173 ) ) ;
#23864 = CARTESIAN_POINT ( 'NONE',  ( 18.62812500061451715, -4.541064518000419881, 2.621784821874995952 ) ) ;
#23865 = ORIENTED_EDGE ( 'NONE', *, *, #23767, .T. ) ;
#23866 = CARTESIAN_POINT ( 'NONE',  ( 50.00000000000000000, 8.875000000000000000, -1.494782592887675232 ) ) ;
#23867 = CARTESIAN_POINT ( 'NONE',  ( 28.30312500061451431, 4.541064518000418104, -2.621784821874998173 ) ) ;
#23868 = CARTESIAN_POINT ( 'NONE',  ( 3.384375000614517237, -4.541064518000419881, 2.621784821874995952 ) ) ;
#23869 = CARTESIAN_POINT ( 'NONE',  ( -2.000000000000000000, 14.52500000000000036, 26.53589838486224650 ) ) ;
#23870 = FACE_OUTER_BOUND ( 'NONE', #46060, .T. ) ;
#23871 = CARTESIAN_POINT ( 'NONE',  ( 16.35000000000000142, 4.330127018922192761, -2.499999999999997780 ) ) ;
#23872 = CARTESIAN_POINT ( 'NONE',  ( 21.29062500061451502, -3.027376345333614438, 5.243569643749998122 ) ) ;
#23873 = ORIENTED_EDGE ( 'NONE', *, *, #26612, .T. ) ;
#23874 = CARTESIAN_POINT ( 'NONE',  ( 24.37500000000000000, 6.123233995736764310E-16, -4.999999999999998224 ) ) ;
#23875 = EDGE_CURVE ( 'NONE', #8942, #23775, #63535, .T. ) ;
#23876 = CARTESIAN_POINT ( 'NONE',  ( 26.18437500061451573, 4.541064518000418104, 2.621784821874999949 ) ) ;
#23877 = VERTEX_POINT ( 'NONE', #35149 ) ;
#23878 = CARTESIAN_POINT ( 'NONE',  ( 16.22812500061451857, 4.541064518000418104, 2.621784821874999949 ) ) ;
#23879 = CARTESIAN_POINT ( 'NONE',  ( 6.703125000614516438, 4.541064518000418104, -2.621784821874998173 ) ) ;
#23880 = CARTESIAN_POINT ( 'NONE',  ( 20.10937500061451644, 2.746126346562645981, -4.756430356249997438 ) ) ;
#23881 = CARTESIAN_POINT ( 'NONE',  ( 28.11562500061451431, -6.054752690667223547, -1.112240025338166033E-15 ) ) ;
#23882 = CARTESIAN_POINT ( 'NONE',  ( 14.43750000122903288, -4.330127018922194537, 2.499999999999995559 ) ) ;
#23883 = CARTESIAN_POINT ( 'NONE',  ( 21.78750000000000142, 5.773502691896255534, 3.535250795749688894E-16 ) ) ;
#23884 = CARTESIAN_POINT ( 'NONE',  ( 28.27499999999999858, -4.330127018922194537, 2.499999999999995559 ) ) ;
#23885 = CARTESIAN_POINT ( 'NONE',  ( 5.146875000614517859, -3.027376345333614438, 5.243569643749998122 ) ) ;
#23886 = CARTESIAN_POINT ( 'NONE',  ( 10.35937500061451644, 4.541064518000418104, -2.621784821874998173 ) ) ;
#23887 = CARTESIAN_POINT ( 'NONE',  ( 19.47187500061451360, 3.027376345333611329, 5.243569643749999010 ) ) ;
#23888 = CARTESIAN_POINT ( 'NONE',  ( 10.05000000122903181, -2.886751345948126435, -5.000000000000000000 ) ) ;
#23889 = ORIENTED_EDGE ( 'NONE', *, *, #16221, .F. ) ;
#23890 = CARTESIAN_POINT ( 'NONE',  ( 5.146875000614517859, -3.027376345333614438, 5.243569643749998122 ) ) ;
#23891 = CARTESIAN_POINT ( 'NONE',  ( 3.937500000000000444, -2.886751345948129988, 4.999999999999997335 ) ) ;
#23892 = CARTESIAN_POINT ( 'NONE',  ( 5.184375000614516615, -4.541064518000419881, 2.621784821874995952 ) ) ;
#23893 = CARTESIAN_POINT ( 'NONE',  ( 19.34999999999999787, -4.330127018922190985, -2.500000000000001332 ) ) ;
#23894 = CARTESIAN_POINT ( 'NONE',  ( 16.22812500061451857, 4.541064518000418104, 2.621784821874999949 ) ) ;
#23895 = CARTESIAN_POINT ( 'NONE',  ( -1.999999999999999112, 18.95000000000000284, 26.53589838486224650 ) ) ;
#23896 = CARTESIAN_POINT ( 'NONE',  ( 18.07499999999999929, 6.123233995736764310E-16, -4.999999999999998224 ) ) ;
#23897 = CARTESIAN_POINT ( 'NONE',  ( 19.73437500061451644, 5.824947211148865298E-16, -4.756430356249998326 ) ) ;
#23898 = CARTESIAN_POINT ( 'NONE',  ( 8.990625000614516082, 6.054752690667223547, 3.707466751127219781E-16 ) ) ;
#23899 = CARTESIAN_POINT ( 'NONE',  ( 27.60937500061451644, 0.000000000000000000, 5.243569643749999010 ) ) ;
#23900 = CARTESIAN_POINT ( 'NONE',  ( -2.121784821874996840, 18.58437500061451786, 33.67503911421598417 ) ) ;
#23901 = CARTESIAN_POINT ( 'NONE',  ( 27.15937500061451360, 0.000000000000000000, 5.243569643749999010 ) ) ;
#23902 = CARTESIAN_POINT ( 'NONE',  ( 7.800000000000001599, 4.330127018922192761, -2.499999999999997780 ) ) ;
#23903 = CARTESIAN_POINT ( 'NONE',  ( -3.999999999999999112, 12.01250000122903394, 30.00000000000000000 ) ) ;
#23904 = CARTESIAN_POINT ( 'NONE',  ( 14.72812500061451679, 6.421520780324663323E-16, -5.243569643749999010 ) ) ;
#23905 = CARTESIAN_POINT ( 'NONE',  ( 7.237500001229035362, -4.330127018922194537, 2.499999999999995559 ) ) ;
#23906 = CARTESIAN_POINT ( 'NONE',  ( 18.75937500061451857, -4.541064518000417216, -2.621784821875001281 ) ) ;
#23907 = CARTESIAN_POINT ( 'NONE',  ( 12.42187500061451821, -6.054752690667223547, -1.112240025338166033E-15 ) ) ;
#23908 = CARTESIAN_POINT ( 'NONE',  ( 0.000000000000000000, 10.00000000000000000, 0.000000000000000000 ) ) ;
#23909 = EDGE_LOOP ( 'NONE', ( #42599, #2794, #8934, #12780 ) ) ;
#23910 = CARTESIAN_POINT ( 'NONE',  ( 13.19062500061451537, -3.027376345333614438, 5.243569643749998122 ) ) ;
#23911 = CARTESIAN_POINT ( 'NONE',  ( 25.05000000122903714, 5.773502691896255534, 3.535250795749688894E-16 ) ) ;
#23912 = CARTESIAN_POINT ( 'NONE',  ( 12.00937500061451857, -4.541064518000417216, -2.621784821875001281 ) ) ;
#23913 = CARTESIAN_POINT ( 'NONE',  ( 30.00000000000000000, 0.000000000000000000, 4.999999999999998224 ) ) ;
#23914 = CARTESIAN_POINT ( 'NONE',  ( 15.17812500061451608, 6.421520780324663323E-16, -5.243569643749999010 ) ) ;
#23915 = CARTESIAN_POINT ( 'NONE',  ( 20.94375000122902719, 5.773502691896255534, 3.535250795749688401E-16 ) ) ;
#23916 = CARTESIAN_POINT ( 'NONE',  ( 23.59687500061451715, -3.027376345333614438, 5.243569643749998122 ) ) ;
#23917 = FACE_OUTER_BOUND ( 'NONE', #35256, .T. ) ;
#23918 = CARTESIAN_POINT ( 'NONE',  ( 11.96250000122903501, 4.330127018922192761, -2.499999999999997780 ) ) ;
#23919 = CARTESIAN_POINT ( 'NONE',  ( 20.43750000122903643, 6.123233995736764310E-16, -4.999999999999998224 ) ) ;
#23920 = CARTESIAN_POINT ( 'NONE',  ( -3.000416591977282496E-16, 16.59687500061452070, -34.90005215228797653 ) ) ;
#23921 = CARTESIAN_POINT ( 'NONE',  ( 17.85937500061451999, -4.541064518000417216, -2.621784821875001281 ) ) ;
#23922 = CARTESIAN_POINT ( 'NONE',  ( 18.48750000122903359, -4.330127018922194537, 2.499999999999995559 ) ) ;
#23923 = CARTESIAN_POINT ( 'NONE',  ( 15.19687500061451857, -3.027376345333610441, -5.243569643749999898 ) ) ;
#23924 = CARTESIAN_POINT ( 'NONE',  ( -1.473772837211104525, 9.872922166578584680, 25.95083099200021337 ) ) ;
#23925 = CARTESIAN_POINT ( 'NONE',  ( 20.28750000122903074, -4.330127018922194537, 2.499999999999995559 ) ) ;
#23926 = CARTESIAN_POINT ( 'NONE',  ( 14.12812500061451715, -4.541064518000419881, 2.621784821874995952 ) ) ;
#23927 = ORIENTED_EDGE ( 'NONE', *, *, #18114, .F. ) ;
#23928 = ORIENTED_EDGE ( 'NONE', *, *, #66238, .T. ) ;
#23929 = CARTESIAN_POINT ( 'NONE',  ( 18.00000000000000355, -4.330127018922190985, -2.500000000000001332 ) ) ;
#23930 = CARTESIAN_POINT ( 'NONE',  ( 0.000000000000000000, 10.00000000000000000, 0.000000000000000000 ) ) ;
#23931 = CARTESIAN_POINT ( 'NONE',  ( 4.078125000614517326, 4.541064518000418104, 2.621784821874999949 ) ) ;
#23932 = ADVANCED_FACE ( 'NONE', ( #12615 ), #23691, .F. ) ;
#23933 = CARTESIAN_POINT ( 'NONE',  ( 14.10000000122903252, -2.886751345948125991, -5.000000000000000000 ) ) ;
#23934 = CARTESIAN_POINT ( 'NONE',  ( 27.64687500061452141, -3.027376345333614438, 5.243569643749998122 ) ) ;
#23935 = CARTESIAN_POINT ( 'NONE',  ( 20.12812500061451715, 6.421520780324663323E-16, -5.243569643749999010 ) ) ;
#23936 = CARTESIAN_POINT ( 'NONE',  ( 22.60312500061451857, 0.000000000000000000, 5.243569643749999010 ) ) ;
#23937 = CARTESIAN_POINT ( 'NONE',  ( 2.915625000614516793, -6.054752690667223547, -1.112240025338166033E-15 ) ) ;
#23938 = CARTESIAN_POINT ( 'NONE',  ( 27.97500000000000142, 6.123233995736764310E-16, -4.999999999999998224 ) ) ;
#23939 = CARTESIAN_POINT ( 'NONE',  ( -3.999999999999999112, 10.17500000122903359, -32.30940107675850470 ) ) ;
#23940 = CARTESIAN_POINT ( 'NONE',  ( 10.02187500061451964, 2.746126346562643317, 4.756430356249998326 ) ) ;
#23941 = CARTESIAN_POINT ( 'NONE',  ( 26.90625000122902932, 0.000000000000000000, 4.999999999999998224 ) ) ;
#23942 = DIRECTION ( 'NONE',  ( 0.000000000000000000, 0.000000000000000000, 1.000000000000000000 ) ) ;
#23943 = CARTESIAN_POINT ( 'NONE',  ( 2.121784821874999061, 15.65937500061451892, -33.67503911421598417 ) ) ;
#23944 = CARTESIAN_POINT ( 'NONE',  ( 7.162500001229032520, 0.000000000000000000, 4.999999999999998224 ) ) ;
#23945 = CARTESIAN_POINT ( 'NONE',  ( 5.250000000000000888, 0.000000000000000000, 4.999999999999998224 ) ) ;
#23946 = CARTESIAN_POINT ( 'NONE',  ( 2.887500001229035274, 6.123233995736764310E-16, -4.999999999999998224 ) ) ;
#23947 = CARTESIAN_POINT ( 'NONE',  ( 10.84687500061451892, 6.054752690667223547, 3.707466751127219781E-16 ) ) ;
#23948 = CARTESIAN_POINT ( 'NONE',  ( 29.01562500061451644, -6.054752690667223547, -1.112240025338166033E-15 ) ) ;
#23949 = CYLINDRICAL_SURFACE ( 'NONE', #58620, 4.999999999999998224 ) ;
#23950 = LINE ( 'NONE', #25041, #60954 ) ;
#23951 = CARTESIAN_POINT ( 'NONE',  ( 9.637499999999999289, 5.773502691896255534, 3.535250795749688401E-16 ) ) ;
#23952 = CARTESIAN_POINT ( 'NONE',  ( 8.484375000614518214, 6.421520780324663323E-16, -5.243569643749999010 ) ) ;
#23953 = CARTESIAN_POINT ( 'NONE',  ( 11.44687500061451857, -3.027376345333614438, 5.243569643749998122 ) ) ;
#23954 = CARTESIAN_POINT ( 'NONE',  ( 7.687500000000000000, -2.886751345948125991, -5.000000000000000000 ) ) ;
#23955 = CARTESIAN_POINT ( 'NONE',  ( 9.001249775931846008E-16, 14.96562500061459389, 34.90005215228797653 ) ) ;
#23956 = CARTESIAN_POINT ( 'NONE',  ( 21.98437500061451644, 6.421520780324663323E-16, -5.243569643749999010 ) ) ;
#23957 = EDGE_CURVE ( 'NONE', #50074, #20630, #56947, .T. ) ;
#23958 = CARTESIAN_POINT ( 'NONE',  ( 4.898850051585143718E-16, 25.54316770519903557, 34.00000000000000000 ) ) ;
#23959 = CARTESIAN_POINT ( 'NONE',  ( 6.412500000000001421, 2.886751345948129099, -4.999999999999998224 ) ) ;
#23960 = CARTESIAN_POINT ( 'NONE',  ( 25.91250000122903074, 4.330127018922192761, -2.499999999999997780 ) ) ;
#23961 = CARTESIAN_POINT ( 'NONE',  ( 16.50937500061451502, 2.746126346562645981, -4.756430356249997438 ) ) ;
#23962 = CARTESIAN_POINT ( 'NONE',  ( 21.51562500061451644, 3.027376345333613106, -5.243569643749998122 ) ) ;
#23963 = CARTESIAN_POINT ( 'NONE',  ( 14.16562500061451679, -6.054752690667223547, -1.112240025338166033E-15 ) ) ;
#23964 = CARTESIAN_POINT ( 'NONE',  ( 26.78437500061451715, -2.746126346562642428, -4.756430356249999214 ) ) ;
#23965 = CARTESIAN_POINT ( 'NONE',  ( 9.009375000614518569, 4.541064518000418104, -2.621784821874998173 ) ) ;
#23966 = CARTESIAN_POINT ( 'NONE',  ( 29.32499999999999929, 6.123233995736764310E-16, -4.999999999999998224 ) ) ;
#23967 = CARTESIAN_POINT ( 'NONE',  ( 21.90000000122903145, 5.773502691896255534, 3.535250795749688894E-16 ) ) ;
#23968 = DIRECTION ( 'NONE',  ( 0.000000000000000000, 0.000000000000000000, -1.000000000000000000 ) ) ;
#23969 = CARTESIAN_POINT ( 'NONE',  ( 12.87187500061451750, -6.054752690667223547, -1.112240025338166033E-15 ) ) ;
#23970 = CARTESIAN_POINT ( 'NONE',  ( 28.69687500061451502, -3.027376345333610441, -5.243569643749999898 ) ) ;
#23971 = CARTESIAN_POINT ( 'NONE',  ( 21.80625000122903145, 4.330127018922192761, -2.499999999999997780 ) ) ;
#23972 = CARTESIAN_POINT ( 'NONE',  ( -3.999999999999997335, 14.63750000000000107, 32.30940107675850470 ) ) ;
#23973 = CARTESIAN_POINT ( 'NONE',  ( 21.19687500061451502, 6.054752690667223547, 3.707466751127219781E-16 ) ) ;
#23974 = CARTESIAN_POINT ( 'NONE',  ( 14.74687500061451573, -3.027376345333610441, -5.243569643749999898 ) ) ;
#23975 = CARTESIAN_POINT ( 'NONE',  ( 3.756430356250000102, 19.05312499938548143, 30.00000000000000000 ) ) ;
#23976 = CARTESIAN_POINT ( 'NONE',  ( 26.51249999999999929, -5.773502691896255534, -1.060575238724906372E-15 ) ) ;
#23977 = CARTESIAN_POINT ( 'NONE',  ( 3.756430356250000546, 20.32812499938548356, 27.83122392262697886 ) ) ;
#23978 = CARTESIAN_POINT ( 'NONE',  ( 2.121784821875001281, 14.60937500061451821, -26.32496088578401938 ) ) ;
#23979 = CARTESIAN_POINT ( 'NONE',  ( 27.23437500061451644, -4.119189519843968306, 2.378215178124996054 ) ) ;
#23980 = CARTESIAN_POINT ( 'NONE',  ( 17.50312500061451715, 4.541064518000418104, -2.621784821874998173 ) ) ;
#23981 = CARTESIAN_POINT ( 'NONE',  ( 7.425000000000000711, 4.330127018922191873, 2.499999999999999556 ) ) ;
#23982 =( BOUNDED_CURVE ( )  B_SPLINE_CURVE ( 3, ( #42567, #37019, #59543, #63997 ),
 .UNSPECIFIED., .F., .F. ) 
 B_SPLINE_CURVE_WITH_KNOTS ( ( 4, 4 ),
 ( 3.315795346099966956, 3.411714352141634876 ),
 .UNSPECIFIED. ) 
 CURVE ( )  GEOMETRIC_REPRESENTATION_ITEM ( )  RATIONAL_B_SPLINE_CURVE ( ( 1.000000000000000000, 0.9992334423044004765, 0.9992334423044004765, 1.000000000000000000 ) ) 
 REPRESENTATION_ITEM ( '' )  );
#23983 = CARTESIAN_POINT ( 'NONE',  ( 12.18750000122903465, -4.330127018922194537, 2.499999999999995559 ) ) ;
#23984 = CARTESIAN_POINT ( 'NONE',  ( 14.13750000000000107, 5.773502691896255534, 3.535250795749688894E-16 ) ) ;
#23985 = CARTESIAN_POINT ( 'NONE',  ( -0.7368814052146555049, 9.803648494990884643, 25.82089852767304095 ) ) ;
#23986 = CARTESIAN_POINT ( 'NONE',  ( 14.47500000122903430, -5.773502691896255534, -1.060575238724906372E-15 ) ) ;
#23987 = CARTESIAN_POINT ( 'NONE',  ( 24.68437500061451573, 6.421520780324663323E-16, -5.243569643749999010 ) ) ;
#23988 = VERTEX_POINT ( 'NONE', #62856 ) ;
#23989 = CARTESIAN_POINT ( 'NONE',  ( 19.34062500061451573, 6.054752690667223547, 3.707466751127219781E-16 ) ) ;
#23990 = CARTESIAN_POINT ( 'NONE',  ( 20.37187500061451573, 3.027376345333611329, 5.243569643749999010 ) ) ;
#23991 = CARTESIAN_POINT ( 'NONE',  ( 5.025000000000002132, 6.123233995736764310E-16, -4.999999999999998224 ) ) ;
#23992 = CARTESIAN_POINT ( 'NONE',  ( 8.315625000614515372, -6.054752690667223547, -1.112240025338166033E-15 ) ) ;
#23993 = CARTESIAN_POINT ( 'NONE',  ( 22.86562500061451431, 3.027376345333613106, -5.243569643749998122 ) ) ;
#23994 = CARTESIAN_POINT ( 'NONE',  ( 13.39687500061451608, -3.027376345333610441, -5.243569643749999898 ) ) ;
#23995 = CARTESIAN_POINT ( 'NONE',  ( 17.74687500061451928, -3.027376345333614438, 5.243569643749998122 ) ) ;
#23996 = CARTESIAN_POINT ( 'NONE',  ( -4.243569643749999898, 16.16562500061451857, 27.54997392385601529 ) ) ;
#23997 = CARTESIAN_POINT ( 'NONE',  ( 19.12500000122903288, 2.886751345948129099, -4.999999999999998224 ) ) ;
#23998 = CARTESIAN_POINT ( 'NONE',  ( 14.97187500061451892, 2.746126346562643317, 4.756430356249998326 ) ) ;
#23999 = CARTESIAN_POINT ( 'NONE',  ( 10.49062500061451608, -3.027376345333614438, 5.243569643749998122 ) ) ;
#24000 = CARTESIAN_POINT ( 'NONE',  ( 3.009375000614516793, -4.541064518000417216, -2.621784821875001281 ) ) ;
#24001 = CARTESIAN_POINT ( 'NONE',  ( 29.35312500061451502, 0.000000000000000000, 5.243569643749999010 ) ) ;
#24002 = CARTESIAN_POINT ( 'NONE',  ( 25.65937500061451715, 4.541064518000418104, -2.621784821874998173 ) ) ;
#24003 = CARTESIAN_POINT ( 'NONE',  ( 16.71562500061451573, 3.027376345333611329, 5.243569643749999010 ) ) ;
#24004 = CARTESIAN_POINT ( 'NONE',  ( 27.22500000122903430, 2.886751345948129099, -4.999999999999998224 ) ) ;
#24005 = CARTESIAN_POINT ( 'NONE',  ( 25.56562500061452070, 3.027376345333613106, -5.243569643749998122 ) ) ;
#24006 = CARTESIAN_POINT ( 'NONE',  ( 22.80937500061451573, -4.541064518000417216, -2.621784821875001281 ) ) ;
#24007 = CARTESIAN_POINT ( 'NONE',  ( 16.97812500061451502, 6.421520780324663323E-16, -5.243569643749999010 ) ) ;
#24008 = CARTESIAN_POINT ( 'NONE',  ( -4.243569643749999898, 17.15937500061451715, 30.00000000000000000 ) ) ;
#24009 = CARTESIAN_POINT ( 'NONE',  ( 23.31562500061451715, 3.027376345333613106, -5.243569643749998122 ) ) ;
#24010 = VERTEX_POINT ( 'NONE', #34055 ) ;
#24011 = CARTESIAN_POINT ( 'NONE',  ( 24.78750000000000497, -2.886751345948125991, -5.000000000000000000 ) ) ;
#24012 = CARTESIAN_POINT ( 'NONE',  ( 4.000000000000000000, 12.98749999999999893, -27.69059892324149530 ) ) ;
#24013 = CARTESIAN_POINT ( 'NONE',  ( 1.878215178124997609, 20.32812499938548356, 33.25316411605952993 ) ) ;
#24014 = CARTESIAN_POINT ( 'NONE',  ( 3.009375000614516793, -4.541064518000417216, -2.621784821875001281 ) ) ;
#24015 = CARTESIAN_POINT ( 'NONE',  ( 10.41562500061451679, 3.027376345333611329, 5.243569643749999010 ) ) ;
#24016 = CARTESIAN_POINT ( 'NONE',  ( 22.08750000122903501, -4.330127018922194537, 2.499999999999995559 ) ) ;
#24017 = CARTESIAN_POINT ( 'NONE',  ( 26.99062500061451431, 6.054752690667223547, 3.707466751127219781E-16 ) ) ;
#24018 = CARTESIAN_POINT ( 'NONE',  ( 26.51249999999999929, -5.773502691896255534, -1.060575238724906372E-15 ) ) ;
#24019 = CARTESIAN_POINT ( 'NONE',  ( -3.999999999999997335, 16.55000000122903003, -27.69059892324149175 ) ) ;
#24020 = CARTESIAN_POINT ( 'NONE',  ( 29.69062500061451715, 6.054752690667223547, 3.707466751127219781E-16 ) ) ;
#24021 = CARTESIAN_POINT ( 'NONE',  ( 10.11562500061451608, -6.054752690667223547, -1.112240025338166033E-15 ) ) ;
#24022 = VERTEX_POINT ( 'NONE', #46239 ) ;
#24023 = CARTESIAN_POINT ( 'NONE',  ( 26.42812500061451431, 6.421520780324663323E-16, -5.243569643749999010 ) ) ;
#24024 = CARTESIAN_POINT ( 'NONE',  ( 8.878125000614515372, 6.421520780324663323E-16, -5.243569643749999010 ) ) ;
#24025 = PRODUCT_DEFINITION_CONTEXT ( 'detailed design', #4977, 'design' ) ;
#24026 = CARTESIAN_POINT ( 'NONE',  ( 7.115625000614516082, 3.027376345333613106, -5.243569643749998122 ) ) ;
#24027 = CARTESIAN_POINT ( 'NONE',  ( 15.53437500061451715, -4.119189519843968306, 2.378215178124996054 ) ) ;
#24028 = CARTESIAN_POINT ( 'NONE',  ( 4.652730581016856881, -1.830942677413806896, 4.913544636837456459 ) ) ;
#24029 =( BOUNDED_CURVE ( )  B_SPLINE_CURVE ( 2, ( #51147, #11982, #72592, #57033, #56680, #28975, #34505 ),
 .UNSPECIFIED., .F., .F. ) 
 B_SPLINE_CURVE_WITH_KNOTS ( ( 3, 2, 2, 3 ),
 ( 0.7583333333333333037, 0.7611111111111110716, 0.7638888888888889506, 0.7666666666666668295 ),
 .UNSPECIFIED. ) 
 CURVE ( )  GEOMETRIC_REPRESENTATION_ITEM ( )  RATIONAL_B_SPLINE_CURVE ( ( 1.000000000000000000, 0.8660254037844387076, 1.000000000000000000, 0.8660254037844387076, 1.000000000000000000, 0.8660254037844333785, 1.000000000000005329 ) ) 
 REPRESENTATION_ITEM ( '' )  );
#24030 = CARTESIAN_POINT ( 'NONE',  ( 14.21249999999999858, 2.886751345948126879, 4.999999999999999112 ) ) ;
#24031 =( BOUNDED_SURFACE ( )  B_SPLINE_SURFACE ( 1, 2, ( 
 ( #14991, #48257, #38254, #16444, #27916, #61516, #50450, #55261, #39001, #67447, #4298, #44554, #10914, #67085, #5017, #26823, #55985, #37893, #49357, #33440, #5378, #61159, #21625, #16809, #43450, #72976, #9821, #44183, #22358, #10554, #32353, #20896, #71887, #65972, #44910, #39365, #15352, #61881, #27551, #11287, #33808, #56351, #5741, #28275, #60412, #4657, #72614, #50083, #71521, #54891, #33082, #21260, #55621, #27186, #43813, #66713, #66338, #15716, #60783, #10189, #21996, #49720, #32724, #72248, #16087, #38635, #56699, #46351, #209, #17173, #11647, #45634, #45267, #51168, #572, #23442, #68885, #52252, #63687, #39733, #51892, #62250, #35255, #69251, #57055, #68167, #6099, #18613, #35616, #22714, #58136, #28630, #34162, #67800, #23077, #13077, #17530, #18242, #24164, #934, #6462, #1290, #45988, #1655, #40815, #34892, #40092, #62606, #12002, #34525, #28997, #51534, #68525, #17886, #40446, #57776, #62962, #12358, #57421, #63331, #7186, #6825, #29359, #23800, #12719, #29714, #46716, #41178, #7542, #50807, #52975, #69965, #24889, #18971, #31542, #13811, #59967, #30076, #64050, #19336, #14906, #9010, #53338, #70331, #37074, #24531, #59230, #36351, #54082, #47434, #31167, #2020, #69610, #47075, #2736, #52614, #30805, #58865, #41891, #19707, #64418, #8275, #2371, #41531, #71064, #25631, #13430, #20068, #53709, #35980, #7908, #3479, #64783, #8638, #37447, #25998, #30446, #58499, #25253, #47802, #14174, #48537, #42260, #3102, #36708, #48168, #70693, #20439, #42988, #42624, #65148, #14538, #65520, #59598, #4933, #44828, #67363, #55538, #22276, #15269, #27837, #43727, #16726, #72162, #66999, #50369, #10828, #44096, #38549, #10469, #61072, #16000, #5291, #48903, #31907, #32999, #65888, #26738, #10107, #27103, #43365, #60327, #37807, #27468, #66250, #21541, #49635, #55177, #16361, #15628, #61435, #72894, #39281, #49999, #66623, #32271, #32637, #38915, #33363, #9737, #55900, #54804, #4573, #72524, #3843, #9375, #54444, #4210, #49272, #21913, #26364, #44469, #71805, #21174, #71434, #38170, #60694, #20810, #45550, #11563, #34079, #28549, #56619, #50725, #63242, #68079, #19529, #61793, #22633, #51083, #47619, #40726, #11917, #28906, #68802, #56270, #17798, #17448, #12636, #6014, #62877, #33725, #28196, #5660, #34442, #11198, #62520, #40005, #480, #51444, #22989, #56970, #6374, #128, #29629, #57336, #45183, #51804, #12273, #67715, #39648, #35171, #23355, #40358, #70151, #57695, #62167, #17087, #846, #45904, #68435, #7100, #34804, #6740, #29274, #1207, #23712, #52166, #1569, #46262, #18158, #25076, #32462, #30994, #37629, #4402, #26931, #15093, #54996, #47996, #60518, #3298, #49456, #31731, #26557, #9923, #43551, #3663, #71249, #43187, #20628, #48726, #37996, #8459, #64609, #65707, #25452, #59420, #42813, #59790, #2922, #19899, #70524, #60152, #25825, #54269, #9196, #14726, #49097, #48362, #20999, #71990, #42087, #9562, #26186, #64974, #65336, #71626, #31364, #13995, #66073, #37268, #32095, #15451, #36534, #54626, #70888, #59054, #8828, #4032, #53527, #42452, #14365, #36900, #53905, #20261, #27653, #61262, #61618, #10656, #5119, #44289, #15820, #62350, #16908, #38364, #11386, #22459, #27290, #72348, #45367, #56092, #73078, #6202, #306, #21729, #60890, #66818, #51270, #5483, #67903, #50192, #67545, #67188, #33186, #43918, #11746, #34263, #16191, #11020, #4757, #56796, #10295, #39463, #28729, #21364, #61985, #66444, #49824, #39836, #55725, #32826, #33541, #5839, #55364, #22816, #28022, #50550, #45009, #33905, #56449, #17274, #38742, #72717, #28371, #22100, #44658, #16549, #39101, #50908, #51636, #57158, #52356, #57530, #12824, #40925, #46455, #58243, #35000, #52716, #64154, #13541, #1759, #63438, #23544, #23907, #30186, #24634, #1037, #68993, #18352, #68269, #7647, #45734, #6570, #46094, #63792, #2123, #29821, #68630, #17992, #24273, #40551, #6930, #35358, #29461, #63068, #12471, #51997, #1398, #62712, #47180, #57882, #30552, #673, #34629, #29101, #7292, #69712, #46822, #69359, #18717, #41281, #13182, #19080, #35721, #41635, #36089, #58609, #8016, #23180, #17631, #40191, #12106, #59707, #58971, #37549, #19443, #8378, #71168, #65624, #42733, #3212, #71544, #24998, #54547, #64524, #25741, #48643, #65252, #13918, #2474, #53449, #47541, #15012, #20540, #70070, #9483, #9114, #3949, #60071, #43097, #32012, #20917, #42004, #36818, #54185, #31652, #26104, #36456, #14642, #15374, #37182, #8744, #26473, #48278, #49011, #2839, #42369, #43469, #3582, #59333, #25368, #65993, #30908, #37916, #47912, #60434, #70441, #19817, #64891, #14281, #31276, #53819, #70802, #20178, #9844, #53078, #45287, #71908, #33460, #43835, #16830, #50828, #38657, #49742, #60804, #229, #17193, #54912, #39754, #10211, #21281, #49378, #4320, #67821, #32745, #50469, #5762, #55642, #61181, #56006, #5037, #56371, #22379, #16463, #55283, #26845, #66362, #4677, #27207, #38276, #10576, #72270, #22019, #44930, #15737, #62272, #10936, #33103, #16106, #32373, #21647, #44204, #66735, #27573, #50105, #72635, #44574, #67106, #67467, #39022, #61536, #5399, #27936, #72997, #39383, #61902, #11307, #33828, #28294, #22736, #40111, #12735, #68186, #51553, #29731, #41194, #1671, #63703, #68544, #52269, #7558, #17550, #57793, #24180, #7202, #18260, #62626, #69267, #51188, #12021, #46733, #18630, #1309, #34912, #30093, #56717, #13094, #23096, #57440, #35632, #23818, #45654, #34182, #34545, #6119, #58153, #52630, #28649, #2035, #40833, #24546, #47091, #69624, #18986, #41548, #591, #17904, #35272, #63350, #11666, #57074, #46369, #6482, #68903, #40466, #29016, #6843, #954, #23462, #46008, #62981, #12377, #29378, #51911, #43006, #30461, #65535, #69981, #59613, #13446, #52990, #24905, #58879, #58513, #64433, #13825, #36723, #9027, #14921 ),
 ( #42639, #36366, #25269, #8653, #47816, #8289, #30820, #53352, #2750, #2387, #37463, #70346, #19723, #42274, #47449, #59982, #64797, #20826, #64065, #19351, #14188, #48921, #9393, #59245, #31183, #71079, #7924, #20083, #53725, #31923, #3117, #65163, #35995, #41908, #25647, #48184, #70708, #14555, #37089, #31558, #54098, #3495, #26014, #48552, #20453, #54459, #3858, #26380, #71452, #44485, #49287, #21192, #67379, #4950, #21929, #28211, #22291, #43743, #60343, #15646, #143, #27484, #16741, #72180, #16378, #16017, #32654, #65904, #11214, #56286, #66268, #10488, #26755, #33740, #32286, #38933, #5675, #50740, #61451, #43380, #71820, #61811, #4589, #15284, #33015, #27853, #37824, #44843, #50017, #72541, #67017, #10845, #33379, #39296, #9752, #54820, #55915, #38186, #60711, #44113, #61089, #4228, #10123, #55195, #5310, #27118, #55554, #50384, #38565, #72909, #49652, #21559, #66640, #35545, #1222, #12287, #45566, #45919, #52182, #46641, #497, #17813, #68451, #17103, #29644, #67729, #28565, #68098, #12650, #1584, #51819, #17463, #23007, #23728, #40022, #56986, #40374, #6392, #62536, #28924, #40742, #18543, #51101, #68817, #63258, #18173, #29289, #11933, #7115, #62182, #34458, #35185, #57711, #34822, #62893, #41107, #39663, #24093, #34095, #57350, #69182, #6756, #56635, #45198, #51461, #11579, #63617, #13007, #6031, #58065, #46278, #7474, #30000, #52543, #22649, #864, #23371, #58794, #3028, #8568, #48100, #69540, #64714, #37375, #14098, #30733, #54012, #25180, #70623, #2303, #64347, #3408, #25559, #8204, #24818, #25928, #41461, #48468, #7839, #19998, #24457, #63980, #35903, #69896, #18899, #47365, #19262, #47723, #42551, #70992, #14834, #13362, #65078, #58428, #59525, #20368, #53265, #41816, #30376, #42919, #59899, #47005, #9304, #52905, #13738, #36280, #2663, #31838, #70262, #14469, #65442, #19633, #42190, #37003, #36638, #1950, #8938, #59160, #31096, #53635, #31469, #26669, #49202, #60255, #10034, #71736, #44026, #44401, #3769, #11125, #32932, #55107, #38102, #61724, #48831, #16654, #37735, #66548, #50302, #9669, #55470, #32202, #21106, #72453, #10762, #66927, #33295, #4862, #27036, #5220, #16296, #38477, #54736, #26294, #71361, #43659, #66181, #4138, #32569, #15559, #15927, #38850, #20736, #54374, #27398, #4507, #60624, #43294, #65815, #39212, #49567, #61001, #72824, #72089, #49928, #21473, #10400, #21837, #55833, #61365, #27762, #22207, #44761, #67296, #15197, #6674, #51737, #29202, #40290, #39572, #18091, #59, #62096, #1137, #46192, #23284, #56901, #52097, #5590, #35101, #45113, #6306, #23647, #45833, #67648, #56197, #34012, #28127, #68733, #40652, #50655, #63172, #62812, #57626, #12567, #7030, #29560, #1502, #22565, #17380, #34732, #12204, #24007, #17014, #68370, #69096, #17731, #62451, #46555, #28834, #18458, #56549, #22918, #41022, #57261, #39938, #5943, #63538, #11490, #33652, #28476, #51013, #409, #45475, #68008, #11849, #34368, #51373, #776, #58709, #31013, #14385, #25845, #52459, #14016, #24372, #70543, #31384, #19179, #30288, #41379, #53924, #70909, #35458, #20281, #63890, #1866, #29919, #57981, #48382, #13280, #53546, #59441, #36191, #41732, #36555, #8120, #36920, #2942, #70173, #35819, #7391, #46920, #58341, #7751, #18816, #64260, #52820, #2577, #25471, #69458, #42835, #64630, #13647, #69813, #12924, #2222, #24735, #47279, #25096, #8848, #30648, #59075, #53180, #47640, #48017, #42472, #19918, #64995, #19550, #3319, #42107, #8479, #38385, #10312, #60908, #72007, #71271, #49842, #31754, #20649, #32844, #4775, #55015, #15471, #11683, #37289, #67836, #3684, #38015, #55381, #4420, #26208, #14747, #65726, #59812, #27309, #72367, #9217, #21747, #21382, #17209, #45302, #39771, #62287, #34198, #54291, #49117, #66462, #43938, #56732, #48747, #26949, #28665, #49475, #21018, #6135, #60537, #51204, #15112, #54647, #606, #15839, #71645, #37649, #23112, #43206, #65357, #60172, #9581, #32113, #4051, #26577, #43571, #66092, #9944, #32482, #18275, #63717, #47107, #58529, #12036, #46749, #57089, #30109, #64080, #51927, #62998, #968, #13462, #30477, #68204, #53006, #23478, #34561, #62641, #17565, #7939, #46024, #13109, #19001, #68918, #1324, #12392, #69283, #40127, #6497, #29033, #40849, #2401, #46384, #23834, #34928, #12752, #57455, #29393, #68561, #51568, #36011, #41209, #17919, #35647, #18645, #40482, #6860, #69639, #7218, #24195, #45669, #24561, #63367, #35287, #57809, #29747, #52285, #41562, #1686, #58169, #7574, #52643, #2050, #65920, #37839, #47834, #65180, #8306, #15300, #13841, #20468, #60359, #9768, #71094, #32302, #30836, #43397, #59261, #54837, #14571, #9408, #24922, #26396, #59630, #54112, #26029, #3510, #31573, #20843, #64450, #47464, #48568, #53369, #42291, #25665, #42656, #58896, #2766, #25288, #43022, #8670, #37104, #9043, #70724, #31938, #31201, #3873, #69997, #19366, #65550, #14939, #70364, #48202, #54475, #48938, #19742, #20099, #37478, #41924, #71467, #36380, #64815, #14205, #59998, #36741, #53743, #3136, #55212, #55932, #49670, #38582, #21946, #61107, #27136, #72197, #44130, #21576, #66285, #5691, #10504, #34113, #4244, #38202, #66657, #62200, #56301, #27499, #44502, #11233, #71837, #33396, #33032, #28226, #15663, #61828, #22665, #55571, #16034, #32671, #45215, #11596, #26771, #49303, #4605, #60728, #21208, #43760, #39680, #4966, #22308, #50756, #50033, #72558, #5328, #67035, #159, #67396, #61468, #16395, #10139, #38950, #10863, #27869, #50401, #72926, #44860, #16758, #39316, #33756, #67749, #17121, #40391, #23388, #58081, #51118, #13023, #68114, #6774, #18558, #40040, #68834, #17480, #28942, #63275, #52198, #12667, #1599, #45937, #35204, #41123, #62554, #40760, #57726, #18190, #1240, #11950, #7131, #515, #34475, #29661, #24110, #29306, #62910 ) ),
 .UNSPECIFIED., .F., .F., .F. ) 
 B_SPLINE_SURFACE_WITH_KNOTS ( ( 2, 2 ),
 ( 3, 2, 2, 2, 2, 2, 2, 2, 2, 2, 2, 2, 2, 2, 2, 2, 2, 2, 2, 2, 2, 2, 2, 2, 2, 2, 2, 2, 2, 2, 2, 2, 2, 2, 2, 2, 2, 2, 2, 2, 2, 2, 2, 2, 2, 2, 2, 2, 2, 2, 2, 2, 2, 2, 2, 2, 2, 2, 2, 2, 2, 2, 2, 2, 2, 2, 2, 2, 2, 2, 2, 2, 2, 2, 2, 2, 2, 2, 2, 2, 2, 2, 2, 2, 2, 2, 2, 2, 2, 2, 2, 2, 2, 2, 2, 2, 2, 2, 2, 2, 2, 2, 2, 2, 2, 2, 2, 2, 2, 2, 2, 2, 2, 2, 2, 2, 2, 2, 2, 2, 2, 2, 2, 2, 2, 2, 2, 2, 2, 2, 2, 2, 2, 2, 2, 2, 2, 2, 2, 2, 2, 2, 2, 2, 2, 2, 2, 2, 2, 2, 2, 2, 2, 2, 2, 2, 2, 2, 2, 2, 2, 2, 2, 2, 2, 2, 2, 2, 2, 2, 2, 2, 2, 2, 2, 2, 2, 2, 2, 2, 2, 2, 2, 2, 2, 2, 2, 2, 2, 2, 2, 2, 2, 2, 2, 2, 2, 2, 2, 2, 2, 2, 2, 2, 2, 2, 2, 2, 2, 2, 2, 2, 2, 2, 2, 2, 2, 2, 2, 2, 2, 2, 2, 2, 2, 2, 2, 2, 2, 2, 2, 2, 2, 2, 2, 2, 2, 2, 2, 2, 2, 2, 2, 2, 2, 2, 2, 2, 2, 2, 2, 2, 2, 2, 2, 2, 2, 2, 2, 2, 2, 2, 2, 2, 2, 2, 2, 2, 2, 2, 2, 2, 2, 2, 2, 2, 2, 2, 2, 2, 2, 2, 2, 2, 2, 2, 2, 2, 2, 2, 2, 2, 2, 2, 2, 2, 2, 2, 2, 2, 2, 2, 2, 2, 2, 2, 2, 2, 2, 2, 2, 2, 2, 2, 2, 2, 2, 2, 2, 2, 2, 2, 2, 2, 2, 2, 2, 2, 2, 2, 2, 2, 2, 2, 2, 2, 2, 2, 2, 2, 2, 2, 2, 2, 2, 2, 2, 2, 2, 2, 2, 2, 2, 2, 2, 2, 2, 2, 2, 2, 3 ),
 ( 0.000000000000000000, 1.000000000000000000 ),
 ( 0.000000000000000000, 0.002777777777777777884, 0.005555555555555555768, 0.008333333333333333218, 0.01111111111111111154, 0.01388888888888888812, 0.01666666666666666644, 0.01944444444444444475, 0.02222222222222222307, 0.02500000000000000139, 0.02777777777777777624, 0.03055555555555555455, 0.03333333333333333287, 0.03611111111111110772, 0.03888888888888888951, 0.04166666666666666435, 0.04444444444444444614, 0.04722222222222222099, 0.05000000000000000278, 0.05277777777777777762, 0.05555555555555555247, 0.05833333333333333426, 0.06111111111111110911, 0.06388888888888888395, 0.06666666666666666574, 0.06944444444444444753, 0.07222222222222221544, 0.07499999999999999722, 0.07777777777777777901, 0.08055555555555556080, 0.08333333333333332871, 0.08611111111111111049, 0.08888888888888889228, 0.09166666666666666019, 0.09444444444444444198, 0.09722222222222222376, 0.1000000000000000056, 0.1027777777777777735, 0.1055555555555555552, 0.1083333333333333370, 0.1111111111111111049, 0.1138888888888888867, 0.1166666666666666685, 0.1194444444444444503, 0.1222222222222222182, 0.1250000000000000000, 0.1277777777777777679, 0.1305555555555555636, 0.1333333333333333315, 0.1361111111111110994, 0.1388888888888888951, 0.1416666666666666630, 0.1444444444444444309, 0.1472222222222222265, 0.1499999999999999944, 0.1527777777777777901, 0.1555555555555555580, 0.1583333333333333259, 0.1611111111111111216, 0.1638888888888888895, 0.1666666666666666574, 0.1694444444444444531, 0.1722222222222222210, 0.1749999999999999889, 0.1777777777777777846, 0.1805555555555555525, 0.1833333333333333204, 0.1861111111111111160, 0.1888888888888888840, 0.1916666666666666796, 0.1944444444444444475, 0.1972222222222222154, 0.2000000000000000111, 0.2027777777777777790, 0.2055555555555555469, 0.2083333333333333426, 0.2111111111111111105, 0.2138888888888888784, 0.2166666666666666741, 0.2194444444444444420, 0.2222222222222222099, 0.2250000000000000056, 0.2277777777777777735, 0.2305555555555555691, 0.2333333333333333370, 0.2361111111111111049, 0.2388888888888889006, 0.2416666666666666685, 0.2444444444444444364, 0.2472222222222222321, 0.2500000000000000000, 0.2527777777777777679, 0.2555555555555555358, 0.2583333333333333592, 0.2611111111111111271, 0.2638888888888888951, 0.2666666666666666630, 0.2694444444444444309, 0.2722222222222221988, 0.2750000000000000222, 0.2777777777777777901, 0.2805555555555555580, 0.2833333333333333259, 0.2861111111111110938, 0.2888888888888888618, 0.2916666666666666852, 0.2944444444444444531, 0.2972222222222222210, 0.2999999999999999889, 0.3027777777777777568, 0.3055555555555555802, 0.3083333333333333481, 0.3111111111111111160, 0.3138888888888888840, 0.3166666666666666519, 0.3194444444444444198, 0.3222222222222222432, 0.3250000000000000111, 0.3277777777777777790, 0.3305555555555555469, 0.3333333333333333148, 0.3361111111111111382, 0.3388888888888889062, 0.3416666666666666741, 0.3444444444444444420, 0.3472222222222222099, 0.3499999999999999778, 0.3527777777777778012, 0.3555555555555555691, 0.3583333333333333370, 0.3611111111111111049, 0.3638888888888888729, 0.3666666666666666408, 0.3694444444444444642, 0.3722222222222222321, 0.3750000000000000000, 0.3777777777777777679, 0.3805555555555555358, 0.3833333333333333592, 0.3861111111111111271, 0.3888888888888888951, 0.3916666666666666630, 0.3944444444444444309, 0.3972222222222221988, 0.4000000000000000222, 0.4027777777777777901, 0.4055555555555555580, 0.4083333333333333259, 0.4111111111111110938, 0.4138888888888888618, 0.4166666666666666852, 0.4194444444444444531, 0.4222222222222222210, 0.4249999999999999889, 0.4277777777777777568, 0.4305555555555555802, 0.4333333333333333481, 0.4361111111111111160, 0.4388888888888888840, 0.4416666666666666519, 0.4444444444444444198, 0.4472222222222222432, 0.4500000000000000111, 0.4527777777777777790, 0.4555555555555555469, 0.4583333333333333148, 0.4611111111111111382, 0.4638888888888889062, 0.4666666666666666741, 0.4694444444444444420, 0.4722222222222222099, 0.4749999999999999778, 0.4777777777777778012, 0.4805555555555555691, 0.4833333333333333370, 0.4861111111111111049, 0.4888888888888888729, 0.4916666666666666408, 0.4944444444444444642, 0.4972222222222222321, 0.5000000000000000000, 0.5027777777777777679, 0.5055555555555555358, 0.5083333333333333037, 0.5111111111111110716, 0.5138888888888888395, 0.5166666666666667185, 0.5194444444444444864, 0.5222222222222222543, 0.5250000000000000222, 0.5277777777777777901, 0.5305555555555555580, 0.5333333333333333259, 0.5361111111111110938, 0.5388888888888888618, 0.5416666666666666297, 0.5444444444444443976, 0.5472222222222222765, 0.5500000000000000444, 0.5527777777777778123, 0.5555555555555555802, 0.5583333333333333481, 0.5611111111111111160, 0.5638888888888888840, 0.5666666666666666519, 0.5694444444444444198, 0.5722222222222221877, 0.5749999999999999556, 0.5777777777777777235, 0.5805555555555556024, 0.5833333333333333703, 0.5861111111111111382, 0.5888888888888889062, 0.5916666666666666741, 0.5944444444444444420, 0.5972222222222222099, 0.5999999999999999778, 0.6027777777777777457, 0.6055555555555555136, 0.6083333333333332815, 0.6111111111111111605, 0.6138888888888889284, 0.6166666666666666963, 0.6194444444444444642, 0.6222222222222222321, 0.6250000000000000000, 0.6277777777777777679, 0.6305555555555555358, 0.6333333333333333037, 0.6361111111111110716, 0.6388888888888888395, 0.6416666666666667185, 0.6444444444444444864, 0.6472222222222222543, 0.6500000000000000222, 0.6527777777777777901, 0.6555555555555555580, 0.6583333333333333259, 0.6611111111111110938, 0.6638888888888888618, 0.6666666666666666297, 0.6694444444444443976, 0.6722222222222222765, 0.6750000000000000444, 0.6777777777777778123, 0.6805555555555555802, 0.6833333333333333481, 0.6861111111111111160, 0.6888888888888888840, 0.6916666666666666519, 0.6944444444444444198, 0.6972222222222221877, 0.6999999999999999556, 0.7027777777777777235, 0.7055555555555556024, 0.7083333333333333703, 0.7111111111111111382, 0.7138888888888889062, 0.7166666666666666741, 0.7194444444444444420, 0.7222222222222222099, 0.7249999999999999778, 0.7277777777777777457, 0.7305555555555555136, 0.7333333333333332815, 0.7361111111111111605, 0.7388888888888889284, 0.7416666666666666963, 0.7444444444444444642, 0.7472222222222222321, 0.7500000000000000000, 0.7527777777777777679, 0.7555555555555555358, 0.7583333333333333037, 0.7611111111111110716, 0.7638888888888888395, 0.7666666666666667185, 0.7694444444444444864, 0.7722222222222222543, 0.7750000000000000222, 0.7777777777777777901, 0.7805555555555555580, 0.7833333333333333259, 0.7861111111111110938, 0.7888888888888888618, 0.7916666666666666297, 0.7944444444444443976, 0.7972222222222222765, 0.8000000000000000444, 0.8027777777777778123, 0.8055555555555555802, 0.8083333333333333481, 0.8111111111111111160, 0.8138888888888888840, 0.8166666666666666519, 0.8194444444444444198, 0.8222222222222221877, 0.8249999999999999556, 0.8277777777777777235, 0.8305555555555556024, 0.8333333333333333703, 0.8361111111111111382, 0.8388888888888889062, 0.8416666666666666741, 0.8444444444444444420, 0.8472222222222222099, 0.8499999999999999778, 0.8527777777777777457, 0.8555555555555555136, 0.8583333333333332815, 0.8611111111111111605, 0.8638888888888889284, 0.8666666666666666963, 0.8694444444444444642, 0.8722222222222222321, 0.8750000000000000000, 0.8777777777777777679, 0.8805555555555555358, 0.8833333333333333037, 0.8861111111111110716, 0.8888888888888888395, 0.8916666666666667185, 0.8944444444444444864, 0.8972222222222222543, 0.9000000000000000222, 0.9027777777777777901, 0.9055555555555555580, 0.9083333333333333259, 0.9111111111111110938, 0.9138888888888888618, 0.9166666666666666297, 0.9194444444444443976, 0.9222222222222222765, 0.9250000000000000444, 0.9277777777777778123, 0.9305555555555555802, 0.9333333333333333481, 0.9361111111111111160, 0.9388888888888888840, 0.9416666666666666519, 0.9444444444444444198, 0.9472222222222221877, 0.9499999999999999556, 0.9527777777777777235, 0.9555555555555556024, 0.9583333333333333703, 0.9611111111111111382, 0.9638888888888889062, 0.9666666666666666741, 0.9694444444444444420, 0.9722222222222222099, 0.9749999999999999778, 0.9777777777777777457, 0.9805555555555555136, 0.9833333333333332815, 0.9861111111111111605, 0.9888888888888889284, 0.9916666666666666963, 0.9944444444444444642, 0.9972222222222222321, 1.000000000000000000 ),
 .UNSPECIFIED. ) 
 GEOMETRIC_REPRESENTATION_ITEM ( )  RATIONAL_B_SPLINE_SURFACE ( (
 ( 1.000000000000000000, 0.8660254037844387076, 1.000000000000000000, 0.8660254037844387076, 1.000000000000000000, 0.8660254037844387076, 1.000000000000000000, 0.8660254037844387076, 1.000000000000000000, 0.8660254037844387076, 1.000000000000000000, 0.8660254037844387076, 1.000000000000000000, 0.8660254037844387076, 1.000000000000000000, 0.8660254037844387076, 1.000000000000000000, 0.8660254037844387076, 1.000000000000000000, 0.8660254037844387076, 1.000000000000000000, 0.8660254037844387076, 1.000000000000000000, 0.8660254037844387076, 1.000000000000000000, 0.8660254037844387076, 1.000000000000000000, 0.8660254037844387076, 1.000000000000000000, 0.8660254037844387076, 1.000000000000000000, 0.8660254037844387076, 1.000000000000000000, 0.8660254037844387076, 1.000000000000000000, 0.8660254037844387076, 1.000000000000000000, 0.8660254037844387076, 1.000000000000000000, 0.8660254037844387076, 1.000000000000000000, 0.8660254037844387076, 1.000000000000000000, 0.8660254037844387076, 1.000000000000000000, 0.8660254037844387076, 1.000000000000000000, 0.8660254037844387076, 1.000000000000000000, 0.8660254037844387076, 1.000000000000000000, 0.8660254037844387076, 1.000000000000000000, 0.8660254037844387076, 1.000000000000000000, 0.8660254037844387076, 1.000000000000000000, 0.8660254037844387076, 1.000000000000000000, 0.8660254037844387076, 1.000000000000000000, 0.8660254037844387076, 1.000000000000000000, 0.8660254037844387076, 1.000000000000000000, 0.8660254037844387076, 1.000000000000000000, 0.8660254037844387076, 1.000000000000000000, 0.8660254037844387076, 1.000000000000000000, 0.8660254037844387076, 1.000000000000000000, 0.8660254037844387076, 1.000000000000000000, 0.8660254037844387076, 1.000000000000000000, 0.8660254037844387076, 1.000000000000000000, 0.8660254037844387076, 1.000000000000000000, 0.8660254037844387076, 1.000000000000000000, 0.8660254037844387076, 1.000000000000000000, 0.8660254037844387076, 1.000000000000000000, 0.8660254037844387076, 1.000000000000000000, 0.8660254037844387076, 1.000000000000000000, 0.8660254037844387076, 1.000000000000000000, 0.8660254037844387076, 1.000000000000000000, 0.8660254037844387076, 1.000000000000000000, 0.8660254037844387076, 1.000000000000000000, 0.8660254037844387076, 1.000000000000000000, 0.8660254037844387076, 1.000000000000000000, 0.8660254037844387076, 1.000000000000000000, 0.8660254037844387076, 1.000000000000000000, 0.8660254037844387076, 1.000000000000000000, 0.8660254037844387076, 1.000000000000000000, 0.8660254037844387076, 1.000000000000000000, 0.8660254037844387076, 1.000000000000000000, 0.8660254037844387076, 1.000000000000000000, 0.8660254037844387076, 1.000000000000000000, 0.8660254037844387076, 1.000000000000000000, 0.8660254037844387076, 1.000000000000000000, 0.8660254037844387076, 1.000000000000000000, 0.8660254037844387076, 1.000000000000000000, 0.8660254037844387076, 1.000000000000000000, 0.8660254037844387076, 1.000000000000000000, 0.8660254037844387076, 1.000000000000000000, 0.8660254037844387076, 1.000000000000000000, 0.8660254037844387076, 1.000000000000000000, 0.8660254037844387076, 1.000000000000000000, 0.8660254037844387076, 1.000000000000000000, 0.8660254037844387076, 1.000000000000000000, 0.8660254037844387076, 1.000000000000000000, 0.8660254037844387076, 1.000000000000000000, 0.8660254037844387076, 1.000000000000000000, 0.8660254037844387076, 1.000000000000000000, 0.8660254037844387076, 1.000000000000000000, 0.8660254037844387076, 1.000000000000000000, 0.8660254037844387076, 1.000000000000000000, 0.8660254037844387076, 1.000000000000000000, 0.8660254037844387076, 1.000000000000000000, 0.8660254037844387076, 1.000000000000000000, 0.8660254037844387076, 1.000000000000000000, 0.8660254037844387076, 1.000000000000000000, 0.8660254037844387076, 1.000000000000000000, 0.8660254037844387076, 1.000000000000000000, 0.8660254037844387076, 1.000000000000000000, 0.8660254037844387076, 1.000000000000000000, 0.8660254037844387076, 1.000000000000000000, 0.8660254037844387076, 1.000000000000000000, 0.8660254037844387076, 1.000000000000000000, 0.8660254037844387076, 1.000000000000000000, 0.8660254037844387076, 1.000000000000000000, 0.8660254037844387076, 1.000000000000000000, 0.8660254037844387076, 1.000000000000000000, 0.8660254037844387076, 1.000000000000000000, 0.8660254037844387076, 1.000000000000000000, 0.8660254037844387076, 1.000000000000000000, 0.8660254037844387076, 1.000000000000000000, 0.8660254037844387076, 1.000000000000000000, 0.8660254037844387076, 1.000000000000000000, 0.8660254037844387076, 1.000000000000000000, 0.8660254037844387076, 1.000000000000000000, 0.8660254037844387076, 1.000000000000000000, 0.8660254037844387076, 1.000000000000000000, 0.8660254037844387076, 1.000000000000000000, 0.8660254037844387076, 1.000000000000000000, 0.8660254037844387076, 1.000000000000000000, 0.8660254037844387076, 1.000000000000000000, 0.8660254037844387076, 1.000000000000000000, 0.8660254037844387076, 1.000000000000000000, 0.8660254037844387076, 1.000000000000000000, 0.8660254037844387076, 1.000000000000000000, 0.8660254037844387076, 1.000000000000000000, 0.8660254037844387076, 1.000000000000000000, 0.8660254037844387076, 1.000000000000000000, 0.8660254037844387076, 1.000000000000000000, 0.8660254037844387076, 1.000000000000000000, 0.8660254037844387076, 1.000000000000000000, 0.8660254037844387076, 1.000000000000000000, 0.8660254037844387076, 1.000000000000000000, 0.8660254037844387076, 1.000000000000000000, 0.8660254037844387076, 1.000000000000000000, 0.8660254037844387076, 1.000000000000000000, 0.8660254037844387076, 1.000000000000000000, 0.8660254037844387076, 1.000000000000000000, 0.8660254037844387076, 1.000000000000000000, 0.8660254037844387076, 1.000000000000000000, 0.8660254037844387076, 1.000000000000000000, 0.8660254037844387076, 1.000000000000000000, 0.8660254037844387076, 1.000000000000000000, 0.8660254037844387076, 1.000000000000000000, 0.8660254037844387076, 1.000000000000000000, 0.8660254037844387076, 1.000000000000000000, 0.8660254037844387076, 1.000000000000000000, 0.8660254037844387076, 1.000000000000000000, 0.8660254037844387076, 1.000000000000000000, 0.8660254037844387076, 1.000000000000000000, 0.8660254037844387076, 1.000000000000000000, 0.8660254037844387076, 1.000000000000000000, 0.8660254037844387076, 1.000000000000000000, 0.8660254037844387076, 1.000000000000000000, 0.8660254037844387076, 1.000000000000000000, 0.8660254037844387076, 1.000000000000000000, 0.8660254037844387076, 1.000000000000000000, 0.8660254037844387076, 1.000000000000000000, 0.8660254037844387076, 1.000000000000000000, 0.8660254037844387076, 1.000000000000000000, 0.8660254037844387076, 1.000000000000000000, 0.8660254037844387076, 1.000000000000000000, 0.8660254037844387076, 1.000000000000000000, 0.8660254037844387076, 1.000000000000000000, 0.8660254037844387076, 1.000000000000000000, 0.8660254037844387076, 1.000000000000000000, 0.8660254037844387076, 1.000000000000000000, 0.8660254037844387076, 1.000000000000000000, 0.8660254037844387076, 1.000000000000000000, 0.8660254037844387076, 1.000000000000000000, 0.8660254037844387076, 1.000000000000000000, 0.8660254037844387076, 1.000000000000000000, 0.8660254037844387076, 1.000000000000000000, 0.8660254037844387076, 1.000000000000000000, 0.8660254037844387076, 1.000000000000000000, 0.8660254037844387076, 1.000000000000000000, 0.8660254037844387076, 1.000000000000000000, 0.8660254037844387076, 1.000000000000000000, 0.8660254037844387076, 1.000000000000000000, 0.8660254037844387076, 1.000000000000000000, 0.8660254037844387076, 1.000000000000000000, 0.8660254037844387076, 1.000000000000000000, 0.8660254037844387076, 1.000000000000000000, 0.8660254037844387076, 1.000000000000000000, 0.8660254037844387076, 1.000000000000000000, 0.8660254037844387076, 1.000000000000000000, 0.8660254037844387076, 1.000000000000000000, 0.8660254037844387076, 1.000000000000000000, 0.8660254037844387076, 1.000000000000000000, 0.8660254037844387076, 1.000000000000000000, 0.8660254037844387076, 1.000000000000000000, 0.8660254037844387076, 1.000000000000000000, 0.8660254037844387076, 1.000000000000000000, 0.8660254037844387076, 1.000000000000000000, 0.8660254037844387076, 1.000000000000000000, 0.8660254037844387076, 1.000000000000000000, 0.8660254037844387076, 1.000000000000000000, 0.8660254037844387076, 1.000000000000000000, 0.8660254037844387076, 1.000000000000000000, 0.8660254037844387076, 1.000000000000000000, 0.8660254037844387076, 1.000000000000000000, 0.8660254037844387076, 1.000000000000000000, 0.8660254037844387076, 1.000000000000000000, 0.8660254037844387076, 1.000000000000000000, 0.8660254037844387076, 1.000000000000000000, 0.8660254037844387076, 1.000000000000000000, 0.8660254037844387076, 1.000000000000000000, 0.8660254037844387076, 1.000000000000000000, 0.8660254037844387076, 1.000000000000000000, 0.8660254037844387076, 1.000000000000000000, 0.8660254037844387076, 1.000000000000000000, 0.8660254037844387076, 1.000000000000000000, 0.8660254037844387076, 1.000000000000000000, 0.8660254037844387076, 1.000000000000000000, 0.8660254037844387076, 1.000000000000000000, 0.8660254037844387076, 1.000000000000000000, 0.8660254037844387076, 1.000000000000000000, 0.8660254037844387076, 1.000000000000000000, 0.8660254037844387076, 1.000000000000000000, 0.8660254037844387076, 1.000000000000000000, 0.8660254037844387076, 1.000000000000000000, 0.8660254037844387076, 1.000000000000000000, 0.8660254037844387076, 1.000000000000000000, 0.8660254037844387076, 1.000000000000000000, 0.8660254037844387076, 1.000000000000000000, 0.8660254037844387076, 1.000000000000000000, 0.8660254037844387076, 1.000000000000000000, 0.8660254037844387076, 1.000000000000000000, 0.8660254037844387076, 1.000000000000000000, 0.8660254037844387076, 1.000000000000000000, 0.8660254037844387076, 1.000000000000000000, 0.8660254037844387076, 1.000000000000000000, 0.8660254037844387076, 1.000000000000000000, 0.8660254037844387076, 1.000000000000000000, 0.8660254037844387076, 1.000000000000000000, 0.8660254037844387076, 1.000000000000000000, 0.8660254037844387076, 1.000000000000000000, 0.8660254037844387076, 1.000000000000000000, 0.8660254037844387076, 1.000000000000000000, 0.8660254037844387076, 1.000000000000000000, 0.8660254037844387076, 1.000000000000000000, 0.8660254037844387076, 1.000000000000000000, 0.8660254037844387076, 1.000000000000000000, 0.8660254037844387076, 1.000000000000000000, 0.8660254037844387076, 1.000000000000000000, 0.8660254037844387076, 1.000000000000000000, 0.8660254037844387076, 1.000000000000000000, 0.8660254037844387076, 1.000000000000000000, 0.8660254037844387076, 1.000000000000000000, 0.8660254037844387076, 1.000000000000000000, 0.8660254037844387076, 1.000000000000000000, 0.8660254037844387076, 1.000000000000000000, 0.8660254037844387076, 1.000000000000000000, 0.8660254037844387076, 1.000000000000000000, 0.8660254037844387076, 1.000000000000000000, 0.8660254037844387076, 1.000000000000000000, 0.8660254037844387076, 1.000000000000000000, 0.8660254037844387076, 1.000000000000000000, 0.8660254037844387076, 1.000000000000000000, 0.8660254037844387076, 1.000000000000000000, 0.8660254037844387076, 1.000000000000000000, 0.8660254037844387076, 1.000000000000000000, 0.8660254037844387076, 1.000000000000000000, 0.8660254037844387076, 1.000000000000000000, 0.8660254037844387076, 1.000000000000000000, 0.8660254037844387076, 1.000000000000000000, 0.8660254037844387076, 1.000000000000000000, 0.8660254037844387076, 1.000000000000000000, 0.8660254037844387076, 1.000000000000000000, 0.8660254037844387076, 1.000000000000000000, 0.8660254037844387076, 1.000000000000000000, 0.8660254037844387076, 1.000000000000000000, 0.8660254037844387076, 1.000000000000000000, 0.8660254037844387076, 1.000000000000000000, 0.8660254037844387076, 1.000000000000000000, 0.8660254037844387076, 1.000000000000000000, 0.8660254037844387076, 1.000000000000000000, 0.8660254037844387076, 1.000000000000000000, 0.8660254037844387076, 1.000000000000000000, 0.8660254037844387076, 1.000000000000000000, 0.8660254037844387076, 1.000000000000000000, 0.8660254037844387076, 1.000000000000000000, 0.8660254037844387076, 1.000000000000000000, 0.8660254037844387076, 1.000000000000000000, 0.8660254037844387076, 1.000000000000000000, 0.8660254037844387076, 1.000000000000000000, 0.8660254037844387076, 1.000000000000000000, 0.8660254037844387076, 1.000000000000000000, 0.8660254037844387076, 1.000000000000000000, 0.8660254037844387076, 1.000000000000000000, 0.8660254037844387076, 1.000000000000000000, 0.8660254037844387076, 1.000000000000000000, 0.8660254037844387076, 1.000000000000000000, 0.8660254037844387076, 1.000000000000000000, 0.8660254037844387076, 1.000000000000000000, 0.8660254037844387076, 1.000000000000000000, 0.8660254037844387076, 1.000000000000000000, 0.8660254037844387076, 1.000000000000000000, 0.8660254037844387076, 1.000000000000000000, 0.8660254037844387076, 1.000000000000000000, 0.8660254037844387076, 1.000000000000000000, 0.8660254037844387076, 1.000000000000000000, 0.8660254037844387076, 1.000000000000000000, 0.8660254037844387076, 1.000000000000000000, 0.8660254037844387076, 1.000000000000000000, 0.8660254037844387076, 1.000000000000000000, 0.8660254037844387076, 1.000000000000000000, 0.8660254037844387076, 1.000000000000000000, 0.8660254037844387076, 1.000000000000000000, 0.8660254037844387076, 1.000000000000000000, 0.8660254037844387076, 1.000000000000000000, 0.8660254037844387076, 1.000000000000000000, 0.8660254037844387076, 1.000000000000000000, 0.8660254037844387076, 1.000000000000000000, 0.8660254037844387076, 1.000000000000000000, 0.8660254037844387076, 1.000000000000000000, 0.8660254037844387076, 1.000000000000000000, 0.8660254037844387076, 1.000000000000000000, 0.8660254037844387076, 1.000000000000000000, 0.8660254037844387076, 1.000000000000000000, 0.8660254037844387076, 1.000000000000000000, 0.8660254037844387076, 1.000000000000000000, 0.8660254037844387076, 1.000000000000000000, 0.8660254037844387076, 1.000000000000000000, 0.8660254037844387076, 1.000000000000000000, 0.8660254037844387076, 1.000000000000000000, 0.8660254037844387076, 1.000000000000000000, 0.8660254037844387076, 1.000000000000000000, 0.8660254037844387076, 1.000000000000000000, 0.8660254037844387076, 1.000000000000000000, 0.8660254037844387076, 1.000000000000000000, 0.8660254037844387076, 1.000000000000000000, 0.8660254037844387076, 1.000000000000000000, 0.8660254037844387076, 1.000000000000000000, 0.8660254037844387076, 1.000000000000000000, 0.8660254037844387076, 1.000000000000000000, 0.8660254037844387076, 1.000000000000000000, 0.8660254037844387076, 1.000000000000000000, 0.8660254037844387076, 1.000000000000000000, 0.8660254037844387076, 1.000000000000000000, 0.8660254037844387076, 1.000000000000000000, 0.8660254037844387076, 1.000000000000000000, 0.8660254037844387076, 1.000000000000000000, 0.8660254037844387076, 1.000000000000000000, 0.8660254037844387076, 1.000000000000000000, 0.8660254037844387076, 1.000000000000000000, 0.8660254037844387076, 1.000000000000000000, 0.8660254037844387076, 1.000000000000000000, 0.8660254037844387076, 1.000000000000000000, 0.8660254037844387076, 1.000000000000000000, 0.8660254037844387076, 1.000000000000000000, 0.8660254037844387076, 1.000000000000000000, 0.8660254037844387076, 1.000000000000000000, 0.8660254037844387076, 1.000000000000000000, 0.8660254037844387076, 1.000000000000000000, 0.8660254037844387076, 1.000000000000000000, 0.8660254037844387076, 1.000000000000000000, 0.8660254037844387076, 1.000000000000000000, 0.8660254037844387076, 1.000000000000000000, 0.8660254037844387076, 1.000000000000000000, 0.8660254037844387076, 1.000000000000000000, 0.8660254037844387076, 1.000000000000000000, 0.8660254037844387076, 1.000000000000000000, 0.8660254037844387076, 1.000000000000000000, 0.8660254037844387076, 1.000000000000000000, 0.8660254037844387076, 1.000000000000000000, 0.8660254037844387076, 1.000000000000000000, 0.8660254037844387076, 1.000000000000000000, 0.8660254037844387076, 1.000000000000000000, 0.8660254037844387076, 1.000000000000000000, 0.8660254037844387076, 1.000000000000000000, 0.8660254037844387076, 1.000000000000000000, 0.8660254037844387076, 1.000000000000000000),
 ( 1.000000000000000000, 0.8660254037844387076, 1.000000000000000000, 0.8660254037844387076, 1.000000000000000000, 0.8660254037844387076, 1.000000000000000000, 0.8660254037844387076, 1.000000000000000000, 0.8660254037844387076, 1.000000000000000000, 0.8660254037844387076, 1.000000000000000000, 0.8660254037844387076, 1.000000000000000000, 0.8660254037844387076, 1.000000000000000000, 0.8660254037844387076, 1.000000000000000000, 0.8660254037844387076, 1.000000000000000000, 0.8660254037844387076, 1.000000000000000000, 0.8660254037844387076, 1.000000000000000000, 0.8660254037844387076, 1.000000000000000000, 0.8660254037844387076, 1.000000000000000000, 0.8660254037844387076, 1.000000000000000000, 0.8660254037844387076, 1.000000000000000000, 0.8660254037844387076, 1.000000000000000000, 0.8660254037844387076, 1.000000000000000000, 0.8660254037844387076, 1.000000000000000000, 0.8660254037844387076, 1.000000000000000000, 0.8660254037844387076, 1.000000000000000000, 0.8660254037844387076, 1.000000000000000000, 0.8660254037844387076, 1.000000000000000000, 0.8660254037844387076, 1.000000000000000000, 0.8660254037844387076, 1.000000000000000000, 0.8660254037844387076, 1.000000000000000000, 0.8660254037844387076, 1.000000000000000000, 0.8660254037844387076, 1.000000000000000000, 0.8660254037844387076, 1.000000000000000000, 0.8660254037844387076, 1.000000000000000000, 0.8660254037844387076, 1.000000000000000000, 0.8660254037844387076, 1.000000000000000000, 0.8660254037844387076, 1.000000000000000000, 0.8660254037844387076, 1.000000000000000000, 0.8660254037844387076, 1.000000000000000000, 0.8660254037844387076, 1.000000000000000000, 0.8660254037844387076, 1.000000000000000000, 0.8660254037844387076, 1.000000000000000000, 0.8660254037844387076, 1.000000000000000000, 0.8660254037844387076, 1.000000000000000000, 0.8660254037844387076, 1.000000000000000000, 0.8660254037844387076, 1.000000000000000000, 0.8660254037844387076, 1.000000000000000000, 0.8660254037844387076, 1.000000000000000000, 0.8660254037844387076, 1.000000000000000000, 0.8660254037844387076, 1.000000000000000000, 0.8660254037844387076, 1.000000000000000000, 0.8660254037844387076, 1.000000000000000000, 0.8660254037844387076, 1.000000000000000000, 0.8660254037844387076, 1.000000000000000000, 0.8660254037844387076, 1.000000000000000000, 0.8660254037844387076, 1.000000000000000000, 0.8660254037844387076, 1.000000000000000000, 0.8660254037844387076, 1.000000000000000000, 0.8660254037844387076, 1.000000000000000000, 0.8660254037844387076, 1.000000000000000000, 0.8660254037844387076, 1.000000000000000000, 0.8660254037844387076, 1.000000000000000000, 0.8660254037844387076, 1.000000000000000000, 0.8660254037844387076, 1.000000000000000000, 0.8660254037844387076, 1.000000000000000000, 0.8660254037844387076, 1.000000000000000000, 0.8660254037844387076, 1.000000000000000000, 0.8660254037844387076, 1.000000000000000000, 0.8660254037844387076, 1.000000000000000000, 0.8660254037844387076, 1.000000000000000000, 0.8660254037844387076, 1.000000000000000000, 0.8660254037844387076, 1.000000000000000000, 0.8660254037844387076, 1.000000000000000000, 0.8660254037844387076, 1.000000000000000000, 0.8660254037844387076, 1.000000000000000000, 0.8660254037844387076, 1.000000000000000000, 0.8660254037844387076, 1.000000000000000000, 0.8660254037844387076, 1.000000000000000000, 0.8660254037844387076, 1.000000000000000000, 0.8660254037844387076, 1.000000000000000000, 0.8660254037844387076, 1.000000000000000000, 0.8660254037844387076, 1.000000000000000000, 0.8660254037844387076, 1.000000000000000000, 0.8660254037844387076, 1.000000000000000000, 0.8660254037844387076, 1.000000000000000000, 0.8660254037844387076, 1.000000000000000000, 0.8660254037844387076, 1.000000000000000000, 0.8660254037844387076, 1.000000000000000000, 0.8660254037844387076, 1.000000000000000000, 0.8660254037844387076, 1.000000000000000000, 0.8660254037844387076, 1.000000000000000000, 0.8660254037844387076, 1.000000000000000000, 0.8660254037844387076, 1.000000000000000000, 0.8660254037844387076, 1.000000000000000000, 0.8660254037844387076, 1.000000000000000000, 0.8660254037844387076, 1.000000000000000000, 0.8660254037844387076, 1.000000000000000000, 0.8660254037844387076, 1.000000000000000000, 0.8660254037844387076, 1.000000000000000000, 0.8660254037844387076, 1.000000000000000000, 0.8660254037844387076, 1.000000000000000000, 0.8660254037844387076, 1.000000000000000000, 0.8660254037844387076, 1.000000000000000000, 0.8660254037844387076, 1.000000000000000000, 0.8660254037844387076, 1.000000000000000000, 0.8660254037844387076, 1.000000000000000000, 0.8660254037844387076, 1.000000000000000000, 0.8660254037844387076, 1.000000000000000000, 0.8660254037844387076, 1.000000000000000000, 0.8660254037844387076, 1.000000000000000000, 0.8660254037844387076, 1.000000000000000000, 0.8660254037844387076, 1.000000000000000000, 0.8660254037844387076, 1.000000000000000000, 0.8660254037844387076, 1.000000000000000000, 0.8660254037844387076, 1.000000000000000000, 0.8660254037844387076, 1.000000000000000000, 0.8660254037844387076, 1.000000000000000000, 0.8660254037844387076, 1.000000000000000000, 0.8660254037844387076, 1.000000000000000000, 0.8660254037844387076, 1.000000000000000000, 0.8660254037844387076, 1.000000000000000000, 0.8660254037844387076, 1.000000000000000000, 0.8660254037844387076, 1.000000000000000000, 0.8660254037844387076, 1.000000000000000000, 0.8660254037844387076, 1.000000000000000000, 0.8660254037844387076, 1.000000000000000000, 0.8660254037844387076, 1.000000000000000000, 0.8660254037844387076, 1.000000000000000000, 0.8660254037844387076, 1.000000000000000000, 0.8660254037844387076, 1.000000000000000000, 0.8660254037844387076, 1.000000000000000000, 0.8660254037844387076, 1.000000000000000000, 0.8660254037844387076, 1.000000000000000000, 0.8660254037844387076, 1.000000000000000000, 0.8660254037844387076, 1.000000000000000000, 0.8660254037844387076, 1.000000000000000000, 0.8660254037844387076, 1.000000000000000000, 0.8660254037844387076, 1.000000000000000000, 0.8660254037844387076, 1.000000000000000000, 0.8660254037844387076, 1.000000000000000000, 0.8660254037844387076, 1.000000000000000000, 0.8660254037844387076, 1.000000000000000000, 0.8660254037844387076, 1.000000000000000000, 0.8660254037844387076, 1.000000000000000000, 0.8660254037844387076, 1.000000000000000000, 0.8660254037844387076, 1.000000000000000000, 0.8660254037844387076, 1.000000000000000000, 0.8660254037844387076, 1.000000000000000000, 0.8660254037844387076, 1.000000000000000000, 0.8660254037844387076, 1.000000000000000000, 0.8660254037844387076, 1.000000000000000000, 0.8660254037844387076, 1.000000000000000000, 0.8660254037844387076, 1.000000000000000000, 0.8660254037844387076, 1.000000000000000000, 0.8660254037844387076, 1.000000000000000000, 0.8660254037844387076, 1.000000000000000000, 0.8660254037844387076, 1.000000000000000000, 0.8660254037844387076, 1.000000000000000000, 0.8660254037844387076, 1.000000000000000000, 0.8660254037844387076, 1.000000000000000000, 0.8660254037844387076, 1.000000000000000000, 0.8660254037844387076, 1.000000000000000000, 0.8660254037844387076, 1.000000000000000000, 0.8660254037844387076, 1.000000000000000000, 0.8660254037844387076, 1.000000000000000000, 0.8660254037844387076, 1.000000000000000000, 0.8660254037844387076, 1.000000000000000000, 0.8660254037844387076, 1.000000000000000000, 0.8660254037844387076, 1.000000000000000000, 0.8660254037844387076, 1.000000000000000000, 0.8660254037844387076, 1.000000000000000000, 0.8660254037844387076, 1.000000000000000000, 0.8660254037844387076, 1.000000000000000000, 0.8660254037844387076, 1.000000000000000000, 0.8660254037844387076, 1.000000000000000000, 0.8660254037844387076, 1.000000000000000000, 0.8660254037844387076, 1.000000000000000000, 0.8660254037844387076, 1.000000000000000000, 0.8660254037844387076, 1.000000000000000000, 0.8660254037844387076, 1.000000000000000000, 0.8660254037844387076, 1.000000000000000000, 0.8660254037844387076, 1.000000000000000000, 0.8660254037844387076, 1.000000000000000000, 0.8660254037844387076, 1.000000000000000000, 0.8660254037844387076, 1.000000000000000000, 0.8660254037844387076, 1.000000000000000000, 0.8660254037844387076, 1.000000000000000000, 0.8660254037844387076, 1.000000000000000000, 0.8660254037844387076, 1.000000000000000000, 0.8660254037844387076, 1.000000000000000000, 0.8660254037844387076, 1.000000000000000000, 0.8660254037844387076, 1.000000000000000000, 0.8660254037844387076, 1.000000000000000000, 0.8660254037844387076, 1.000000000000000000, 0.8660254037844387076, 1.000000000000000000, 0.8660254037844387076, 1.000000000000000000, 0.8660254037844387076, 1.000000000000000000, 0.8660254037844387076, 1.000000000000000000, 0.8660254037844387076, 1.000000000000000000, 0.8660254037844387076, 1.000000000000000000, 0.8660254037844387076, 1.000000000000000000, 0.8660254037844387076, 1.000000000000000000, 0.8660254037844387076, 1.000000000000000000, 0.8660254037844387076, 1.000000000000000000, 0.8660254037844387076, 1.000000000000000000, 0.8660254037844387076, 1.000000000000000000, 0.8660254037844387076, 1.000000000000000000, 0.8660254037844387076, 1.000000000000000000, 0.8660254037844387076, 1.000000000000000000, 0.8660254037844387076, 1.000000000000000000, 0.8660254037844387076, 1.000000000000000000, 0.8660254037844387076, 1.000000000000000000, 0.8660254037844387076, 1.000000000000000000, 0.8660254037844387076, 1.000000000000000000, 0.8660254037844387076, 1.000000000000000000, 0.8660254037844387076, 1.000000000000000000, 0.8660254037844387076, 1.000000000000000000, 0.8660254037844387076, 1.000000000000000000, 0.8660254037844387076, 1.000000000000000000, 0.8660254037844387076, 1.000000000000000000, 0.8660254037844387076, 1.000000000000000000, 0.8660254037844387076, 1.000000000000000000, 0.8660254037844387076, 1.000000000000000000, 0.8660254037844387076, 1.000000000000000000, 0.8660254037844387076, 1.000000000000000000, 0.8660254037844387076, 1.000000000000000000, 0.8660254037844387076, 1.000000000000000000, 0.8660254037844387076, 1.000000000000000000, 0.8660254037844387076, 1.000000000000000000, 0.8660254037844387076, 1.000000000000000000, 0.8660254037844387076, 1.000000000000000000, 0.8660254037844387076, 1.000000000000000000, 0.8660254037844387076, 1.000000000000000000, 0.8660254037844387076, 1.000000000000000000, 0.8660254037844387076, 1.000000000000000000, 0.8660254037844387076, 1.000000000000000000, 0.8660254037844387076, 1.000000000000000000, 0.8660254037844387076, 1.000000000000000000, 0.8660254037844387076, 1.000000000000000000, 0.8660254037844387076, 1.000000000000000000, 0.8660254037844387076, 1.000000000000000000, 0.8660254037844387076, 1.000000000000000000, 0.8660254037844387076, 1.000000000000000000, 0.8660254037844387076, 1.000000000000000000, 0.8660254037844387076, 1.000000000000000000, 0.8660254037844387076, 1.000000000000000000, 0.8660254037844387076, 1.000000000000000000, 0.8660254037844387076, 1.000000000000000000, 0.8660254037844387076, 1.000000000000000000, 0.8660254037844387076, 1.000000000000000000, 0.8660254037844387076, 1.000000000000000000, 0.8660254037844387076, 1.000000000000000000, 0.8660254037844387076, 1.000000000000000000, 0.8660254037844387076, 1.000000000000000000, 0.8660254037844387076, 1.000000000000000000, 0.8660254037844387076, 1.000000000000000000, 0.8660254037844387076, 1.000000000000000000, 0.8660254037844387076, 1.000000000000000000, 0.8660254037844387076, 1.000000000000000000, 0.8660254037844387076, 1.000000000000000000, 0.8660254037844387076, 1.000000000000000000, 0.8660254037844387076, 1.000000000000000000, 0.8660254037844387076, 1.000000000000000000, 0.8660254037844387076, 1.000000000000000000, 0.8660254037844387076, 1.000000000000000000, 0.8660254037844387076, 1.000000000000000000, 0.8660254037844387076, 1.000000000000000000, 0.8660254037844387076, 1.000000000000000000, 0.8660254037844387076, 1.000000000000000000, 0.8660254037844387076, 1.000000000000000000, 0.8660254037844387076, 1.000000000000000000, 0.8660254037844387076, 1.000000000000000000, 0.8660254037844387076, 1.000000000000000000, 0.8660254037844387076, 1.000000000000000000, 0.8660254037844387076, 1.000000000000000000, 0.8660254037844387076, 1.000000000000000000, 0.8660254037844387076, 1.000000000000000000, 0.8660254037844387076, 1.000000000000000000, 0.8660254037844387076, 1.000000000000000000, 0.8660254037844387076, 1.000000000000000000, 0.8660254037844387076, 1.000000000000000000, 0.8660254037844387076, 1.000000000000000000, 0.8660254037844387076, 1.000000000000000000, 0.8660254037844387076, 1.000000000000000000, 0.8660254037844387076, 1.000000000000000000, 0.8660254037844387076, 1.000000000000000000, 0.8660254037844387076, 1.000000000000000000, 0.8660254037844387076, 1.000000000000000000, 0.8660254037844387076, 1.000000000000000000, 0.8660254037844387076, 1.000000000000000000, 0.8660254037844387076, 1.000000000000000000, 0.8660254037844387076, 1.000000000000000000, 0.8660254037844387076, 1.000000000000000000, 0.8660254037844387076, 1.000000000000000000, 0.8660254037844387076, 1.000000000000000000, 0.8660254037844387076, 1.000000000000000000, 0.8660254037844387076, 1.000000000000000000, 0.8660254037844387076, 1.000000000000000000, 0.8660254037844387076, 1.000000000000000000, 0.8660254037844387076, 1.000000000000000000, 0.8660254037844387076, 1.000000000000000000, 0.8660254037844387076, 1.000000000000000000, 0.8660254037844387076, 1.000000000000000000, 0.8660254037844387076, 1.000000000000000000, 0.8660254037844387076, 1.000000000000000000, 0.8660254037844387076, 1.000000000000000000, 0.8660254037844387076, 1.000000000000000000, 0.8660254037844387076, 1.000000000000000000, 0.8660254037844387076, 1.000000000000000000, 0.8660254037844387076, 1.000000000000000000, 0.8660254037844387076, 1.000000000000000000, 0.8660254037844387076, 1.000000000000000000, 0.8660254037844387076, 1.000000000000000000, 0.8660254037844387076, 1.000000000000000000, 0.8660254037844387076, 1.000000000000000000, 0.8660254037844387076, 1.000000000000000000, 0.8660254037844387076, 1.000000000000000000, 0.8660254037844387076, 1.000000000000000000, 0.8660254037844387076, 1.000000000000000000, 0.8660254037844387076, 1.000000000000000000, 0.8660254037844387076, 1.000000000000000000, 0.8660254037844387076, 1.000000000000000000, 0.8660254037844387076, 1.000000000000000000, 0.8660254037844387076, 1.000000000000000000, 0.8660254037844387076, 1.000000000000000000, 0.8660254037844387076, 1.000000000000000000, 0.8660254037844387076, 1.000000000000000000, 0.8660254037844387076, 1.000000000000000000, 0.8660254037844387076, 1.000000000000000000, 0.8660254037844387076, 1.000000000000000000, 0.8660254037844387076, 1.000000000000000000, 0.8660254037844387076, 1.000000000000000000, 0.8660254037844387076, 1.000000000000000000, 0.8660254037844387076, 1.000000000000000000, 0.8660254037844387076, 1.000000000000000000, 0.8660254037844387076, 1.000000000000000000, 0.8660254037844387076, 1.000000000000000000, 0.8660254037844387076, 1.000000000000000000, 0.8660254037844387076, 1.000000000000000000, 0.8660254037844387076, 1.000000000000000000, 0.8660254037844387076, 1.000000000000000000, 0.8660254037844387076, 1.000000000000000000, 0.8660254037844387076, 1.000000000000000000, 0.8660254037844387076, 1.000000000000000000, 0.8660254037844387076, 1.000000000000000000, 0.8660254037844387076, 1.000000000000000000, 0.8660254037844387076, 1.000000000000000000, 0.8660254037844387076, 1.000000000000000000, 0.8660254037844387076, 1.000000000000000000, 0.8660254037844387076, 1.000000000000000000, 0.8660254037844387076, 1.000000000000000000, 0.8660254037844387076, 1.000000000000000000, 0.8660254037844387076, 1.000000000000000000, 0.8660254037844387076, 1.000000000000000000, 0.8660254037844387076, 1.000000000000000000, 0.8660254037844387076, 1.000000000000000000, 0.8660254037844387076, 1.000000000000000000, 0.8660254037844387076, 1.000000000000000000, 0.8660254037844387076, 1.000000000000000000, 0.8660254037844387076, 1.000000000000000000, 0.8660254037844387076, 1.000000000000000000, 0.8660254037844387076, 1.000000000000000000, 0.8660254037844387076, 1.000000000000000000, 0.8660254037844387076, 1.000000000000000000) ) ) 
 REPRESENTATION_ITEM ( '' )  SURFACE ( )  );
#24032 = CARTESIAN_POINT ( 'NONE',  ( 14.74687500061451573, -3.027376345333610441, -5.243569643749999898 ) ) ;
#24033 = CARTESIAN_POINT ( 'NONE',  ( 10.80000000122903536, -2.886751345948129988, 4.999999999999997335 ) ) ;
#24034 = CARTESIAN_POINT ( 'NONE',  ( 16.77187500061451786, 3.027376345333611329, 5.243569643749999010 ) ) ;
#24035 = CARTESIAN_POINT ( 'NONE',  ( 18.56250000000000000, 2.886751345948129099, -4.999999999999998224 ) ) ;
#24036 = CARTESIAN_POINT ( 'NONE',  ( 9.046875000614518214, 6.054752690667223547, 3.707466751127219781E-16 ) ) ;
#24037 = CARTESIAN_POINT ( 'NONE',  ( 9.001249775931846008E-16, 10.91562500061451857, -25.09994784771203058 ) ) ;
#24038 = CARTESIAN_POINT ( 'NONE',  ( 3.999999999999999112, 16.62500000000000000, 30.00000000000000000 ) ) ;
#24039 = CARTESIAN_POINT ( 'NONE',  ( 23.63437500061451502, -2.746126346562641984, -4.756430356249999214 ) ) ;
#24040 = CYLINDRICAL_SURFACE ( 'NONE', #51281, 4.999999999999998224 ) ;
#24041 = CARTESIAN_POINT ( 'NONE',  ( 25.11562500061451431, 3.027376345333613106, -5.243569643749998122 ) ) ;
#24043 = ADVANCED_FACE ( 'NONE', ( #51783 ), #41069, .F. ) ;
#24042 = CARTESIAN_POINT ( 'NONE',  ( 26.55000000000000071, -4.330127018922190985, -2.500000000000001332 ) ) ;
#24044 = CARTESIAN_POINT ( 'NONE',  ( 28.39687500061452141, 6.054752690667223547, 3.707466751127219781E-16 ) ) ;
#24045 = CARTESIAN_POINT ( 'NONE',  ( 23.77499999999999858, -4.330127018922194537, 2.499999999999995559 ) ) ;
#24046 = ADVANCED_FACE ( 'NONE', ( #56595 ), #12970, .T. ) ;
#24047 =( BOUNDED_CURVE ( )  B_SPLINE_CURVE ( 3, ( #44175, #60774, #15342, #5372 ),
 .UNSPECIFIED., .F., .F. ) 
 B_SPLINE_CURVE_WITH_KNOTS ( ( 4, 4 ),
 ( 0.9384417405046960869, 1.570796326794896780 ),
 .UNSPECIFIED. ) 
 CURVE ( )  GEOMETRIC_REPRESENTATION_ITEM ( )  RATIONAL_B_SPLINE_CURVE ( ( 1.000000000000000000, 0.9669539835197179523, 0.9669539835197179523, 1.000000000000000000 ) ) 
 REPRESENTATION_ITEM ( '' )  );
#24048 = CARTESIAN_POINT ( 'NONE',  ( 7.640625000614517326, 6.054752690667223547, 3.707466751127219781E-16 ) ) ;
#24049 = CARTESIAN_POINT ( 'NONE',  ( 24.23437500061451644, 5.492252693125287522, 3.363034840372157021E-16 ) ) ;
#24050 = CARTESIAN_POINT ( 'NONE',  ( 18.34687500061451715, -3.027376345333610441, -5.243569643749999898 ) ) ;
#24051 = CARTESIAN_POINT ( 'NONE',  ( 11.93437500061451750, -2.746126346562641984, -4.756430356249999214 ) ) ;
#24052 = CARTESIAN_POINT ( 'NONE',  ( 3.290625000614516793, -3.027376345333614438, 5.243569643749998122 ) ) ;
#24053 = CARTESIAN_POINT ( 'NONE',  ( 9.459375000614517859, 4.541064518000418104, -2.621784821874998173 ) ) ;
#24054 = ORIENTED_EDGE ( 'NONE', *, *, #11775, .T. ) ;
#24055 = CARTESIAN_POINT ( 'NONE',  ( 19.92187500061451644, 3.027376345333611329, 5.243569643749999010 ) ) ;
#24056 = CARTESIAN_POINT ( 'NONE',  ( 8.043750001229032165, -2.886751345948130876, 4.999999999999996447 ) ) ;
#24057 = CARTESIAN_POINT ( 'NONE',  ( 26.43750000000000000, -2.886751345948129988, 4.999999999999997335 ) ) ;
#24058 = CARTESIAN_POINT ( 'NONE',  ( 3.712499999999999911, 2.886751345948129099, -4.999999999999998224 ) ) ;
#24059 = CARTESIAN_POINT ( 'NONE',  ( 29.73749999999999716, -2.886751345948115777, -5.000000000000017764 ) ) ;
#24060 = CARTESIAN_POINT ( 'NONE',  ( 15.82499999999999929, 6.123233995736764310E-16, -4.999999999999998224 ) ) ;
#24061 = ORIENTED_EDGE ( 'NONE', *, *, #54124, .T. ) ;
#24062 = CARTESIAN_POINT ( 'NONE',  ( 10.08749999999999858, 5.773502691896255534, 3.535250795749688894E-16 ) ) ;
#24063 = CARTESIAN_POINT ( 'NONE',  ( 12.27187500061451608, -4.119189519843968306, 2.378215178124996054 ) ) ;
#24064 = CARTESIAN_POINT ( 'NONE',  ( 23.99062500061451786, -3.027376345333614438, 5.243569643749998122 ) ) ;
#24065 = CARTESIAN_POINT ( 'NONE',  ( 13.08750000000000036, -2.886751345948125991, -5.000000000000000000 ) ) ;
#24066 = EDGE_CURVE ( 'NONE', #29126, #23351, #56245, .T. ) ;
#24067 = CARTESIAN_POINT ( 'NONE',  ( 8.212500001229035007, -4.330127018922190985, -2.500000000000001332 ) ) ;
#24068 = CARTESIAN_POINT ( 'NONE',  ( 6.478125000614516793, -4.541064518000419881, 2.621784821874995952 ) ) ;
#24069 = CARTESIAN_POINT ( 'NONE',  ( 22.19999999999999574, 4.330127018922192761, -2.499999999999997780 ) ) ;
#24070 = CARTESIAN_POINT ( 'NONE',  ( 19.75312500061451360, 4.541064518000418104, -2.621784821874998173 ) ) ;
#24071 = CARTESIAN_POINT ( 'NONE',  ( 45.00000000000000000, 0.000000000000000000, 0.000000000000000000 ) ) ;
#24072 = CARTESIAN_POINT ( 'NONE',  ( 25.27500000122903145, -5.773502691896255534, -1.060575238724906372E-15 ) ) ;
#24073 = CARTESIAN_POINT ( 'NONE',  ( -1.878215178125001827, 17.89062499938548356, 33.25316411605952283 ) ) ;
#24074 = CARTESIAN_POINT ( 'NONE',  ( 4.500000000000000888, -4.330127018922190985, -2.500000000000001332 ) ) ;
#24075 = ORIENTED_EDGE ( 'NONE', *, *, #12791, .F. ) ;
#24076 = CARTESIAN_POINT ( 'NONE',  ( 22.71562500061451573, -6.054752690667223547, -1.112240025338166033E-15 ) ) ;
#24077 = CARTESIAN_POINT ( 'NONE',  ( 3.422429900546629877, -3.645130117820770455, -3.769356580772429410 ) ) ;
#24078 = CARTESIAN_POINT ( 'NONE',  ( 27.57187500061451857, 3.027376345333611329, 5.243569643749999010 ) ) ;
#24079 = CARTESIAN_POINT ( 'NONE',  ( 14.76562500061451821, 3.027376345333613106, -5.243569643749998122 ) ) ;
#24080 = CARTESIAN_POINT ( 'NONE',  ( 7.500000000000000000, 0.000000000000000000, 4.999999999999998224 ) ) ;
#24081 = CARTESIAN_POINT ( 'NONE',  ( 27.30000000122903359, 5.773502691896255534, 3.535250795749688894E-16 ) ) ;
#24082 = CARTESIAN_POINT ( 'NONE',  ( 21.49687500061451573, -2.746126346562641984, -4.756430356249999214 ) ) ;
#24083 = CARTESIAN_POINT ( 'NONE',  ( 16.41562500061451857, -6.054752690667223547, -1.112240025338166033E-15 ) ) ;
#24084 = CARTESIAN_POINT ( 'NONE',  ( -1.626862140677534273E-15, 15.53750000000000142, 34.00000000000000000 ) ) ;
#24085 = CARTESIAN_POINT ( 'NONE',  ( 6.000000001229031987, -2.886751345948126435, -5.000000000000000000 ) ) ;
#24086 = CARTESIAN_POINT ( 'NONE',  ( 12.49687500061451573, -3.027376345333610441, -5.243569643749999898 ) ) ;
#24087 = CARTESIAN_POINT ( 'NONE',  ( 11.07187500061451679, -6.054752690667223547, -1.112240025338166033E-15 ) ) ;
#24088 = CARTESIAN_POINT ( 'NONE',  ( 20.52187500061451786, -6.054752690667223547, -1.112240025338166033E-15 ) ) ;
#24089 = EDGE_LOOP ( 'NONE', ( #10180, #57904, #36336, #6323 ) ) ;
#24090 = CARTESIAN_POINT ( 'NONE',  ( 0.000000000000000000, 10.00000000000000000, 24.00000000000000000 ) ) ;
#24091 = CARTESIAN_POINT ( 'NONE',  ( 23.24062500061451786, -3.027376345333610441, -5.243569643749999898 ) ) ;
#24092 = CARTESIAN_POINT ( 'NONE',  ( 18.68437500061451928, -4.541064518000419881, 2.621784821874995952 ) ) ;
#24093 = CARTESIAN_POINT ( 'NONE',  ( 23.91562500061451502, 3.027376345333611329, 5.243569643749999010 ) ) ;
#24094 = CARTESIAN_POINT ( 'NONE',  ( 0.000000000000000000, 20.00000000000000000, 24.00000000000000000 ) ) ;
#24095 = CARTESIAN_POINT ( 'NONE',  ( 8.484601909799253346E-16, 15.16250000000000142, 34.61880215351700230 ) ) ;
#24096 = AXIS2_PLACEMENT_3D ( 'NONE', #5520, #28058, #50586 ) ;
#24097 = CARTESIAN_POINT ( 'NONE',  ( 29.50312500061451360, -4.541064518000417216, -2.621784821875001281 ) ) ;
#24098 = CARTESIAN_POINT ( 'NONE',  ( 8.662500001229034297, -4.330127018922190985, -2.500000000000001332 ) ) ;
#24099 = CARTESIAN_POINT ( 'NONE',  ( 4.687500001229034652, 6.123233995736764310E-16, -4.999999999999998224 ) ) ;
#24100 = CARTESIAN_POINT ( 'NONE',  ( 21.33749999999999858, 5.773502691896255534, 3.535250795749688401E-16 ) ) ;
#24101 = CARTESIAN_POINT ( 'NONE',  ( 27.75000000122903288, 5.773502691896255534, 3.535250795749688894E-16 ) ) ;
#24102 = CARTESIAN_POINT ( 'NONE',  ( -1.878215178124999163, 13.80312499938548321, 26.74683588394047007 ) ) ;
#24103 = CARTESIAN_POINT ( 'NONE',  ( 10.32187500061451679, 3.027376345333613106, -5.243569643749998122 ) ) ;
#24104 = CARTESIAN_POINT ( 'NONE',  ( 10.03125000122903288, 6.123233995736764310E-16, -4.999999999999998224 ) ) ;
#24105 = CARTESIAN_POINT ( 'NONE',  ( 17.01562500061451644, 3.027376345333613106, -5.243569643749998122 ) ) ;
#24106 = CARTESIAN_POINT ( 'NONE',  ( 10.09687500061451715, -3.027376345333614438, 5.243569643749998122 ) ) ;
#24107 = CARTESIAN_POINT ( 'NONE',  ( 2.953125000614516438, -4.541064518000417216, -2.621784821875001281 ) ) ;
#24108 = CARTESIAN_POINT ( 'NONE',  ( 18.87187500061452283, 3.027376345333612662, -5.243569643749998122 ) ) ;
#24109 = CARTESIAN_POINT ( 'NONE',  ( 7.471875000614519813, -6.054752690667223547, -1.112240025338166033E-15 ) ) ;
#24110 = CARTESIAN_POINT ( 'NONE',  ( 2.878125000614517592, -4.541064518000419881, 2.621784821874995952 ) ) ;
#24111 = CARTESIAN_POINT ( 'NONE',  ( -2.498395430326213790E-14, 16.66250000000000497, 26.00000000000000000 ) ) ;
#24112 = CARTESIAN_POINT ( 'NONE',  ( 8.053125000614516082, 4.541064518000418104, -2.621784821874998173 ) ) ;
#24113 = CARTESIAN_POINT ( 'NONE',  ( 17.87812500061451715, 6.421520780324663323E-16, -5.243569643749999010 ) ) ;
#24114 = EDGE_LOOP ( 'NONE', ( #60862, #38345, #56700, #23689 ) ) ;
#24115 = CARTESIAN_POINT ( 'NONE',  ( 6.675000001229034474, 2.886751345948126879, 4.999999999999999112 ) ) ;
#24116 = CARTESIAN_POINT ( 'NONE',  ( 15.51562500061451644, -6.054752690667223547, -1.112240025338166033E-15 ) ) ;
#24117 = CARTESIAN_POINT ( 'NONE',  ( 12.06562500061451537, 3.027376345333613106, -5.243569643749998122 ) ) ;
#24118 = CARTESIAN_POINT ( 'NONE',  ( 23.67187500061451999, -5.492252693125287522, -1.008910452111647106E-15 ) ) ;
#24119 = CARTESIAN_POINT ( 'NONE',  ( 12.75000000000000178, 4.330127018922192761, -2.499999999999997780 ) ) ;
#24120 = CARTESIAN_POINT ( 'NONE',  ( 5.550000001229032698, -2.886751345948125991, -5.000000000000000000 ) ) ;
#24121 = CARTESIAN_POINT ( 'NONE',  ( 29.21249999999999858, -5.773502691896255534, -1.060575238724906372E-15 ) ) ;
#24122 = CARTESIAN_POINT ( 'NONE',  ( 15.19687500061451857, -3.027376345333610441, -5.243569643749999898 ) ) ;
#24123 = CARTESIAN_POINT ( 'NONE',  ( 17.55000000122903359, -2.886751345948129988, 4.999999999999997335 ) ) ;
#24124 = CARTESIAN_POINT ( 'NONE',  ( 25.38749999999999929, 5.773502691896255534, 3.535250795749688894E-16 ) ) ;
#24125 = CARTESIAN_POINT ( 'NONE',  ( 4.243569643749999010, 19.16562500061451857, -32.45002607614398471 ) ) ;
#24126 = CARTESIAN_POINT ( 'NONE',  ( 8.437500000000000000, -2.886751345948130876, 4.999999999999996447 ) ) ;
#24127 = CARTESIAN_POINT ( 'NONE',  ( 23.51250000122903216, -4.330127018922190985, -2.500000000000001332 ) ) ;
#24128 = CYLINDRICAL_SURFACE ( 'NONE', #25724, 15.00000000000000000 ) ;
#24129 = CYLINDRICAL_SURFACE ( 'NONE', #13693, 4.999999999999998224 ) ;
#24130 = CARTESIAN_POINT ( 'NONE',  ( 19.50937500061451857, 0.000000000000000000, 5.243569643749999010 ) ) ;
#24131 = CARTESIAN_POINT ( 'NONE',  ( 21.52500000122903145, 2.886751345948126879, 4.999999999999998224 ) ) ;
#24132 = EDGE_CURVE ( 'NONE', #36091, #16314, #17775, .T. ) ;
#24133 = CARTESIAN_POINT ( 'NONE',  ( 13.41562500061451502, 3.027376345333613106, -5.243569643749998122 ) ) ;
#24134 = CARTESIAN_POINT ( 'NONE',  ( 8.343750001229034652, 5.773502691896255534, 3.535250795749688894E-16 ) ) ;
#24135 = CARTESIAN_POINT ( 'NONE',  ( 26.70937500061451431, 0.000000000000000000, 5.243569643749999010 ) ) ;
#24136 = CARTESIAN_POINT ( 'NONE',  ( 17.25937500061451502, -5.492252693125287522, -1.008910452111647106E-15 ) ) ;
#24137 = CARTESIAN_POINT ( 'NONE',  ( 9.365625000614519635, 3.027376345333613106, -5.243569643749998122 ) ) ;
#24138 = CARTESIAN_POINT ( 'NONE',  ( 14.74687500061451573, -3.027376345333610441, -5.243569643749999898 ) ) ;
#24139 = ORIENTED_EDGE ( 'NONE', *, *, #70290, .T. ) ;
#24140 = CARTESIAN_POINT ( 'NONE',  ( 28.00312500061451715, 0.000000000000000000, 5.243569643749999010 ) ) ;
#24141 = CARTESIAN_POINT ( 'NONE',  ( 19.45312500061451644, 0.000000000000000000, 5.243569643749999010 ) ) ;
#24142 = CARTESIAN_POINT ( 'NONE',  ( 29.54062500061451502, -3.027376345333610441, -5.243569643749999898 ) ) ;
#24143 = CARTESIAN_POINT ( 'NONE',  ( -3.137519842735245283E-14, 14.71250000000000213, 34.00000000000000000 ) ) ;
#24144 = CARTESIAN_POINT ( 'NONE',  ( 10.61250000000000071, 2.886751345948126879, 4.999999999999999112 ) ) ;
#24145 = CARTESIAN_POINT ( 'NONE',  ( 18.30000000122903359, 5.773502691896255534, 3.535250795749688894E-16 ) ) ;
#24146 = CARTESIAN_POINT ( 'NONE',  ( 23.28750000122903430, 4.330127018922191873, 2.499999999999999556 ) ) ;
#24147 = CARTESIAN_POINT ( 'NONE',  ( 10.69687500061451679, 4.119189519843966529, -2.378215178124998275 ) ) ;
#24148 = VERTEX_POINT ( 'NONE', #51422 ) ;
#24149 = CARTESIAN_POINT ( 'NONE',  ( 16.83749999999999858, 5.773502691896255534, 3.535250795749688894E-16 ) ) ;
#24150 = CARTESIAN_POINT ( 'NONE',  ( 21.78750000000000142, 5.773502691896255534, 3.535250795749688894E-16 ) ) ;
#24151 = CARTESIAN_POINT ( 'NONE',  ( 20.18437500061451573, 6.421520780324663323E-16, -5.243569643749999010 ) ) ;
#24152 = CARTESIAN_POINT ( 'NONE',  ( 25.52812500061451573, 6.421520780324663323E-16, -5.243569643749999010 ) ) ;
#24154 = EDGE_LOOP ( 'NONE', ( #31043, #69915, #17069, #60763 ) ) ;
#24153 = VECTOR ( 'NONE', #53142, 1000.000000000000000 ) ;
#24155 = DIRECTION ( 'NONE',  ( 0.000000000000000000, 0.000000000000000000, -1.000000000000000000 ) ) ;
#24156 = CARTESIAN_POINT ( 'NONE',  ( 4.978125000614518569, 4.541064518000418104, 2.621784821874999949 ) ) ;
#24157 = CARTESIAN_POINT ( 'NONE',  ( 3.159375000614518036, 4.541064518000418104, -2.621784821874998173 ) ) ;
#24158 = CARTESIAN_POINT ( 'NONE',  ( 12.63749999999999929, -2.886751345948125991, -5.000000000000000000 ) ) ;
#24159 = CARTESIAN_POINT ( 'NONE',  ( -2.121784821874996840, 17.17812500061451786, 33.67503911421598417 ) ) ;
#24160 = CARTESIAN_POINT ( 'NONE',  ( 28.07812500061451289, -4.541064518000419881, 2.621784821874995952 ) ) ;
#24161 = CARTESIAN_POINT ( 'NONE',  ( 10.08749999999999858, 5.773502691896255534, 3.535250795749688894E-16 ) ) ;
#24162 = AXIS2_PLACEMENT_3D ( 'NONE', #11879, #18488, #35132 ) ;
#24163 = CARTESIAN_POINT ( 'NONE',  ( 3.756430356249998770, 17.55312499938548143, 32.16877607737302469 ) ) ;
#24164 = CARTESIAN_POINT ( 'NONE',  ( 26.18437500061451573, 4.541064518000418104, 2.621784821874999949 ) ) ;
#24165 = ORIENTED_EDGE ( 'NONE', *, *, #56240, .F. ) ;
#24166 = CARTESIAN_POINT ( 'NONE',  ( 22.67812500061451431, -4.541064518000419881, 2.621784821874995952 ) ) ;
#24167 = CARTESIAN_POINT ( 'NONE',  ( 22.88437500061451857, 6.421520780324663323E-16, -5.243569643749999010 ) ) ;
#24168 = CARTESIAN_POINT ( 'NONE',  ( -4.243569643749998122, 15.79062500061459495, -27.54997392385601174 ) ) ;
#24169 = CARTESIAN_POINT ( 'NONE',  ( 6.140625000614516438, -3.027376345333610441, -5.243569643749999898 ) ) ;
#24170 = CARTESIAN_POINT ( 'NONE',  ( 3.727827348360245097, 3.332161949968362347, -3.727827348360304605 ) ) ;
#24171 = CARTESIAN_POINT ( 'NONE',  ( 24.66562500061451502, 3.027376345333612662, -5.243569643749998122 ) ) ;
#24172 = CARTESIAN_POINT ( 'NONE',  ( 28.62187500061451217, 5.824947211148865298E-16, -4.756430356249998326 ) ) ;
#24173 = CARTESIAN_POINT ( 'NONE',  ( 11.97187500061451892, -5.492252693125287522, -1.008910452111647106E-15 ) ) ;
#24174 = CARTESIAN_POINT ( 'NONE',  ( 17.07187500061451502, 3.027376345333613106, -5.243569643749998122 ) ) ;
#24175 = CARTESIAN_POINT ( 'NONE',  ( 19.20937500061451786, -4.541064518000417216, -2.621784821875001281 ) ) ;
#24176 = CARTESIAN_POINT ( 'NONE',  ( 27.57187500061451857, 3.027376345333611329, 5.243569643749999010 ) ) ;
#24177 = CARTESIAN_POINT ( 'NONE',  ( 9.001249775931846008E-16, 16.82187500061451857, 34.90005215228797653 ) ) ;
#24178 = CARTESIAN_POINT ( 'NONE',  ( 8.353125000614518569, -4.541064518000417216, -2.621784821875001281 ) ) ;
#24179 = CARTESIAN_POINT ( 'NONE',  ( -3.999999999999999112, 19.09999999999999787, 30.00000000000000000 ) ) ;
#24180 = CARTESIAN_POINT ( 'NONE',  ( 5.296875000614518214, -3.027376345333610441, -5.243569643749999898 ) ) ;
#24181 = FACE_OUTER_BOUND ( 'NONE', #20140, .T. ) ;
#24182 = CARTESIAN_POINT ( 'NONE',  ( 4.153125000614515727, 0.000000000000000000, 5.243569643749999010 ) ) ;
#24183 = CARTESIAN_POINT ( 'NONE',  ( 10.47187500061451715, 3.027376345333611329, 5.243569643749999010 ) ) ;
#24184 = CARTESIAN_POINT ( 'NONE',  ( 17.58750000122903145, -4.330127018922194537, 2.499999999999995559 ) ) ;
#24185 = CARTESIAN_POINT ( 'NONE',  ( 4.584375000614516971, 4.541064518000418104, 2.621784821874999949 ) ) ;
#24186 = CARTESIAN_POINT ( 'NONE',  ( 7.753125000614518036, 0.000000000000000000, 5.243569643749999010 ) ) ;
#24187 = DIRECTION ( 'NONE',  ( 0.000000000000000000, 6.195440985631455317E-17, 1.000000000000000000 ) ) ;
#24188 = CARTESIAN_POINT ( 'NONE',  ( 24.61875000122903501, 2.886751345948126879, 4.999999999999999112 ) ) ;
#24189 = CARTESIAN_POINT ( 'NONE',  ( 16.73437500061451644, 4.541064518000418104, 2.621784821874999949 ) ) ;
#24190 = CARTESIAN_POINT ( 'NONE',  ( 30.00000000000000000, 0.000000000000000000, 0.000000000000000000 ) ) ;
#24191 = ORIENTED_EDGE ( 'NONE', *, *, #65091, .F. ) ;
#24192 = CARTESIAN_POINT ( 'NONE',  ( 24.62812500061451715, 6.421520780324663323E-16, -5.243569643749999010 ) ) ;
#24193 = CARTESIAN_POINT ( 'NONE',  ( 10.71562500061451928, 3.027376345333613106, -5.243569643749998122 ) ) ;
#24194 = CARTESIAN_POINT ( 'NONE',  ( 27.49687500061451573, 6.054752690667223547, 3.707466751127219781E-16 ) ) ;
#24195 = CARTESIAN_POINT ( 'NONE',  ( 9.290625000614515017, -3.027376345333610441, -5.243569643749999898 ) ) ;
#24196 = CARTESIAN_POINT ( 'NONE',  ( 2.121784821875001281, 10.10937500061451821, -26.32496088578401938 ) ) ;
#24197 = CARTESIAN_POINT ( 'NONE',  ( 11.62500000122903465, 2.886751345948126879, 4.999999999999999112 ) ) ;
#24198 = EDGE_CURVE ( 'NONE', #65361, #25555, #25332, .T. ) ;
#24199 = CARTESIAN_POINT ( 'NONE',  ( 24.89062500061451644, -3.027376345333614438, 5.243569643749998122 ) ) ;
#24200 = CARTESIAN_POINT ( 'NONE',  ( 9.001249775931846008E-16, 14.06562500061451715, -25.09994784771203058 ) ) ;
#24201 = CARTESIAN_POINT ( 'NONE',  ( 13.31250000122903288, 4.330127018922192761, -2.499999999999997780 ) ) ;
#24202 = CARTESIAN_POINT ( 'NONE',  ( 22.00312500061451360, 4.541064518000418104, -2.621784821874998173 ) ) ;
#24203 = VECTOR ( 'NONE', #27208, 1000.000000000000000 ) ;
#24204 = CARTESIAN_POINT ( 'NONE',  ( 10.23750000000000071, -2.886751345948129988, 4.999999999999997335 ) ) ;
#24205 = CARTESIAN_POINT ( 'NONE',  ( 20.84062500061451573, -3.027376345333614438, 5.243569643749998122 ) ) ;
#24206 = CARTESIAN_POINT ( 'NONE',  ( 5.184375000614516615, -4.541064518000419881, 2.621784821874995952 ) ) ;
#24207 = CARTESIAN_POINT ( 'NONE',  ( 21.03750000000000142, -2.886751345948129988, 4.999999999999997335 ) ) ;
#24208 = CARTESIAN_POINT ( 'NONE',  ( 14.88750000122903394, -4.330127018922194537, 2.499999999999995559 ) ) ;
#24209 = VECTOR ( 'NONE', #2362, 1000.000000000000000 ) ;
#24210 = CARTESIAN_POINT ( 'NONE',  ( 9.328125000614518214, 6.421520780324663323E-16, -5.243569643749999010 ) ) ;
#24211 = CARTESIAN_POINT ( 'NONE',  ( 16.07812500061451289, 6.421520780324663323E-16, -5.243569643749999010 ) ) ;
#24212 = AXIS2_PLACEMENT_3D ( 'NONE', #42382, #32385, #13930 ) ;
#24213 = CARTESIAN_POINT ( 'NONE',  ( 25.91250000122903074, 4.330127018922192761, -2.499999999999997780 ) ) ;
#24214 = VECTOR ( 'NONE', #14266, 1000.000000000000000 ) ;
#24215 = CARTESIAN_POINT ( 'NONE',  ( 22.50937500061451857, 4.541064518000418104, -2.621784821874998173 ) ) ;
#24216 = CARTESIAN_POINT ( 'NONE',  ( 22.21875000122903288, 2.886751345948101122, -5.000000000000046185 ) ) ;
#24217 = EDGE_CURVE ( 'NONE', #34631, #10555, #65473, .T. ) ;
#24218 = CARTESIAN_POINT ( 'NONE',  ( 8.550000001229031810, -2.886751345948129988, 4.999999999999997335 ) ) ;
#24219 = CARTESIAN_POINT ( 'NONE',  ( 9.646875000614516082, -3.027376345333614438, 5.243569643749998122 ) ) ;
#24220 = CARTESIAN_POINT ( 'NONE',  ( 24.98437500061451644, -4.541064518000419881, 2.621784821874995952 ) ) ;
#24221 = CARTESIAN_POINT ( 'NONE',  ( 23.85000000000000142, -4.330127018922190985, -2.500000000000001332 ) ) ;
#24222 = CARTESIAN_POINT ( 'NONE',  ( 22.07812500061451644, 4.541064518000418104, 2.621784821874999949 ) ) ;
#24223 = CARTESIAN_POINT ( 'NONE',  ( 27.57187500061451857, 3.027376345333611329, 5.243569643749999010 ) ) ;
#24224 = CARTESIAN_POINT ( 'NONE',  ( 1.878215178124997609, 17.62812499938548427, 33.25316411605952993 ) ) ;
#24225 = DIRECTION ( 'NONE',  ( -0.000000000000000000, -1.000000000000000000, -0.000000000000000000 ) ) ;
#24226 = CARTESIAN_POINT ( 'NONE',  ( 8.859375000614518214, -4.541064518000417216, -2.621784821875001281 ) ) ;
#24227 = CARTESIAN_POINT ( 'NONE',  ( 20.05312500061451431, -4.541064518000417216, -2.621784821875001281 ) ) ;
#24228 = VERTEX_POINT ( 'NONE', #23331 ) ;
#24229 = DIRECTION ( 'NONE',  ( -1.000000000000000000, -0.000000000000000000, -0.000000000000000000 ) ) ;
#24230 = CARTESIAN_POINT ( 'NONE',  ( 26.91562500061451146, 3.027376345333613106, -5.243569643749998122 ) ) ;
#24231 = CARTESIAN_POINT ( 'NONE',  ( 3.571875000614517237, 3.027376345333613106, -5.243569643749998122 ) ) ;
#24232 = CARTESIAN_POINT ( 'NONE',  ( 4.898587196589411843E-16, 20.00000000000000000, -26.00000000000000000 ) ) ;
#24233 = DIRECTION ( 'NONE',  ( -0.000000000000000000, -1.000000000000000000, -0.000000000000000000 ) ) ;
#24234 = CARTESIAN_POINT ( 'NONE',  ( 16.12500000000000000, -4.330127018922194537, 2.499999999999995559 ) ) ;
#24235 = CARTESIAN_POINT ( 'NONE',  ( 20.31562500061451715, 3.027376345333611329, 5.243569643749999010 ) ) ;
#24236 = VERTEX_POINT ( 'NONE', #63220 ) ;
#24237 = CARTESIAN_POINT ( 'NONE',  ( 25.31250000000000000, 2.886751345948129099, -4.999999999999998224 ) ) ;
#24238 = EDGE_CURVE ( 'NONE', #63984, #30207, #71097, .T. ) ;
#24239 = CARTESIAN_POINT ( 'NONE',  ( 26.74687500061451573, -3.027376345333614438, 5.243569643749998122 ) ) ;
#24240 = ORIENTED_EDGE ( 'NONE', *, *, #66190, .T. ) ;
#24241 = CARTESIAN_POINT ( 'NONE',  ( 13.45312500061451466, 4.541064518000418104, -2.621784821874998173 ) ) ;
#24242 = CARTESIAN_POINT ( 'NONE',  ( 4.940625000614515372, 6.054752690667223547, 3.707466751127219781E-16 ) ) ;
#24243 = CARTESIAN_POINT ( 'NONE',  ( 18.42187500061451644, 4.119189519843966529, 2.378215178124999607 ) ) ;
#24244 = CARTESIAN_POINT ( 'NONE',  ( 29.12812500061451715, 6.421520780324663323E-16, -5.243569643749999010 ) ) ;
#24245 = CARTESIAN_POINT ( 'NONE',  ( 16.27500000122903501, -5.773502691896255534, -1.060575238724906372E-15 ) ) ;
#24246 = AXIS2_PLACEMENT_3D ( 'NONE', #47923, #2483, #53089 ) ;
#24247 = CARTESIAN_POINT ( 'NONE',  ( 20.85000000000000142, 4.330127018922192761, -2.499999999999997780 ) ) ;
#24248 = CARTESIAN_POINT ( 'NONE',  ( 28.35000000000000142, -4.330127018922190985, -2.500000000000001332 ) ) ;
#24249 = CARTESIAN_POINT ( 'NONE',  ( 5.409375000614516260, 4.541064518000418104, -2.621784821874998173 ) ) ;
#24250 = CARTESIAN_POINT ( 'NONE',  ( 9.946875000614516793, 6.054752690667223547, 3.707466751127219781E-16 ) ) ;
#24251 = CARTESIAN_POINT ( 'NONE',  ( 18.53437500061451715, 4.541064518000418104, 2.621784821874999949 ) ) ;
#24252 = LINE ( 'NONE', #39817, #50135 ) ;
#24253 = VERTEX_POINT ( 'NONE', #25890 ) ;
#24254 = CARTESIAN_POINT ( 'NONE',  ( 2.934375000614518392, -4.541064518000419881, 2.621784821874995952 ) ) ;
#24255 = CARTESIAN_POINT ( 'NONE',  ( 3.975000000000002753, -4.330127018922194537, 2.499999999999995559 ) ) ;
#24256 = CARTESIAN_POINT ( 'NONE',  ( 5.034375000614519813, 4.541064518000418104, 2.621784821874999949 ) ) ;
#24257 = CARTESIAN_POINT ( 'NONE',  ( 17.81250000000000355, 2.886751345948126879, 4.999999999999999112 ) ) ;
#24258 = CARTESIAN_POINT ( 'NONE',  ( 13.45312500061451466, 4.541064518000418104, -2.621784821874998173 ) ) ;
#24259 = CARTESIAN_POINT ( 'NONE',  ( 1.999999999999998668, 14.11250000122903359, 26.53589838486224650 ) ) ;
#24260 = CARTESIAN_POINT ( 'NONE',  ( 20.40000000122903145, -2.886751345948125991, -5.000000000000000000 ) ) ;
#24261 = CARTESIAN_POINT ( 'NONE',  ( -1.999999999999997113, 13.43750000122903465, 33.46410161513775705 ) ) ;
#24262 = CARTESIAN_POINT ( 'NONE',  ( 19.32187500061451857, 2.746126346562645981, -4.756430356249997438 ) ) ;
#24263 = CARTESIAN_POINT ( 'NONE',  ( 6.853125000614516793, 0.000000000000000000, 5.243569643749999010 ) ) ;
#24264 = CARTESIAN_POINT ( 'NONE',  ( 24.15937500061451715, -4.541064518000417216, -2.621784821875001281 ) ) ;
#24265 = CARTESIAN_POINT ( 'NONE',  ( 27.15000000122902435, -2.886751345948092684, -5.000000000000057732 ) ) ;
#24266 = CARTESIAN_POINT ( 'NONE',  ( 26.22187500061451715, 3.027376345333611329, 5.243569643749999010 ) ) ;
#24267 = CARTESIAN_POINT ( 'NONE',  ( 6.412500000000001421, 2.886751345948129099, -4.999999999999998224 ) ) ;
#24268 = CARTESIAN_POINT ( 'NONE',  ( -3.999999999999997335, 12.50000000122903465, 32.30940107675850470 ) ) ;
#24269 = CARTESIAN_POINT ( 'NONE',  ( 15.32812500061451644, 4.541064518000418104, 2.621784821874999949 ) ) ;
#24271 =( BOUNDED_CURVE ( )  B_SPLINE_CURVE ( 2, ( #4627, #27157, #38971, #60381, #16055, #72219, #61129 ),
 .UNSPECIFIED., .F., .F. ) 
 B_SPLINE_CURVE_WITH_KNOTS ( ( 3, 2, 2, 3 ),
 ( 0.09999999999999995004, 0.1033333333333332771, 0.1066666666666666041, 0.1099999999999999312 ),
 .UNSPECIFIED. ) 
 CURVE ( )  GEOMETRIC_REPRESENTATION_ITEM ( )  RATIONAL_B_SPLINE_CURVE ( ( 1.000000000000002220, 0.8660254037844364872, 1.000000000000000000, 0.8660254037844387076, 1.000000000000000000, 0.8660254037844414832, 0.9999999999999972244 ) ) 
 REPRESENTATION_ITEM ( '' )  );
#24270 = CARTESIAN_POINT ( 'NONE',  ( 7.650000001229034119, -2.886751345948129988, 4.999999999999997335 ) ) ;
#24272 = CARTESIAN_POINT ( 'NONE',  ( 17.74687500061451928, -3.027376345333614438, 5.243569643749998122 ) ) ;
#24273 = CARTESIAN_POINT ( 'NONE',  ( 11.82187500061451679, 3.027376345333611329, 5.243569643749999010 ) ) ;
#24274 = DIRECTION ( 'NONE',  ( 0.000000000000000000, 0.000000000000000000, 1.000000000000000000 ) ) ;
#24275 = ORIENTED_EDGE ( 'NONE', *, *, #1251, .T. ) ;
#24276 = CARTESIAN_POINT ( 'NONE',  ( 11.57812500061451644, 6.421520780324663323E-16, -5.243569643749999010 ) ) ;
#24277 = VECTOR ( 'NONE', #13989, 1000.000000000000000 ) ;
#24278 = CARTESIAN_POINT ( 'NONE',  ( 4.000000000000000000, 12.20000000122903394, -27.69059892324149885 ) ) ;
#24279 = CARTESIAN_POINT ( 'NONE',  ( 24.41250000122903430, -4.330127018922190985, -2.500000000000001332 ) ) ;
#24280 = CARTESIAN_POINT ( 'NONE',  ( 12.19687500061451679, 6.054752690667223547, 3.707466751127219781E-16 ) ) ;
#24281 = CARTESIAN_POINT ( 'NONE',  ( 14.05312500061451431, 0.000000000000000000, 5.243569643749999010 ) ) ;
#24282 = CARTESIAN_POINT ( 'NONE',  ( 4.000000000000000000, 18.83749999999999858, -27.69059892324149885 ) ) ;
#24283 = CARTESIAN_POINT ( 'NONE',  ( 23.29687500061451644, -3.027376345333610441, -5.243569643749999898 ) ) ;
#24284 = CARTESIAN_POINT ( 'NONE',  ( 8.474999999999999645, -4.330127018922194537, 2.499999999999995559 ) ) ;
#24285 = CARTESIAN_POINT ( 'NONE',  ( 5.400000000000002132, -4.330127018922190985, -2.500000000000001332 ) ) ;
#24286 = CARTESIAN_POINT ( 'NONE',  ( 14.84999999999999964, -4.330127018922190985, -2.500000000000001332 ) ) ;
#24287 = CARTESIAN_POINT ( 'NONE',  ( 4.243569643749999898, 16.48437500061451644, -30.00000000000000000 ) ) ;
#24288 = CARTESIAN_POINT ( 'NONE',  ( 15.64687500061451608, -3.027376345333610441, -5.243569643749999898 ) ) ;
#24289 = CARTESIAN_POINT ( 'NONE',  ( 17.47500000122903430, 2.886751345948126879, 4.999999999999999112 ) ) ;
#24290 = CARTESIAN_POINT ( 'NONE',  ( 13.28437500061451715, -4.541064518000419881, 2.621784821874995952 ) ) ;
#24291 = CARTESIAN_POINT ( 'NONE',  ( -4.243569643749999898, 19.31562500061451715, -32.45002607614398471 ) ) ;
#24292 = CARTESIAN_POINT ( 'NONE',  ( 20.06250000122903643, 4.330127018922192761, -2.499999999999997780 ) ) ;
#24293 = CARTESIAN_POINT ( 'NONE',  ( 15.92812500061451608, -4.541064518000419881, 2.621784821874995952 ) ) ;
#24294 = ORIENTED_EDGE ( 'NONE', *, *, #25301, .F. ) ;
#24295 = ORIENTED_EDGE ( 'NONE', *, *, #68559, .F. ) ;
#24296 = CARTESIAN_POINT ( 'NONE',  ( 19.20000000000000284, 0.000000000000000000, 4.999999999999998224 ) ) ;
#24297 = DIRECTION ( 'NONE',  ( 1.000000000000000000, 0.000000000000000000, -0.000000000000000000 ) ) ;
#24298 = CARTESIAN_POINT ( 'NONE',  ( 12.53437500061451537, 6.421520780324663323E-16, -5.243569643749999010 ) ) ;
#24299 = CARTESIAN_POINT ( 'NONE',  ( 3.035814067847288467, 3.972922589466866938, -3.271563712840051874 ) ) ;
#24300 = CARTESIAN_POINT ( 'NONE',  ( 12.52500000122903145, 2.886751345948126879, 4.999999999999999112 ) ) ;
#24301 = CARTESIAN_POINT ( 'NONE',  ( 19.95000000122903572, -2.886751345948125991, -5.000000000000000000 ) ) ;
#24302 = CARTESIAN_POINT ( 'NONE',  ( 19.07812500061451644, -4.541064518000419881, 2.621784821874995952 ) ) ;
#24303 = EDGE_CURVE ( 'NONE', #18738, #47145, #70211, .T. ) ;
#24304 = CARTESIAN_POINT ( 'NONE',  ( 23.54062500061451146, -3.027376345333614438, 5.243569643749998122 ) ) ;
#24305 = CARTESIAN_POINT ( 'NONE',  ( 3.215625000614518836, 3.027376345333611329, 5.243569643749999010 ) ) ;
#24306 = CARTESIAN_POINT ( 'NONE',  ( 27.78749999999999787, -2.886751345948129988, 4.999999999999997335 ) ) ;
#24307 = CARTESIAN_POINT ( 'NONE',  ( 27.84375000122903288, -2.886751345948137093, 4.999999999999984901 ) ) ;
#24308 = AXIS2_PLACEMENT_3D ( 'NONE', #48841, #25938, #59536 ) ;
#24309 = CARTESIAN_POINT ( 'NONE',  ( 9.796875000614519990, -2.746126346562642428, -4.756430356249999214 ) ) ;
#24310 = CARTESIAN_POINT ( 'NONE',  ( 4.080569135018654592, -2.889455923578380769, -4.080569135022440896 ) ) ;
#24311 = CARTESIAN_POINT ( 'NONE',  ( -4.243569643749999898, 16.70937500061451786, -30.00000000000000000 ) ) ;
#24312 = CARTESIAN_POINT ( 'NONE',  ( 3.900000001229034563, 5.773502691896255534, 3.535250795749688894E-16 ) ) ;
#24313 = CARTESIAN_POINT ( 'NONE',  ( 5.587500000000003020, 5.773502691896255534, 3.535250795749688894E-16 ) ) ;
#24314 = CARTESIAN_POINT ( 'NONE',  ( 10.80937500061451928, 4.541064518000418104, -2.621784821874998173 ) ) ;
#24315 = CARTESIAN_POINT ( 'NONE',  ( 28.64062500061451289, -3.027376345333610441, -5.243569643749999898 ) ) ;
#24316 = CARTESIAN_POINT ( 'NONE',  ( 45.00000000000000000, 0.000000000000000000, 0.000000000000000000 ) ) ;
#24317 = CARTESIAN_POINT ( 'NONE',  ( -4.384844337767558109, 8.988619951912522055, -34.09994685707254547 ) ) ;
#24318 = DIRECTION ( 'NONE',  ( 1.000000000000000000, 0.000000000000000000, 0.000000000000000000 ) ) ;
#24319 = CARTESIAN_POINT ( 'NONE',  ( 8.221875000614518925, 3.027376345333611329, 5.243569643749999010 ) ) ;
#24320 = CARTESIAN_POINT ( 'NONE',  ( 11.10937500061451644, -4.541064518000417216, -2.621784821875001281 ) ) ;
#24321 = CARTESIAN_POINT ( 'NONE',  ( 7.237500000000000711, -2.886751345948125991, -5.000000000000000000 ) ) ;
#24322 = CARTESIAN_POINT ( 'NONE',  ( 4.243569643749999898, 15.52812500061459566, 30.00000000000000000 ) ) ;
#24323 = CARTESIAN_POINT ( 'NONE',  ( 4.875000000000000888, -4.330127018922194537, 2.499999999999995559 ) ) ;
#24324 = CARTESIAN_POINT ( 'NONE',  ( 6.712500000000000355, -5.773502691896255534, -1.060575238724906372E-15 ) ) ;
#24325 = CARTESIAN_POINT ( 'NONE',  ( 14.40937500061451537, 2.746126346562643317, 4.756430356249998326 ) ) ;
#24326 = CARTESIAN_POINT ( 'NONE',  ( 22.45312500061451644, 4.541064518000418104, -2.621784821874998173 ) ) ;
#24327 = CARTESIAN_POINT ( 'NONE',  ( 13.22812500061451502, -4.541064518000419881, 2.621784821874995952 ) ) ;
#24328 = CARTESIAN_POINT ( 'NONE',  ( 25.65937500061451360, 2.746126346562643317, 4.756430356249998326 ) ) ;
#24329 = CARTESIAN_POINT ( 'NONE',  ( 8.484375000614518214, 6.421520780324663323E-16, -5.243569643749999010 ) ) ;
#24330 = CARTESIAN_POINT ( 'NONE',  ( 26.36249999999999716, 2.886751345948126879, 4.999999999999999112 ) ) ;
#24331 = CARTESIAN_POINT ( 'NONE',  ( 23.58750000122903145, 6.123233995736764310E-16, -4.999999999999998224 ) ) ;
#24332 = CARTESIAN_POINT ( 'NONE',  ( 4.898587196589411843E-16, 20.00000000000000000, -26.00000000000000000 ) ) ;
#24333 = CARTESIAN_POINT ( 'NONE',  ( 12.90937500061451537, -4.541064518000417216, -2.621784821875001281 ) ) ;
#24334 = CARTESIAN_POINT ( 'NONE',  ( 25.88437500061451502, -4.541064518000419881, 2.621784821874995952 ) ) ;
#24335 = CARTESIAN_POINT ( 'NONE',  ( 3.796875000614517326, -3.027376345333614438, 5.243569643749998122 ) ) ;
#24336 = EDGE_CURVE ( 'NONE', #18463, #44824, #60649, .T. ) ;
#24337 = CARTESIAN_POINT ( 'NONE',  ( 0.000000000000000000, 20.00000000000000000, 26.00000000000000000 ) ) ;
#24338 = CARTESIAN_POINT ( 'NONE',  ( 19.54687500061451644, -3.027376345333614438, 5.243569643749998122 ) ) ;
#24339 = CARTESIAN_POINT ( 'NONE',  ( 12.49687500061451573, -3.027376345333610441, -5.243569643749999898 ) ) ;
#24340 = CARTESIAN_POINT ( 'NONE',  ( -7.967954043666661671E-16, 19.39062499938548001, 34.33755215474603517 ) ) ;
#24341 = CARTESIAN_POINT ( 'NONE',  ( 24.67500000000000071, -4.330127018922194537, 2.499999999999995559 ) ) ;
#24342 = CARTESIAN_POINT ( 'NONE',  ( 1.999999999999997335, 13.77500000000000036, 33.46410161513775705 ) ) ;
#24343 = CARTESIAN_POINT ( 'NONE',  ( 4.243569643749999010, 11.12187500061451928, -32.45002607614398471 ) ) ;
#24344 = CARTESIAN_POINT ( 'NONE',  ( 27.87187500061451573, 2.746126346562645981, -4.756430356249997438 ) ) ;
#24345 = CARTESIAN_POINT ( 'NONE',  ( 13.67812500061451786, -4.541064518000419881, 2.621784821874995952 ) ) ;
#24346 = CARTESIAN_POINT ( 'NONE',  ( 5.362500000000003375, -5.773502691896255534, -1.060575238724906372E-15 ) ) ;
#24347 = CYLINDRICAL_SURFACE ( 'NONE', #11328, 4.000000000000000000 ) ;
#24348 = CARTESIAN_POINT ( 'NONE',  ( 45.00000000000000000, 0.000000000000000000, 4.999999999999998224 ) ) ;
#24349 = CARTESIAN_POINT ( 'NONE',  ( 13.87500000000000178, -4.330127018922194537, 2.499999999999995559 ) ) ;
#24350 = CARTESIAN_POINT ( 'NONE',  ( 2.121784821874999061, 10.20312500061451821, 26.32496088578401583 ) ) ;
#24351 = CARTESIAN_POINT ( 'NONE',  ( 13.35000000122903430, 5.773502691896255534, 3.535250795749688894E-16 ) ) ;
#24352 = CARTESIAN_POINT ( 'NONE',  ( 25.39687500061451431, -3.027376345333614438, 5.243569643749998122 ) ) ;
#24353 = AXIS2_PLACEMENT_3D ( 'NONE', #66488, #15867, #38415 ) ;
#24354 = ORIENTED_EDGE ( 'NONE', *, *, #50295, .F. ) ;
#24355 = CARTESIAN_POINT ( 'NONE',  ( 19.30312500061451786, 4.541064518000418104, -2.621784821874998173 ) ) ;
#24356 = CARTESIAN_POINT ( 'NONE',  ( 19.54687500061451644, -3.027376345333614438, 5.243569643749998122 ) ) ;
#24357 = CARTESIAN_POINT ( 'NONE',  ( 5.137500000000000178, 5.773502691896255534, 3.535250795749688894E-16 ) ) ;
#24358 = CARTESIAN_POINT ( 'NONE',  ( 7.115625000614516082, 3.027376345333613106, -5.243569643749998122 ) ) ;
#24359 = CARTESIAN_POINT ( 'NONE',  ( 21.47812500061451502, 6.421520780324663323E-16, -5.243569643749999010 ) ) ;
#24360 = CARTESIAN_POINT ( 'NONE',  ( 15.94687500061451502, -3.027376345333614438, 5.243569643749998122 ) ) ;
#24361 = CARTESIAN_POINT ( 'NONE',  ( -2.121784821874999949, 14.32812500061451644, 26.32496088578401938 ) ) ;
#24362 = CARTESIAN_POINT ( 'NONE',  ( 19.98750000122903359, 6.123233995736764310E-16, -4.999999999999998224 ) ) ;
#24363 = CARTESIAN_POINT ( 'NONE',  ( 11.55937500061451928, -4.119189519843965641, -2.378215178125001383 ) ) ;
#24364 = CARTESIAN_POINT ( 'NONE',  ( 9.890625000614514661, 6.054752690667223547, 3.707466751127219781E-16 ) ) ;
#24365 = CARTESIAN_POINT ( 'NONE',  ( 4.059375000614519280, 4.541064518000418104, -2.621784821874998173 ) ) ;
#24366 = CARTESIAN_POINT ( 'NONE',  ( 28.30312500061451431, 4.541064518000418104, -2.621784821874998173 ) ) ;
#24367 = CARTESIAN_POINT ( 'NONE',  ( 24.72187500061451360, 3.027376345333613106, -5.243569643749998122 ) ) ;
#24368 = CARTESIAN_POINT ( 'NONE',  ( 15.62812500061451537, 6.421520780324663323E-16, -5.243569643749999010 ) ) ;
#24369 = CARTESIAN_POINT ( 'NONE',  ( 25.35000000122903074, -2.886751345948125991, -5.000000000000000000 ) ) ;
#24370 = CARTESIAN_POINT ( 'NONE',  ( 24.74062500061451786, 6.054752690667223547, 3.707466751127219781E-16 ) ) ;
#24371 = CARTESIAN_POINT ( 'NONE',  ( 18.57187500061451857, 3.027376345333611329, 5.243569643749999010 ) ) ;
#24372 = CARTESIAN_POINT ( 'NONE',  ( 15.74062500061451608, 6.054752690667223547, 3.707466751127219781E-16 ) ) ;
#24373 = CARTESIAN_POINT ( 'NONE',  ( 4.243569643749999898, 18.28437500061451715, 30.00000000000000000 ) ) ;
#24374 = CARTESIAN_POINT ( 'NONE',  ( 21.17812500061451431, 4.541064518000418104, 2.621784821874999949 ) ) ;
#24375 = CARTESIAN_POINT ( 'NONE',  ( 2.887500001229035274, 6.123233995736764310E-16, -4.999999999999998224 ) ) ;
#24376 = ORIENTED_EDGE ( 'NONE', *, *, #53010, .F. ) ;
#24377 = CARTESIAN_POINT ( 'NONE',  ( 24.63749999999999574, -2.886751345948129988, 4.999999999999997335 ) ) ;
#24378 = CARTESIAN_POINT ( 'NONE',  ( 8.484601909799253346E-16, 10.66250000000000142, -25.38119784648299770 ) ) ;
#24379 = CARTESIAN_POINT ( 'NONE',  ( 1.878215178125000495, 20.02812499938548285, 26.74683588394047007 ) ) ;
#24380 = CARTESIAN_POINT ( 'NONE',  ( 28.71562500061451573, 3.027376345333613106, -5.243569643749998122 ) ) ;
#24381 = CARTESIAN_POINT ( 'NONE',  ( 7.565625000614518036, 3.027376345333613106, -5.243569643749998122 ) ) ;
#24382 = CARTESIAN_POINT ( 'NONE',  ( 23.32500000122903572, 2.886751345948126879, 4.999999999999999112 ) ) ;
#24383 = EDGE_CURVE ( 'NONE', #40816, #14839, #17354, .T. ) ;
#24384 = CARTESIAN_POINT ( 'NONE',  ( 27.25312500061451360, -4.541064518000417216, -2.621784821875001281 ) ) ;
#24385 = CARTESIAN_POINT ( 'NONE',  ( 25.34999999999999787, 4.330127018922192761, -2.499999999999997780 ) ) ;
#24386 = CARTESIAN_POINT ( 'NONE',  ( -1.999999999999997113, 16.13750000122903216, -26.53589838486224295 ) ) ;
#24387 = CARTESIAN_POINT ( 'NONE',  ( 29.61562500061451431, 3.027376345333613106, -5.243569643749998122 ) ) ;
#24388 = CARTESIAN_POINT ( 'NONE',  ( 9.815625000614518925, 3.027376345333613106, -5.243569643749998122 ) ) ;
#24389 = ORIENTED_EDGE ( 'NONE', *, *, #66002, .F. ) ;
#24390 = CARTESIAN_POINT ( 'NONE',  ( 25.71562500061451573, 3.027376345333611329, 5.243569643749999010 ) ) ;
#24391 = CARTESIAN_POINT ( 'NONE',  ( 7.678125000614516082, 4.541064518000418104, 2.621784821874999949 ) ) ;
#24392 = CARTESIAN_POINT ( 'NONE',  ( 4.565625000614516260, 3.027376345333611329, 5.243569643749999010 ) ) ;
#24393 = VECTOR ( 'NONE', #3973, 1000.000000000000000 ) ;
#24394 = CARTESIAN_POINT ( 'NONE',  ( 16.17187500061451644, 2.746126346562645981, -4.756430356249997438 ) ) ;
#24395 = FACE_OUTER_BOUND ( 'NONE', #34091, .T. ) ;
#24396 = CARTESIAN_POINT ( 'NONE',  ( 14.17500000000000071, 4.330127018922191873, 2.499999999999999556 ) ) ;
#24397 = CARTESIAN_POINT ( 'NONE',  ( 13.32187500061451502, -6.054752690667223547, -1.112240025338166033E-15 ) ) ;
#24398 = CARTESIAN_POINT ( 'NONE',  ( 8.850000001229034297, 5.773502691896255534, 3.535250795749688894E-16 ) ) ;
#24399 = CARTESIAN_POINT ( 'NONE',  ( 17.93437500061451928, 6.421520780324663323E-16, -5.243569643749999010 ) ) ;
#24400 = CARTESIAN_POINT ( 'NONE',  ( 16.38749999999999929, 5.773502691896255534, 3.535250795749688894E-16 ) ) ;
#24401 = CARTESIAN_POINT ( 'NONE',  ( 7.471875000614519813, -6.054752690667223547, -1.112240025338166033E-15 ) ) ;
#24402 = CARTESIAN_POINT ( 'NONE',  ( 4.243569643749999898, 11.02812500061451750, -30.00000000000000000 ) ) ;
#24403 = CARTESIAN_POINT ( 'NONE',  ( 7.462499999999999467, 2.886751345948193936, 4.999999999999883649 ) ) ;
#24404 = CARTESIAN_POINT ( 'NONE',  ( 23.18437500061451573, -2.746126346562641984, -4.756430356249999214 ) ) ;
#24405 = CARTESIAN_POINT ( 'NONE',  ( 26.17500000000000071, 6.123233995736764310E-16, -4.999999999999998224 ) ) ;
#24406 = CARTESIAN_POINT ( 'NONE',  ( 23.69062500061451004, -3.027376345333610441, -5.243569643749999898 ) ) ;
#24407 = CARTESIAN_POINT ( 'NONE',  ( -3.999999999999999112, 17.37500000122903288, 27.69059892324149885 ) ) ;
#24408 = CARTESIAN_POINT ( 'NONE',  ( 27.38437500061451857, 6.421520780324663323E-16, -5.243569643749999010 ) ) ;
#24409 =( BOUNDED_CURVE ( )  B_SPLINE_CURVE ( 2, ( #43744, #26756, #38566, #43381, #55196, #4590, #61090 ),
 .UNSPECIFIED., .F., .F. ) 
 B_SPLINE_CURVE_WITH_KNOTS ( ( 3, 2, 2, 3 ),
 ( 0.7833333333333334370, 0.7861111111111112049, 0.7888888888888888618, 0.7916666666666666297 ),
 .UNSPECIFIED. ) 
 CURVE ( )  GEOMETRIC_REPRESENTATION_ITEM ( )  RATIONAL_B_SPLINE_CURVE ( ( 0.9999999999999946709, 0.8660254037844440367, 1.000000000000000000, 0.8660254037844387076, 1.000000000000000000, 0.8660254037844387076, 1.000000000000000000 ) ) 
 REPRESENTATION_ITEM ( '' )  );
#24410 = CARTESIAN_POINT ( 'NONE',  ( 20.99999999999999645, 0.000000000000000000, 4.999999999999998224 ) ) ;
#24411 = CARTESIAN_POINT ( 'NONE',  ( 7.715625000614515727, 3.027376345333611329, 5.243569643749999010 ) ) ;
#24412 = CARTESIAN_POINT ( 'NONE',  ( 25.99687500061451573, 4.119189519843966529, -2.378215178124998275 ) ) ;
#24413 = CARTESIAN_POINT ( 'NONE',  ( 15.87187500061451573, 3.027376345333611329, 5.243569643749999010 ) ) ;
#24414 = CARTESIAN_POINT ( 'NONE',  ( 9.459375000614519635, 2.746126346562643317, 4.756430356249998326 ) ) ;
#24415 = CARTESIAN_POINT ( 'NONE',  ( 4.003125000614518925, 4.541064518000418104, -2.621784821874998173 ) ) ;
#24416 = CARTESIAN_POINT ( 'NONE',  ( 7.546875000614517326, -3.027376345333610441, -5.243569643749999898 ) ) ;
#24417 = VERTEX_POINT ( 'NONE', #59121 ) ;
#24418 = CARTESIAN_POINT ( 'NONE',  ( 20.22187500061451715, 3.027376345333613106, -5.243569643749998122 ) ) ;
#24419 = CARTESIAN_POINT ( 'NONE',  ( 21.56250000000000000, -5.773502691896255534, -1.060575238724906372E-15 ) ) ;
#24420 = CARTESIAN_POINT ( 'NONE',  ( 26.73749999999999716, 5.773502691896255534, 3.535250795749688894E-16 ) ) ;
#24421 = CARTESIAN_POINT ( 'NONE',  ( 28.39687500061452141, 6.054752690667223547, 3.707466751127219781E-16 ) ) ;
#24422 = CARTESIAN_POINT ( 'NONE',  ( 19.20000000000000284, 0.000000000000000000, 4.999999999999998224 ) ) ;
#24423 = CARTESIAN_POINT ( 'NONE',  ( 27.75000000000000000, 0.000000000000000000, 4.999999999999998224 ) ) ;
#24424 = ORIENTED_EDGE ( 'NONE', *, *, #33157, .F. ) ;
#24425 = CARTESIAN_POINT ( 'NONE',  ( 9.899999999999998579, -4.330127018922190985, -2.500000000000001332 ) ) ;
#24426 = CARTESIAN_POINT ( 'NONE',  ( 10.65937500061451892, 2.746126346562645981, -4.756430356249997438 ) ) ;
#24427 = CARTESIAN_POINT ( 'NONE',  ( 23.01562500061451644, 3.027376345333611329, 5.243569643749999010 ) ) ;
#24428 = CARTESIAN_POINT ( 'NONE',  ( 14.02499999999999858, 6.123233995736764310E-16, -4.999999999999998224 ) ) ;
#24429 = CARTESIAN_POINT ( 'NONE',  ( 7.350000001229033408, -2.886751345948125991, -5.000000000000000000 ) ) ;
#24430 = CARTESIAN_POINT ( 'NONE',  ( 6.365625000614518747, 3.027376345333611329, 5.243569643749999010 ) ) ;
#24431 = CARTESIAN_POINT ( 'NONE',  ( 22.72499999999999787, 4.330127018922191873, 2.499999999999999556 ) ) ;
#24432 = CARTESIAN_POINT ( 'NONE',  ( 21.92812500061451431, 6.421520780324663323E-16, -5.243569643749999010 ) ) ;
#24433 = CARTESIAN_POINT ( 'NONE',  ( 12.18749999999999822, -2.886751345948193048, -4.999999999999883649 ) ) ;
#24434 = CARTESIAN_POINT ( 'NONE',  ( 24.63750000122903216, 4.330127018922191873, 2.499999999999999556 ) ) ;
#24435 = CARTESIAN_POINT ( 'NONE',  ( -1.878215178125001827, 16.99062499938548498, 33.25316411605952283 ) ) ;
#24436 = CARTESIAN_POINT ( 'NONE',  ( 5.475000000000000533, 6.123233995736764310E-16, -4.999999999999998224 ) ) ;
#24437 = VERTEX_POINT ( 'NONE', #70587 ) ;
#24438 = CARTESIAN_POINT ( 'NONE',  ( 21.66562500061451502, 3.027376345333611329, 5.243569643749999010 ) ) ;
#24439 = CARTESIAN_POINT ( 'NONE',  ( 27.55312500061451786, 0.000000000000000000, 5.243569643749999010 ) ) ;
#24440 = CARTESIAN_POINT ( 'NONE',  ( 28.09687500061451360, -3.027376345333614438, 5.243569643749998122 ) ) ;
#24441 = CARTESIAN_POINT ( 'NONE',  ( 13.97812500061451679, 4.541064518000418104, 2.621784821874999949 ) ) ;
#24442 = CARTESIAN_POINT ( 'NONE',  ( -0.7368881354385758975, 9.803648613939513368, -34.17910028561248481 ) ) ;
#24443 = AXIS2_PLACEMENT_3D ( 'NONE', #18890, #8196, #36272 ) ;
#24444 = CARTESIAN_POINT ( 'NONE',  ( 26.55000000122902648, -2.886751345948129988, 4.999999999999997335 ) ) ;
#24445 = CARTESIAN_POINT ( 'NONE',  ( 19.28437500061451360, 5.824947211148865298E-16, -4.756430356249998326 ) ) ;
#24446 = CARTESIAN_POINT ( 'NONE',  ( 16.79062500061451857, -3.027376345333614438, 5.243569643749998122 ) ) ;
#24447 = CARTESIAN_POINT ( 'NONE',  ( 3.999999999999999112, 14.48750000122903536, -30.00000000000000000 ) ) ;
#24448 = CARTESIAN_POINT ( 'NONE',  ( 3.300000001229034918, -2.886751345948125991, -5.000000000000000000 ) ) ;
#24449 = CARTESIAN_POINT ( 'NONE',  ( 10.28437500061451715, 6.421520780324663323E-16, -5.243569643749999010 ) ) ;
#24450 = CARTESIAN_POINT ( 'NONE',  ( 8.859375000614518214, -4.541064518000417216, -2.621784821875001281 ) ) ;
#24451 = CARTESIAN_POINT ( 'NONE',  ( 18.04687500061451999, 6.054752690667223547, 3.707466751127219781E-16 ) ) ;
#24452 = ORIENTED_EDGE ( 'NONE', *, *, #29897, .T. ) ;
#24453 = CARTESIAN_POINT ( 'NONE',  ( -4.384844337767561662, 8.988619951912520278, 25.90005314292746519 ) ) ;
#24454 = CARTESIAN_POINT ( 'NONE',  ( 22.94062500061451715, 6.054752690667223547, 3.707466751127219781E-16 ) ) ;
#24455 = B_SPLINE_CURVE_WITH_KNOTS ( 'NONE', 3,
 ( #58203, #64114, #24956, #19402, #41961, #64483, #36415, #53406, #58931, #2798 ),
 .UNSPECIFIED., .F., .F.,
 ( 4, 3, 3, 4 ),
 ( 2.168404344971008868E-19, 0.0001572649580503299096, 0.0003035751770480561132, 0.0004501423746267203254 ),
 .UNSPECIFIED. ) ;
#24456 = CARTESIAN_POINT ( 'NONE',  ( 18.19687500061451502, -3.027376345333614438, 5.243569643749998122 ) ) ;
#24457 = CARTESIAN_POINT ( 'NONE',  ( 22.30312500061451431, -4.541064518000417216, -2.621784821875001281 ) ) ;
#24458 = CARTESIAN_POINT ( 'NONE',  ( 30.00000000000000000, 0.000000000000000000, 4.999999999999998224 ) ) ;
#24459 = CARTESIAN_POINT ( 'NONE',  ( -1.999999999999997113, 14.67500000000000071, 33.46410161513775705 ) ) ;
#24460 = CARTESIAN_POINT ( 'NONE',  ( 3.084375000614519191, 6.421520780324663323E-16, -5.243569643749999010 ) ) ;
#24461 = CARTESIAN_POINT ( 'NONE',  ( 8.437500001229034652, 4.330127018922191873, 2.499999999999999556 ) ) ;
#24462 = VERTEX_POINT ( 'NONE', #69504 ) ;
#24463 = CARTESIAN_POINT ( 'NONE',  ( 3.412500001229032964, 4.330127018922192761, -2.499999999999997780 ) ) ;
#24464 = DIRECTION ( 'NONE',  ( 0.000000000000000000, 0.000000000000000000, 1.000000000000000000 ) ) ;
#24465 = CARTESIAN_POINT ( 'NONE',  ( 27.78750000122903074, 4.330127018922191873, 2.499999999999999556 ) ) ;
#24466 = CARTESIAN_POINT ( 'NONE',  ( -4.000000000000000000, 20.76874999877096428, 30.00000000000000000 ) ) ;
#24467 = CARTESIAN_POINT ( 'NONE',  ( 10.13437500061451679, -4.541064518000419881, 2.621784821874995952 ) ) ;
#24468 = CARTESIAN_POINT ( 'NONE',  ( 45.00000000000000000, 0.000000000000000000, 4.999999999999998224 ) ) ;
#24469 = CARTESIAN_POINT ( 'NONE',  ( 15.44062500061451537, -3.027376345333614438, 5.243569643749998122 ) ) ;
#24470 = CARTESIAN_POINT ( 'NONE',  ( 12.12187500061451573, 3.027376345333613106, -5.243569643749998122 ) ) ;
#24471 = EDGE_CURVE ( 'NONE', #39486, #63581, #5075, .T. ) ;
#24472 = CARTESIAN_POINT ( 'NONE',  ( 29.40000000122903145, -2.886751345948125991, -5.000000000000000000 ) ) ;
#24473 =( BOUNDED_CURVE ( )  B_SPLINE_CURVE ( 2, ( #54323, #70573, #14045, #2975, #8150, #31041, #30321 ),
 .UNSPECIFIED., .F., .F. ) 
 B_SPLINE_CURVE_WITH_KNOTS ( ( 3, 2, 2, 3 ),
 ( 0.2300000000000000100, 0.2333333333333333370, 0.2366666666666666363, 0.2399999999999999634 ),
 .UNSPECIFIED. ) 
 CURVE ( )  GEOMETRIC_REPRESENTATION_ITEM ( )  RATIONAL_B_SPLINE_CURVE ( ( 1.000000000000000000, 0.8660254037844387076, 1.000000000000000000, 0.8660254037844387076, 1.000000000000000000, 0.8660254037844398178, 0.9999999999999988898 ) ) 
 REPRESENTATION_ITEM ( '' )  );
#24474 = CARTESIAN_POINT ( 'NONE',  ( 18.83437500061451431, 6.421520780324663323E-16, -5.243569643749999010 ) ) ;
#24475 = CARTESIAN_POINT ( 'NONE',  ( 6.984375000614516438, -4.541064518000419881, 2.621784821874995952 ) ) ;
#24476 = CARTESIAN_POINT ( 'NONE',  ( 7.265625000614516438, 3.027376345333611329, 5.243569643749999010 ) ) ;
#24477 =( BOUNDED_CURVE ( )  B_SPLINE_CURVE ( 2, ( #66695, #66321, #61140, #10536, #21978, #9075, #31610, #6806, #33424 ),
 .UNSPECIFIED., .F., .F. ) 
 B_SPLINE_CURVE_WITH_KNOTS ( ( 3, 2, 2, 2, 3 ),
 ( 0.1195652173913043514, 0.1231884057971014551, 0.1304347826086956486, 0.1376811594202898559, 0.1413043478260869734 ),
 .UNSPECIFIED. ) 
 CURVE ( )  GEOMETRIC_REPRESENTATION_ITEM ( )  RATIONAL_B_SPLINE_CURVE ( ( 0.9330127018922194093, 0.9330127018922194093, 1.000000000000000000, 0.8660254037844387076, 1.000000000000000000, 0.8660254037844387076, 1.000000000000000000, 0.9330127018922190762, 0.9330127018922194093 ) ) 
 REPRESENTATION_ITEM ( '' )  );
#24478 = CARTESIAN_POINT ( 'NONE',  ( 17.39062500061451644, -3.027376345333610441, -5.243569643749999898 ) ) ;
#24479 = EDGE_CURVE ( 'NONE', #59218, #48662, #35140, .T. ) ;
#24480 = ORIENTED_EDGE ( 'NONE', *, *, #58454, .T. ) ;
#24481 = CARTESIAN_POINT ( 'NONE',  ( 6.150000001229033231, 5.773502691896255534, 3.535250795749688894E-16 ) ) ;
#24482 = CARTESIAN_POINT ( 'NONE',  ( 15.77812500061451573, 4.541064518000418104, 2.621784821874999949 ) ) ;
#24483 = CARTESIAN_POINT ( 'NONE',  ( 10.52812500061451750, -4.541064518000419881, 2.621784821874995952 ) ) ;
#24484 = CARTESIAN_POINT ( 'NONE',  ( 23.03437500061451715, 4.119189519843966529, 2.378215178124999607 ) ) ;
#24485 = CARTESIAN_POINT ( 'NONE',  ( 11.06250000000000000, 2.886751345948126879, 4.999999999999999112 ) ) ;
#24486 = CARTESIAN_POINT ( 'NONE',  ( 7.612500001229035362, 0.000000000000000000, 4.999999999999998224 ) ) ;
#24487 =( BOUNDED_CURVE ( )  B_SPLINE_CURVE ( 2, ( #70023, #71121, #25317, #31228, #42319, #8696, #7968 ),
 .UNSPECIFIED., .F., .T. ) 
 B_SPLINE_CURVE_WITH_KNOTS ( ( 3, 2, 2, 3 ),
 ( 0.5800000000000000711, 0.5833333333333334814, 0.5866666666666666696, 0.5899999999999999689 ),
 .UNSPECIFIED. ) 
 CURVE ( )  GEOMETRIC_REPRESENTATION_ITEM ( )  RATIONAL_B_SPLINE_CURVE ( ( 0.9999999999999955591, 0.8660254037844431485, 1.000000000000000000, 0.8660254037844387076, 1.000000000000000000, 0.8660254037844387076, 1.000000000000000000 ) ) 
 REPRESENTATION_ITEM ( '' )  );
#24488 = CARTESIAN_POINT ( 'NONE',  ( 14.55937500061451573, 0.000000000000000000, 5.243569643749999010 ) ) ;
#24489 = CARTESIAN_POINT ( 'NONE',  ( 17.32500000122903216, 2.886751345948129099, -4.999999999999998224 ) ) ;
#24490 = CARTESIAN_POINT ( 'NONE',  ( 24.14999999999999858, 0.000000000000000000, 4.999999999999998224 ) ) ;
#24491 = CARTESIAN_POINT ( 'NONE',  ( -3.000416591977282496E-16, 19.69062500061451360, -34.90005215228797653 ) ) ;
#24492 = CARTESIAN_POINT ( 'NONE',  ( 0.000000000000000000, 27.50000000000000000, 30.00000000000000000 ) ) ;
#24493 = CARTESIAN_POINT ( 'NONE',  ( 12.76875000122903536, 2.886751345948129099, -4.999999999999997335 ) ) ;
#24494 = AXIS2_PLACEMENT_3D ( 'NONE', #71894, #28282, #33448 ) ;
#24495 = LINE ( 'NONE', #2335, #9229 ) ;
#24496 = CARTESIAN_POINT ( 'NONE',  ( 3.849931240356728512, 3.190302406438068505, 3.849931240356827544 ) ) ;
#24497 = CARTESIAN_POINT ( 'NONE',  ( 18.83437500061451431, 6.421520780324663323E-16, -5.243569643749999010 ) ) ;
#24498 = CARTESIAN_POINT ( 'NONE',  ( 10.76250000122903572, 0.000000000000000000, 4.999999999999998224 ) ) ;
#24499 = CARTESIAN_POINT ( 'NONE',  ( 13.49062500061451608, 6.054752690667223547, 3.707466751127219781E-16 ) ) ;
#24500 = CARTESIAN_POINT ( 'NONE',  ( 8.831250001229033586, 4.330127018922191873, 2.499999999999999556 ) ) ;
#24501 = CARTESIAN_POINT ( 'NONE',  ( -2.498395430326213790E-14, 16.66250000000000497, 26.00000000000000000 ) ) ;
#24502 = CARTESIAN_POINT ( 'NONE',  ( 24.12187500061451217, -6.054752690667223547, -1.112240025338166033E-15 ) ) ;
#24503 = CARTESIAN_POINT ( 'NONE',  ( 18.98437500061451289, -2.746126346562646425, 4.756430356249996549 ) ) ;
#24504 = CARTESIAN_POINT ( 'NONE',  ( 10.37812500061451715, 4.541064518000418104, 2.621784821874999949 ) ) ;
#24505 = CARTESIAN_POINT ( 'NONE',  ( 15.53437500061451715, -4.541064518000419881, 2.621784821874995952 ) ) ;
#24506 = VERTEX_POINT ( 'NONE', #16253 ) ;
#24507 = CARTESIAN_POINT ( 'NONE',  ( 26.14687500061451431, 6.054752690667223547, 3.707466751127219781E-16 ) ) ;
#24508 = CARTESIAN_POINT ( 'NONE',  ( 26.35312500061451857, -4.541064518000417216, -2.621784821875001281 ) ) ;
#24509 = CARTESIAN_POINT ( 'NONE',  ( 19.34062500061451573, 6.054752690667223547, 3.707466751127219781E-16 ) ) ;
#24510 = LINE ( 'NONE', #57035, #35690 ) ;
#24511 = CARTESIAN_POINT ( 'NONE',  ( 0.000000000000000000, 20.00000000000000000, 30.00000000000000000 ) ) ;
#24512 = CARTESIAN_POINT ( 'NONE',  ( 9.337500000000000355, -2.886751345948129988, 4.999999999999997335 ) ) ;
#24513 = CARTESIAN_POINT ( 'NONE',  ( 20.51250000122903216, 4.330127018922192761, -2.499999999999997780 ) ) ;
#24514 = CARTESIAN_POINT ( 'NONE',  ( -3.999999999999999112, 18.72500000122903074, -32.30940107675850470 ) ) ;
#24515 = CARTESIAN_POINT ( 'NONE',  ( 9.646875000614514306, -4.119189519843965641, -2.378215178125001383 ) ) ;
#24516 = ORIENTED_EDGE ( 'NONE', *, *, #48942, .F. ) ;
#24517 = CARTESIAN_POINT ( 'NONE',  ( 18.37500000000000355, -4.330127018922194537, 2.499999999999995559 ) ) ;
#24518 = CARTESIAN_POINT ( 'NONE',  ( 20.24999999999999645, -4.330127018922190985, -2.500000000000001332 ) ) ;
#24519 = CARTESIAN_POINT ( 'NONE',  ( 18.72187500061451360, -6.054752690667223547, -1.112240025338166033E-15 ) ) ;
#24520 = CARTESIAN_POINT ( 'NONE',  ( 14.57812500061451644, -4.541064518000419881, 2.621784821874995952 ) ) ;
#24521 = VERTEX_POINT ( 'NONE', #37694 ) ;
#24522 = CARTESIAN_POINT ( 'NONE',  ( -1.626862140677534273E-15, 16.83124999877096428, 34.00000000000000000 ) ) ;
#24523 = CARTESIAN_POINT ( 'NONE',  ( 6.253125000614517148, 4.541064518000418104, -2.621784821874998173 ) ) ;
#24524 = CARTESIAN_POINT ( 'NONE',  ( -5.810221930991193690E-16, 15.50000000122903465, 26.00000000000000355 ) ) ;
#24525 = CARTESIAN_POINT ( 'NONE',  ( 12.93750000000000178, -2.886751345948129988, 4.999999999999997335 ) ) ;
#24526 = CARTESIAN_POINT ( 'NONE',  ( 27.42187500061451289, 4.119189519843966529, 2.378215178124999607 ) ) ;
#24527 = CARTESIAN_POINT ( 'NONE',  ( 9.001249775931846008E-16, 14.06562500061451715, 34.90005215228797653 ) ) ;
#24528 = CARTESIAN_POINT ( 'NONE',  ( 28.52812500061451573, -4.541064518000419881, 2.621784821874995952 ) ) ;
#24529 = CARTESIAN_POINT ( 'NONE',  ( 9.000000000000001776, -4.330127018922190985, -2.500000000000001332 ) ) ;
#24530 = CARTESIAN_POINT ( 'NONE',  ( 1.878215178125000495, 18.11562499938548498, 26.74683588394047007 ) ) ;
#24531 = CARTESIAN_POINT ( 'NONE',  ( 24.42187500061451999, 3.027376345333611329, 5.243569643749999010 ) ) ;
#24532 = ORIENTED_EDGE ( 'NONE', *, *, #68559, .T. ) ;
#24533 = CARTESIAN_POINT ( 'NONE',  ( 22.52812500061451573, 4.541064518000418104, 2.621784821874999949 ) ) ;
#24534 = CARTESIAN_POINT ( 'NONE',  ( 23.29687500061451644, -3.027376345333610441, -5.243569643749999898 ) ) ;
#24535 = CARTESIAN_POINT ( 'NONE',  ( 2.121784821875001281, 16.35312500061459318, -26.32496088578401938 ) ) ;
#24536 = CARTESIAN_POINT ( 'NONE',  ( 6.403125000614517504, 0.000000000000000000, 5.243569643749999010 ) ) ;
#24537 = CARTESIAN_POINT ( 'NONE',  ( 29.70937500061451431, 4.119189519843966529, -2.378215178124998275 ) ) ;
#24538 = CARTESIAN_POINT ( 'NONE',  ( 24.85312500061451502, 0.000000000000000000, 5.243569643749999010 ) ) ;
#24539 = CARTESIAN_POINT ( 'NONE',  ( 27.83437500061451075, 5.492252693125287522, 3.363034840372157021E-16 ) ) ;
#24540 = CARTESIAN_POINT ( 'NONE',  ( 9.496875000614517504, 5.492252693125287522, 3.363034840372157021E-16 ) ) ;
#24541 = CARTESIAN_POINT ( 'NONE',  ( 16.80937500061451573, 0.000000000000000000, 5.243569643749999010 ) ) ;
#24542 = CARTESIAN_POINT ( 'NONE',  ( 26.07187500061451857, 3.027376345333613106, -5.243569643749998122 ) ) ;
#24543 = CARTESIAN_POINT ( 'NONE',  ( -4.243569643749998122, 16.29687500061451644, 32.45002607614398471 ) ) ;
#24544 = CARTESIAN_POINT ( 'NONE',  ( 6.478125000614516793, -4.541064518000419881, 2.621784821874995952 ) ) ;
#24545 = CARTESIAN_POINT ( 'NONE',  ( 3.999999999999998668, 16.21250000000000213, 27.69059892324149530 ) ) ;
#24546 = CARTESIAN_POINT ( 'NONE',  ( 4.284375000614518925, -4.541064518000419881, 2.621784821874995952 ) ) ;
#24547 = CARTESIAN_POINT ( 'NONE',  ( -4.000000000000000888, 13.66250000000000142, 32.30940107675850470 ) ) ;
#24548 = CARTESIAN_POINT ( 'NONE',  ( 5.165625000614518569, -6.054752690667223547, -1.112240025338166033E-15 ) ) ;
#24549 = CARTESIAN_POINT ( 'NONE',  ( 10.39687500061451786, 6.054752690667223547, 3.707466751127219781E-16 ) ) ;
#24550 = CARTESIAN_POINT ( 'NONE',  ( 17.47500000122903430, 2.886751345948126879, 4.999999999999999112 ) ) ;
#24551 = CARTESIAN_POINT ( 'NONE',  ( 6.496875000614517504, -3.027376345333614438, 5.243569643749998122 ) ) ;
#24552 = CARTESIAN_POINT ( 'NONE',  ( 8.465625000614515727, 3.027376345333613106, -5.243569643749998122 ) ) ;
#24553 = CARTESIAN_POINT ( 'NONE',  ( 2.000000000000000444, 14.76874999877096606, 26.53589838486224650 ) ) ;
#24554 = CARTESIAN_POINT ( 'NONE',  ( 20.79375000122902861, -2.886751345948125991, -5.000000000000000000 ) ) ;
#24555 = CARTESIAN_POINT ( 'NONE',  ( 15.68437500061451573, 6.421520780324663323E-16, -5.243569643749999010 ) ) ;
#24556 = CARTESIAN_POINT ( 'NONE',  ( -3.999999999999999112, 10.55000000000000249, 30.00000000000000000 ) ) ;
#24557 = ORIENTED_EDGE ( 'NONE', *, *, #19020, .F. ) ;
#24558 = CARTESIAN_POINT ( 'NONE',  ( 25.41562500061451146, -6.054752690667223547, -1.112240025338166033E-15 ) ) ;
#24559 = CARTESIAN_POINT ( 'NONE',  ( 10.22812500061451679, 6.421520780324663323E-16, -5.243569643749999010 ) ) ;
#24560 = CARTESIAN_POINT ( 'NONE',  ( 26.93437500061451573, 6.421520780324663323E-16, -5.243569643749999010 ) ) ;
#24561 = CARTESIAN_POINT ( 'NONE',  ( 9.215625000614515727, -6.054752690667223547, -1.112240025338166033E-15 ) ) ;
#24562 = CARTESIAN_POINT ( 'NONE',  ( 23.30625000122903145, 0.000000000000000000, 4.999999999999998224 ) ) ;
#24563 = CARTESIAN_POINT ( 'NONE',  ( 9.825000001229033941, 2.886751345948126879, 4.999999999999999112 ) ) ;
#24564 = CARTESIAN_POINT ( 'NONE',  ( 24.66562500061451502, 3.027376345333613106, -5.243569643749998122 ) ) ;
#24565 = ADVANCED_FACE ( 'NONE', ( #10722 ), #21068, .T. ) ;
#24566 = CARTESIAN_POINT ( 'NONE',  ( 9.001249775931846008E-16, 13.61562500061451786, -25.09994784771203058 ) ) ;
#24567 = CARTESIAN_POINT ( 'NONE',  ( 13.57500000122903572, -5.773502691896255534, -1.060575238724906372E-15 ) ) ;
#24568 = CARTESIAN_POINT ( 'NONE',  ( 20.91562500061451502, -6.054752690667223547, -1.112240025338166033E-15 ) ) ;
#24569 = CARTESIAN_POINT ( 'NONE',  ( 17.99062500061451786, 6.054752690667223547, 3.707466751127219781E-16 ) ) ;
#24570 = CARTESIAN_POINT ( 'NONE',  ( 4.929824033517008708, 3.348239201030694723, -4.687818875421011278 ) ) ;
#24571 = CARTESIAN_POINT ( 'NONE',  ( 20.73750000000000071, -2.886751345948125991, -5.000000000000000000 ) ) ;
#24572 = CARTESIAN_POINT ( 'NONE',  ( 13.72500000122903074, 2.886751345948129099, -4.999999999999998224 ) ) ;
#24573 = CARTESIAN_POINT ( 'NONE',  ( 9.778125000614517504, 6.421520780324663323E-16, -5.243569643749999010 ) ) ;
#24574 = CARTESIAN_POINT ( 'NONE',  ( 14.54062500061451679, -3.027376345333614438, 5.243569643749998122 ) ) ;
#24575 = CARTESIAN_POINT ( 'NONE',  ( 26.85000000122903430, 5.773502691896255534, 3.535250795749688894E-16 ) ) ;
#24576 = CARTESIAN_POINT ( 'NONE',  ( 20.63437500061451857, 6.421520780324663323E-16, -5.243569643749999010 ) ) ;
#24577 = CARTESIAN_POINT ( 'NONE',  ( 45.00000000000000000, 0.000000000000000000, 0.000000000000000000 ) ) ;
#24578 = CARTESIAN_POINT ( 'NONE',  ( 7.050000001229036251, 5.773502691896255534, 3.535250795749688894E-16 ) ) ;
#24579 = CARTESIAN_POINT ( 'NONE',  ( 6.196875000614515905, -3.027376345333610441, -5.243569643749999898 ) ) ;
#24580 = CARTESIAN_POINT ( 'NONE',  ( 26.18437500061451573, 4.541064518000418104, 2.621784821874999949 ) ) ;
#24581 = DIRECTION ( 'NONE',  ( -1.000000000000000000, -0.000000000000000000, -0.000000000000000000 ) ) ;
#24582 = CARTESIAN_POINT ( 'NONE',  ( 21.36562500061451431, -6.054752690667223547, -1.112240025338166033E-15 ) ) ;
#24583 = CARTESIAN_POINT ( 'NONE',  ( 25.92187500061451999, -6.054752690667223547, -1.112240025338166033E-15 ) ) ;
#24584 = CARTESIAN_POINT ( 'NONE',  ( -1.878215178124999163, 17.85312499938548214, 26.74683588394047007 ) ) ;
#24585 = CARTESIAN_POINT ( 'NONE',  ( 7.762499999999999289, 2.886751345948018077, -5.000000000000190070 ) ) ;
#24586 = CARTESIAN_POINT ( 'NONE',  ( 6.037500001229035185, 6.123233995736764310E-16, -4.999999999999998224 ) ) ;
#24587 = CARTESIAN_POINT ( 'NONE',  ( 8.709375000614517859, 0.000000000000000000, 5.243569643749999010 ) ) ;
#24588 = CARTESIAN_POINT ( 'NONE',  ( 16.90312500061451573, -4.541064518000417216, -2.621784821875001281 ) ) ;
#24589 = VERTEX_POINT ( 'NONE', #71696 ) ;
#24590 = FACE_OUTER_BOUND ( 'NONE', #58393, .T. ) ;
#24591 = CARTESIAN_POINT ( 'NONE',  ( 27.81562500061452070, 3.027376345333613106, -5.243569643749998122 ) ) ;
#24592 = CARTESIAN_POINT ( 'NONE',  ( 4.359375000614517326, -4.541064518000417216, -2.621784821875001281 ) ) ;
#24593 = CARTESIAN_POINT ( 'NONE',  ( -1.487416814333745711E-14, 16.06250000000000000, -26.00000000000000000 ) ) ;
#24594 = CARTESIAN_POINT ( 'NONE',  ( 3.628460635209542318, 3.440231774957711153, -3.861774003208584549 ) ) ;
#24595 = CARTESIAN_POINT ( 'NONE',  ( 16.83749999999999858, 5.773502691896255534, 3.535250795749688894E-16 ) ) ;
#24596 = CARTESIAN_POINT ( 'NONE',  ( 21.10312500061451502, 4.541064518000418104, -2.621784821874998173 ) ) ;
#24597 = ORIENTED_EDGE ( 'NONE', *, *, #25641, .T. ) ;
#24598 = CARTESIAN_POINT ( 'NONE',  ( 25.98750000000000071, -2.886751345948129988, 4.999999999999997335 ) ) ;
#24599 = CARTESIAN_POINT ( 'NONE',  ( 25.43437500061451573, -4.541064518000419881, 2.621784821874995952 ) ) ;
#24600 = ADVANCED_FACE ( 'NONE', ( #20696 ), #3731, .T. ) ;
#24601 = ORIENTED_EDGE ( 'NONE', *, *, #6663, .T. ) ;
#24602 = CARTESIAN_POINT ( 'NONE',  ( 13.04062500061451502, 6.054752690667223547, 3.707466751127219781E-16 ) ) ;
#24603 = CARTESIAN_POINT ( 'NONE',  ( 5.465625000614517504, 3.027376345333611329, 5.243569643749999010 ) ) ;
#24604 = CARTESIAN_POINT ( 'NONE',  ( 16.99687500061451573, 4.119189519843966529, -2.378215178124998275 ) ) ;
#24605 = CARTESIAN_POINT ( 'NONE',  ( 3.046875000614519990, -3.027376345333610441, -5.243569643749999898 ) ) ;
#24606 = EDGE_CURVE ( 'NONE', #30066, #37881, #53177, .T. ) ;
#24607 = CARTESIAN_POINT ( 'NONE',  ( 14.70000000122903394, 5.773502691896255534, 3.535250795749688894E-16 ) ) ;
#24608 = CARTESIAN_POINT ( 'NONE',  ( 20.17499999999999716, -4.330127018922194537, 2.499999999999995559 ) ) ;
#24609 = CARTESIAN_POINT ( 'NONE',  ( 29.09999999999999787, 0.000000000000000000, 4.999999999999998224 ) ) ;
#24610 = CARTESIAN_POINT ( 'NONE',  ( 5.746875000614517504, -3.027376345333610441, -5.243569643749999898 ) ) ;
#24611 = CARTESIAN_POINT ( 'NONE',  ( 8.784375000614518925, -4.541064518000419881, 2.621784821874995952 ) ) ;
#24612 = CARTESIAN_POINT ( 'NONE',  ( 20.33437500061451786, 4.541064518000418104, 2.621784821874999949 ) ) ;
#24613 = CARTESIAN_POINT ( 'NONE',  ( -1.999999999999997113, 17.37500000000000000, -26.53589838486224295 ) ) ;
#24614 = ORIENTED_EDGE ( 'NONE', *, *, #56333, .F. ) ;
#24615 = CARTESIAN_POINT ( 'NONE',  ( 28.15312500061451573, -4.541064518000417216, -2.621784821875001281 ) ) ;
#24616 = CARTESIAN_POINT ( 'NONE',  ( 29.22187500061451715, 3.027376345333613106, -5.243569643749998122 ) ) ;
#24617 = CARTESIAN_POINT ( 'NONE',  ( 5.596875000614516260, -3.027376345333614438, 5.243569643749998122 ) ) ;
#24618 = CARTESIAN_POINT ( 'NONE',  ( 16.94999999999999929, 0.000000000000000000, 4.999999999999998224 ) ) ;
#24619 = CARTESIAN_POINT ( 'NONE',  ( 14.46562500061451750, 3.027376345333611329, 5.243569643749999010 ) ) ;
#24620 = CARTESIAN_POINT ( 'NONE',  ( 5.810221930991193690E-16, 19.81250000000000000, 26.00000000000000000 ) ) ;
#24621 = DIRECTION ( 'NONE',  ( -1.000000000000000000, -0.000000000000000000, -0.000000000000000000 ) ) ;
#24622 = CARTESIAN_POINT ( 'NONE',  ( 19.31250000122903288, 0.000000000000000000, 4.999999999999998224 ) ) ;
#24623 = DIRECTION ( 'NONE',  ( -1.000000000000000000, -0.000000000000000000, -0.000000000000000000 ) ) ;
#24624 = CARTESIAN_POINT ( 'NONE',  ( 17.89687500061451431, -2.746126346562642428, -4.756430356249999214 ) ) ;
#24625 = CARTESIAN_POINT ( 'NONE',  ( 7.603125000614517681, 4.541064518000418104, -2.621784821874998173 ) ) ;
#24626 = CARTESIAN_POINT ( 'NONE',  ( 23.74687500061451573, -3.027376345333610441, -5.243569643749999898 ) ) ;
#24627 = EDGE_CURVE ( 'NONE', #71409, #5357, #17765, .T. ) ;
#24628 = CYLINDRICAL_SURFACE ( 'NONE', #17195, 4.999999999999998224 ) ;
#24629 = CARTESIAN_POINT ( 'NONE',  ( 27.00937500061451857, 4.541064518000418104, -2.621784821874998173 ) ) ;
#24630 = CARTESIAN_POINT ( 'NONE',  ( 8.437500000000000000, -2.886751345948129988, 4.999999999999997335 ) ) ;
#24631 = CARTESIAN_POINT ( 'NONE',  ( 2.000000000000001332, 12.61250000122903536, 33.46410161513774995 ) ) ;
#24632 = CARTESIAN_POINT ( 'NONE',  ( 13.75312500061451715, -4.541064518000417216, -2.621784821875001281 ) ) ;
#24633 = CARTESIAN_POINT ( 'NONE',  ( 7.087500001229034119, 4.330127018922191873, 2.499999999999999556 ) ) ;
#24634 = CARTESIAN_POINT ( 'NONE',  ( 12.34687500061452070, -3.027376345333614438, 5.243569643749998122 ) ) ;
#24635 = CARTESIAN_POINT ( 'NONE',  ( -1.349117715399773765, 4.821506530989289274, -26.22488606966763314 ) ) ;
#24636 = ORIENTED_EDGE ( 'NONE', *, *, #1852, .T. ) ;
#24637 = CARTESIAN_POINT ( 'NONE',  ( 12.44062500061451537, -3.027376345333610441, -5.243569643749999898 ) ) ;
#24638 = CARTESIAN_POINT ( 'NONE',  ( 27.29999999999999716, 0.000000000000000000, 4.999999999999998224 ) ) ;
#24639 = CARTESIAN_POINT ( 'NONE',  ( 24.90000000122903145, -2.886751345948125991, -5.000000000000000000 ) ) ;
#24640 = CARTESIAN_POINT ( 'NONE',  ( 13.05937500061451750, 4.541064518000418104, -2.621784821874998173 ) ) ;
#24641 = CARTESIAN_POINT ( 'NONE',  ( 14.84062500061451750, 6.054752690667223547, 3.707466751127219781E-16 ) ) ;
#24642 = EDGE_CURVE ( 'NONE', #58713, #69279, #10250, .T. ) ;
#24643 = CARTESIAN_POINT ( 'NONE',  ( 4.779258346327469376, 1.469247991000700582, 4.779258346327429408 ) ) ;
#24644 = CARTESIAN_POINT ( 'NONE',  ( 24.23437500061451644, 6.421520780324663323E-16, -5.243569643749999010 ) ) ;
#24645 = CARTESIAN_POINT ( 'NONE',  ( 4.648177544792955741E-15, 14.13124999877096499, 33.99999999999999289 ) ) ;
#24646 = CARTESIAN_POINT ( 'NONE',  ( -3.999999999999997335, 19.58750000000000213, 32.30940107675850470 ) ) ;
#24647 = CARTESIAN_POINT ( 'NONE',  ( -2.121784821874996840, 14.98437500061451644, -26.32496088578401583 ) ) ;
#24648 = CARTESIAN_POINT ( 'NONE',  ( 16.20937500061451786, 4.541064518000418104, -2.621784821874998173 ) ) ;
#24649 = CARTESIAN_POINT ( 'NONE',  ( 17.66250000122903430, -4.330127018922190985, -2.500000000000001332 ) ) ;
#24650 = CARTESIAN_POINT ( 'NONE',  ( 12.60937500061451821, 4.541064518000418104, -2.621784821874998173 ) ) ;
#24651 = CARTESIAN_POINT ( 'NONE',  ( 2.121784821874999061, 10.25937500061451857, 26.32496088578401583 ) ) ;
#24652 = CARTESIAN_POINT ( 'NONE',  ( 20.10000000122903074, 5.773502691896255534, 3.535250795749688894E-16 ) ) ;
#24653 = CARTESIAN_POINT ( 'NONE',  ( 13.41562500061451502, 3.027376345333613106, -5.243569643749998122 ) ) ;
#24654 = ORIENTED_EDGE ( 'NONE', *, *, #24697, .F. ) ;
#24655 = ORIENTED_EDGE ( 'NONE', *, *, #46671, .T. ) ;
#24656 = CARTESIAN_POINT ( 'NONE',  ( 19.01249999999999929, 2.886751345948129099, -4.999999999999998224 ) ) ;
#24657 = CARTESIAN_POINT ( 'NONE',  ( 1.999999999999997335, 18.21874999877096712, 33.46410161513775705 ) ) ;
#24658 = CARTESIAN_POINT ( 'NONE',  ( 11.78437500061451892, 4.541064518000418104, 2.621784821874999949 ) ) ;
#24659 = CARTESIAN_POINT ( 'NONE',  ( 3.062382790376843467, 3.952479298030559640, -3.370876042629931568 ) ) ;
#24660 = CARTESIAN_POINT ( 'NONE',  ( 13.12500000122903288, -5.773502691896255534, -1.060575238724906372E-15 ) ) ;
#24661 = CARTESIAN_POINT ( 'NONE',  ( 21.11250000122903359, 0.000000000000000000, 4.999999999999998224 ) ) ;
#24662 = CARTESIAN_POINT ( 'NONE',  ( 17.61562500061451786, 3.027376345333611329, 5.243569643749999010 ) ) ;
#24663 = CARTESIAN_POINT ( 'NONE',  ( 21.21562500061451573, 3.027376345333611329, 5.243569643749999010 ) ) ;
#24664 = CARTESIAN_POINT ( 'NONE',  ( 29.02500000122903145, 2.886751345948129099, -4.999999999999998224 ) ) ;
#24665 = CARTESIAN_POINT ( 'NONE',  ( 28.61249999999999716, 2.886751345948126879, 4.999999999999999112 ) ) ;
#24666 = CARTESIAN_POINT ( 'NONE',  ( 2.655984681222220721E-16, 12.75312499938548427, 25.66244784525396483 ) ) ;
#24667 = CARTESIAN_POINT ( 'NONE',  ( 28.53749999999999787, 5.773502691896255534, 3.535250795749688894E-16 ) ) ;
#24668 = CARTESIAN_POINT ( 'NONE',  ( 27.23437500061451644, -4.541064518000419881, 2.621784821874995952 ) ) ;
#24669 = CARTESIAN_POINT ( 'NONE',  ( 4.016637241357584820, -2.977687906974178400, -4.152725646678794291 ) ) ;
#24670 = CARTESIAN_POINT ( 'NONE',  ( -4.243569643749997233, 14.94687500061451679, -27.54997392385601174 ) ) ;
#24671 = CARTESIAN_POINT ( 'NONE',  ( 3.112500001229034918, 0.000000000000000000, 4.999999999999998224 ) ) ;
#24672 = CARTESIAN_POINT ( 'NONE',  ( 5.775000000000002132, -4.330127018922194537, 2.499999999999995559 ) ) ;
#24673 = CARTESIAN_POINT ( 'NONE',  ( 28.81875000122903074, -5.773502691896255534, -1.060575238724906372E-15 ) ) ;
#24674 = CARTESIAN_POINT ( 'NONE',  ( 10.05937500061451750, 0.000000000000000000, 5.243569643749999010 ) ) ;
#24675 = CARTESIAN_POINT ( 'NONE',  ( 28.07812500061451289, -4.541064518000419881, 2.621784821874995952 ) ) ;
#24676 = CARTESIAN_POINT ( 'NONE',  ( 30.00000000000000000, 0.000000000000000000, 0.000000000000000000 ) ) ;
#24677 = CARTESIAN_POINT ( 'NONE',  ( -3.517994946560662139, 9.362281625417800512, -25.13577631594603190 ) ) ;
#24678 = CARTESIAN_POINT ( 'NONE',  ( 8.362500000000002487, 2.886751345948126879, 4.999999999999998224 ) ) ;
#24679 = CARTESIAN_POINT ( 'NONE',  ( 7.396875000614519635, -3.027376345333614438, 5.243569643749998122 ) ) ;
#24680 = CARTESIAN_POINT ( 'NONE',  ( 10.62187500061451928, -6.054752690667223547, -1.112240025338166033E-15 ) ) ;
#24681 = CARTESIAN_POINT ( 'NONE',  ( 4.912499999999999645, -5.773502691896255534, -1.060575238724906372E-15 ) ) ;
#24682 = CARTESIAN_POINT ( 'NONE',  ( 2.121784821874999061, 14.70312500061459460, 26.32496088578401583 ) ) ;
#24683 = CARTESIAN_POINT ( 'NONE',  ( 2.642249610956118655, 25.30481484749465793, 33.01446934944805633 ) ) ;
#24684 =( BOUNDED_CURVE ( )  B_SPLINE_CURVE ( 2, ( #12999, #35535, #58056, #1941, #24447, #46995, #69531, #72356, #61625 ),
 .UNSPECIFIED., .F., .F. ) 
 B_SPLINE_CURVE_WITH_KNOTS ( ( 3, 2, 2, 2, 3 ),
 ( 0.4891304347826087029, 0.4927536231884058204, 0.5000000000000000000, 0.5072463768115942351, 0.5108695652173913526 ),
 .UNSPECIFIED. ) 
 CURVE ( )  GEOMETRIC_REPRESENTATION_ITEM ( )  RATIONAL_B_SPLINE_CURVE ( ( 0.9330127018922194093, 0.9330127018922194093, 1.000000000000000000, 0.8660254037844387076, 1.000000000000000000, 0.8660254037844387076, 1.000000000000000000, 0.9330127018922182991, 0.9330127018922192983 ) ) 
 REPRESENTATION_ITEM ( '' )  );
#24685 = CARTESIAN_POINT ( 'NONE',  ( 7.124999999999999112, -4.330127018922194537, 2.499999999999995559 ) ) ;
#24686 = ADVANCED_FACE ( 'NONE', ( #49165 ), #65775, .F. ) ;
#24687 = CARTESIAN_POINT ( 'NONE',  ( 15.75937500061451502, 2.746126346562643317, 4.756430356249998326 ) ) ;
#24688 = CARTESIAN_POINT ( 'NONE',  ( 21.02812500061451573, 6.421520780324663323E-16, -5.243569643749999010 ) ) ;
#24689 = CARTESIAN_POINT ( 'NONE',  ( 12.92812500061451786, 6.421520780324663323E-16, -5.243569643749999010 ) ) ;
#24690 = CARTESIAN_POINT ( 'NONE',  ( 23.37187500061451573, 4.119189519843966529, 2.378215178124999607 ) ) ;
#24691 = CARTESIAN_POINT ( 'NONE',  ( 9.759375000614516793, -4.541064518000417216, -2.621784821875001281 ) ) ;
#24692 = CARTESIAN_POINT ( 'NONE',  ( 26.73749999999999716, 5.773502691896255534, 3.535250795749688894E-16 ) ) ;
#24693 = CARTESIAN_POINT ( 'NONE',  ( 22.38750000122903216, 4.330127018922191873, 2.499999999999999556 ) ) ;
#24694 = CARTESIAN_POINT ( 'NONE',  ( 28.83749999999999858, -2.886751345948149972, -4.999999999999956479 ) ) ;
#24695 = CARTESIAN_POINT ( 'NONE',  ( 11.55937500061451928, -4.541064518000417216, -2.621784821875001281 ) ) ;
#24696 = CARTESIAN_POINT ( 'NONE',  ( 25.73437500061451644, 4.541064518000418104, 2.621784821874999949 ) ) ;
#24697 = EDGE_CURVE ( 'NONE', #54370, #18194, #338, .T. ) ;
#24698 = CARTESIAN_POINT ( 'NONE',  ( 3.121875000614518836, 3.027376345333613106, -5.243569643749998122 ) ) ;
#24699 = CARTESIAN_POINT ( 'NONE',  ( -1.999999999999997113, 12.98750000122903359, -26.53589838486224295 ) ) ;
#24700 = CARTESIAN_POINT ( 'NONE',  ( 20.63437500061451857, 6.421520780324663323E-16, -5.243569643749999010 ) ) ;
#24701 = CARTESIAN_POINT ( 'NONE',  ( 12.15937500061451892, 4.541064518000418104, -2.621784821874998173 ) ) ;
#24702 = CARTESIAN_POINT ( 'NONE',  ( -1.878215178124999163, 17.40312499938548285, 26.74683588394047007 ) ) ;
#24703 = CARTESIAN_POINT ( 'NONE',  ( 22.38749999999999929, -2.886751345948129988, 4.999999999999997335 ) ) ;
#24704 = CARTESIAN_POINT ( 'NONE',  ( -3.756430356250001434, 20.55312499938548498, 32.16877607737301048 ) ) ;
#24705 = CARTESIAN_POINT ( 'NONE',  ( -4.243569643749999898, 11.75937500061451857, -30.00000000000000000 ) ) ;
#24706 = CARTESIAN_POINT ( 'NONE',  ( 27.38437500061451857, 5.824947211148865298E-16, -4.756430356249998326 ) ) ;
#24707 = CARTESIAN_POINT ( 'NONE',  ( 14.42812500061451786, 4.541064518000418104, 2.621784821874999949 ) ) ;
#24708 = CARTESIAN_POINT ( 'NONE',  ( 4.800000000000002487, 0.000000000000000000, 4.999999999999998224 ) ) ;
#24709 = EDGE_CURVE ( 'NONE', #52280, #34596, #20582, .T. ) ;
#24710 = CARTESIAN_POINT ( 'NONE',  ( -4.000000000000000888, 18.16249999999999787, 32.30940107675850470 ) ) ;
#24711 = CARTESIAN_POINT ( 'NONE',  ( -3.999999999999999112, 19.66250000122903430, -30.00000000000000000 ) ) ;
#24712 = CARTESIAN_POINT ( 'NONE',  ( 15.63749999999999751, -2.886751345948129988, 4.999999999999997335 ) ) ;
#24713 = CARTESIAN_POINT ( 'NONE',  ( -1.999999999999997113, 19.28750000122903430, 33.46410161513775705 ) ) ;
#24714 = CARTESIAN_POINT ( 'NONE',  ( 13.01250000122903394, 0.000000000000000000, 4.999999999999998224 ) ) ;
#24715 = CARTESIAN_POINT ( 'NONE',  ( 23.70937500061451786, -4.541064518000417216, -2.621784821875001281 ) ) ;
#24716 = CARTESIAN_POINT ( 'NONE',  ( -1.071796769724483234, 16.30759618943233491, -34.00000000000000711 ) ) ;
#24717 = VERTEX_POINT ( 'NONE', #11812 ) ;
#24718 = CARTESIAN_POINT ( 'NONE',  ( 18.59062500061451573, -3.027376345333614438, 5.243569643749998122 ) ) ;
#24719 = CARTESIAN_POINT ( 'NONE',  ( 3.628125000614518036, 4.541064518000418104, 2.621784821874999949 ) ) ;
#24720 = CARTESIAN_POINT ( 'NONE',  ( 18.94687500061451502, 6.054752690667223547, 3.707466751127219781E-16 ) ) ;
#24721 = CARTESIAN_POINT ( 'NONE',  ( 3.637500000000001954, -2.886751345948125991, -5.000000000000000000 ) ) ;
#24722 = CARTESIAN_POINT ( 'NONE',  ( 6.140625000614516438, -3.027376345333610441, -5.243569643749999898 ) ) ;
#24723 = CARTESIAN_POINT ( 'NONE',  ( 22.64062500061451644, -3.027376345333614438, 5.243569643749998122 ) ) ;
#24724 = CARTESIAN_POINT ( 'NONE',  ( -4.243569643749999898, 15.26562500061451644, 27.54997392385601529 ) ) ;
#24725 = CARTESIAN_POINT ( 'NONE',  ( 18.03750000122903430, -4.330127018922194537, 2.499999999999995559 ) ) ;
#24726 = CARTESIAN_POINT ( 'NONE',  ( 11.25937500061451679, 4.119189519843966529, -2.378215178124998275 ) ) ;
#24727 = CARTESIAN_POINT ( 'NONE',  ( 10.67812500061451608, 6.421520780324663323E-16, -5.243569643749999010 ) ) ;
#24728 = CARTESIAN_POINT ( 'NONE',  ( 2.896875000614518747, -3.027376345333614438, 5.243569643749998122 ) ) ;
#24729 = CARTESIAN_POINT ( 'NONE',  ( 3.346875000614518036, -3.027376345333614438, 5.243569643749998122 ) ) ;
#24730 = CARTESIAN_POINT ( 'NONE',  ( 23.18437500061451573, -4.541064518000419881, 2.621784821874995952 ) ) ;
#24731 = CARTESIAN_POINT ( 'NONE',  ( 15.25312500061451715, 4.541064518000418104, -2.621784821874998173 ) ) ;
#24732 = CARTESIAN_POINT ( 'NONE',  ( 25.46250000122903501, 4.330127018922192761, -2.499999999999997780 ) ) ;
#24733 = CARTESIAN_POINT ( 'NONE',  ( 25.45312500061451644, -4.541064518000417216, -2.621784821875001281 ) ) ;
#24734 = CARTESIAN_POINT ( 'NONE',  ( 18.30937500061451928, -4.541064518000417216, -2.621784821875001281 ) ) ;
#24735 = CARTESIAN_POINT ( 'NONE',  ( 14.16562500061451679, -6.054752690667223547, -1.112240025338166033E-15 ) ) ;
#24736 = CARTESIAN_POINT ( 'NONE',  ( -2.121784821874999949, 16.18437500061451573, 26.32496088578401938 ) ) ;
#24737 = CARTESIAN_POINT ( 'NONE',  ( 19.07812500061451644, -4.541064518000419881, 2.621784821874995952 ) ) ;
#24738 = CARTESIAN_POINT ( 'NONE',  ( 22.12500000000000000, 6.123233995736764310E-16, -4.999999999999998224 ) ) ;
#24739 = ORIENTED_EDGE ( 'NONE', *, *, #9015, .F. ) ;
#24740 = CARTESIAN_POINT ( 'NONE',  ( 24.29999999999999716, -4.330127018922190985, -2.500000000000001332 ) ) ;
#24741 = CARTESIAN_POINT ( 'NONE',  ( 4.000000000000000000, 11.18750000000000178, -27.69059892324149530 ) ) ;
#24742 = CARTESIAN_POINT ( 'NONE',  ( -1.878215178124999163, 20.10312499938548569, 26.74683588394047007 ) ) ;
#24743 = CARTESIAN_POINT ( 'NONE',  ( 27.89062500061451289, 6.054752690667223547, 3.707466751127219781E-16 ) ) ;
#24744 = CARTESIAN_POINT ( 'NONE',  ( 8.090625000614515727, 6.054752690667223547, 3.707466751127219781E-16 ) ) ;
#24745 = CARTESIAN_POINT ( 'NONE',  ( 20.43750000122903643, 6.123233995736764310E-16, -4.999999999999998224 ) ) ;
#24746 = ADVANCED_FACE ( 'NONE', ( #33971 ), #12605, .T. ) ;
#24747 = CARTESIAN_POINT ( 'NONE',  ( 24.47812500061451502, -4.541064518000419881, 2.621784821874995952 ) ) ;
#24748 = CARTESIAN_POINT ( 'NONE',  ( 24.97499999999999787, 4.330127018922191873, 2.499999999999999556 ) ) ;
#24749 = CARTESIAN_POINT ( 'NONE',  ( 3.999999999999998668, 14.97500000122903430, -32.30940107675850470 ) ) ;
#24750 = CARTESIAN_POINT ( 'NONE',  ( -3.999999999999999112, 12.46250000122903323, 30.00000000000000000 ) ) ;
#24751 = CARTESIAN_POINT ( 'NONE',  ( 9.515625000614518214, 3.027376345333611329, 5.243569643749999010 ) ) ;
#24752 = ORIENTED_EDGE ( 'NONE', *, *, #49936, .T. ) ;
#24753 = CARTESIAN_POINT ( 'NONE',  ( 25.79062500061451502, -3.027376345333614438, 5.243569643749998122 ) ) ;
#24754 = CARTESIAN_POINT ( 'NONE',  ( 4.715625000614516615, -6.054752690667223547, -1.112240025338166033E-15 ) ) ;
#24755 = CARTESIAN_POINT ( 'NONE',  ( 15.08437500061451786, -4.119189519843968306, 2.378215178124996054 ) ) ;
#24756 = VECTOR ( 'NONE', #31423, 1000.000000000000000 ) ;
#24757 = CARTESIAN_POINT ( 'NONE',  ( 17.81250000122903288, 4.330127018922192761, -2.499999999999997780 ) ) ;
#24758 = CARTESIAN_POINT ( 'NONE',  ( 14.10000000000000142, 4.330127018922192761, -2.499999999999997780 ) ) ;
#24759 = CARTESIAN_POINT ( 'NONE',  ( 13.24687500061451750, -3.027376345333614438, 5.243569643749998122 ) ) ;
#24760 = CARTESIAN_POINT ( 'NONE',  ( 9.075000001229033941, -5.773502691896255534, -1.060575238724906372E-15 ) ) ;
#24761 = CARTESIAN_POINT ( 'NONE',  ( 16.99687500061451573, -3.027376345333610441, -5.243569643749999898 ) ) ;
#24762 = CARTESIAN_POINT ( 'NONE',  ( 16.61250000000000426, -5.773502691896255534, -1.060575238724906372E-15 ) ) ;
#24763 = CARTESIAN_POINT ( 'NONE',  ( 8.746875000614515727, -3.027376345333614438, 5.243569643749998122 ) ) ;
#24764 = CARTESIAN_POINT ( 'NONE',  ( 4.243569643749999898, 12.79062500061451679, -27.54997392385601529 ) ) ;
#24765 = CARTESIAN_POINT ( 'NONE',  ( 1.626862140677534273E-15, 12.01250000000000284, -26.00000000000000355 ) ) ;
#24766 = CARTESIAN_POINT ( 'NONE',  ( 22.28437500061451360, -2.746126346562641984, -4.756430356249999214 ) ) ;
#24767 = ORIENTED_EDGE ( 'NONE', *, *, #68132, .F. ) ;
#24768 = CARTESIAN_POINT ( 'NONE',  ( 24.74062500061451786, 6.054752690667223547, 3.707466751127219781E-16 ) ) ;
#24769 = CARTESIAN_POINT ( 'NONE',  ( 21.15000000122903145, -2.886751345948130876, 4.999999999999996447 ) ) ;
#24770 = CARTESIAN_POINT ( 'NONE',  ( 25.58437500061451431, 6.421520780324663323E-16, -5.243569643749999010 ) ) ;
#24771 = CARTESIAN_POINT ( 'NONE',  ( 28.24687500061451573, -3.027376345333610441, -5.243569643749999898 ) ) ;
#24772 = CARTESIAN_POINT ( 'NONE',  ( 21.18749999999999645, -2.886751345948125991, -5.000000000000000000 ) ) ;
#24773 = CARTESIAN_POINT ( 'NONE',  ( 6.365625000614518747, 3.027376345333611329, 5.243569643749999010 ) ) ;
#24774 = CARTESIAN_POINT ( 'NONE',  ( 22.58437500061451786, -2.746126346562646425, 4.756430356249996549 ) ) ;
#24775 = CARTESIAN_POINT ( 'NONE',  ( 15.53437500061451715, -4.541064518000419881, 2.621784821874995952 ) ) ;
#24776 = CARTESIAN_POINT ( 'NONE',  ( 7.846875000614515372, -4.119189519843965641, -2.378215178125001383 ) ) ;
#24777 = CARTESIAN_POINT ( 'NONE',  ( 3.778125000614519280, -4.541064518000419881, 2.621784821874995952 ) ) ;
#24778 = CARTESIAN_POINT ( 'NONE',  ( 7.959375000614516971, -4.541064518000417216, -2.621784821875001281 ) ) ;
#24779 = CARTESIAN_POINT ( 'NONE',  ( 19.09687500061451360, -3.027376345333614438, 5.243569643749998122 ) ) ;
#24780 = CARTESIAN_POINT ( 'NONE',  ( -2.442157805219161926, 25.33991025467384972, 33.17866654912879909 ) ) ;
#24781 = CARTESIAN_POINT ( 'NONE',  ( 27.18750000000000000, 5.773502691896255534, 3.535250795749688894E-16 ) ) ;
#24782 = CARTESIAN_POINT ( 'NONE',  ( 28.13437500061451502, -4.541064518000419881, 2.621784821874995952 ) ) ;
#24783 = CARTESIAN_POINT ( 'NONE',  ( 1.071796769724491893, 10.23259618943233384, -26.00000000000000355 ) ) ;
#24784 = CARTESIAN_POINT ( 'NONE',  ( 29.39999999999999858, 4.330127018922192761, -2.499999999999997780 ) ) ;
#24785 = VERTEX_POINT ( 'NONE', #36426 ) ;
#24786 = CARTESIAN_POINT ( 'NONE',  ( 10.57500000000000107, 4.330127018922191873, 2.499999999999999556 ) ) ;
#24787 = CARTESIAN_POINT ( 'NONE',  ( 11.07187500061451679, 5.824947211148865298E-16, -4.756430356249998326 ) ) ;
#24788 = CARTESIAN_POINT ( 'NONE',  ( 22.41562500061451502, 3.027376345333613106, -5.243569643749998122 ) ) ;
#24789 = CARTESIAN_POINT ( 'NONE',  ( 11.10000000000000142, 0.000000000000000000, 4.999999999999998224 ) ) ;
#24790 = EDGE_CURVE ( 'NONE', #36195, #38197, #4289, .T. ) ;
#24791 = CARTESIAN_POINT ( 'NONE',  ( 9.300000001229035362, 5.773502691896255534, 3.535250795749688894E-16 ) ) ;
#24792 = CARTESIAN_POINT ( 'NONE',  ( 6.628125000614517148, 6.421520780324663323E-16, -5.243569643749999010 ) ) ;
#24793 = CARTESIAN_POINT ( 'NONE',  ( 22.46250000000000213, -5.773502691896255534, -1.060575238724906372E-15 ) ) ;
#24794 = CARTESIAN_POINT ( 'NONE',  ( 20.24062500061451431, 6.054752690667223547, 3.707466751127219781E-16 ) ) ;
#24795 = CARTESIAN_POINT ( 'NONE',  ( 14.73749999999999893, -2.886751345948063374, 5.000000000000112799 ) ) ;
#24796 = CARTESIAN_POINT ( 'NONE',  ( 25.12500000122903288, 2.886751345948126879, 4.999999999999999112 ) ) ;
#24797 = CARTESIAN_POINT ( 'NONE',  ( 2.655984681222220721E-16, 20.40312499938548285, 25.66244784525396483 ) ) ;
#24798 = CARTESIAN_POINT ( 'NONE',  ( 4.200000000000001954, 4.330127018922192761, -2.499999999999997780 ) ) ;
#24799 = ORIENTED_EDGE ( 'NONE', *, *, #30402, .T. ) ;
#24800 = CARTESIAN_POINT ( 'NONE',  ( 20.65312500061451573, 4.541064518000418104, -2.621784821874998173 ) ) ;
#24801 = CARTESIAN_POINT ( 'NONE',  ( 26.46562500061451573, 3.027376345333613106, -5.243569643749998122 ) ) ;
#24802 = CARTESIAN_POINT ( 'NONE',  ( 28.05937500061451573, 0.000000000000000000, 5.243569643749999010 ) ) ;
#24803 = CARTESIAN_POINT ( 'NONE',  ( 14.09062500061451750, -3.027376345333614438, 5.243569643749998122 ) ) ;
#24804 = CARTESIAN_POINT ( 'NONE',  ( 28.34062500061451928, 6.054752690667223547, 3.707466751127219781E-16 ) ) ;
#24805 = CARTESIAN_POINT ( 'NONE',  ( 9.403125000614517504, 4.541064518000418104, -2.621784821874998173 ) ) ;
#24806 = CARTESIAN_POINT ( 'NONE',  ( 26.28750000122903430, 6.123233995736764310E-16, -4.999999999999998224 ) ) ;
#24807 = CARTESIAN_POINT ( 'NONE',  ( 20.52187500061451786, -5.492252693125287522, -1.008910452111647106E-15 ) ) ;
#24808 = CARTESIAN_POINT ( 'NONE',  ( 17.80312500061451786, -4.541064518000417216, -2.621784821875001281 ) ) ;
#24809 = CARTESIAN_POINT ( 'NONE',  ( 28.59375000122903288, 5.773502691896255534, 3.535250795749688401E-16 ) ) ;
#24810 = CARTESIAN_POINT ( 'NONE',  ( 29.78437500061451715, 4.541064518000418104, 2.621784821874999949 ) ) ;
#24811 = CARTESIAN_POINT ( 'NONE',  ( 10.09687500061451715, -3.027376345333614438, 5.243569643749998122 ) ) ;
#24812 = CARTESIAN_POINT ( 'NONE',  ( 8.709375000614517859, 0.000000000000000000, 5.243569643749999010 ) ) ;
#24813 = CARTESIAN_POINT ( 'NONE',  ( 18.68437500061451928, -4.541064518000419881, 2.621784821874995952 ) ) ;
#24814 = ORIENTED_EDGE ( 'NONE', *, *, #10750, .T. ) ;
#24815 = CARTESIAN_POINT ( 'NONE',  ( 29.59687500061451715, -3.027376345333610441, -5.243569643749999898 ) ) ;
#24816 = CARTESIAN_POINT ( 'NONE',  ( 22.04062500061451502, 6.054752690667223547, 3.707466751127219781E-16 ) ) ;
#24817 = CARTESIAN_POINT ( 'NONE',  ( 15.49687500061451750, -3.027376345333614438, 5.243569643749998122 ) ) ;
#24818 = CARTESIAN_POINT ( 'NONE',  ( 22.52812500061451573, 4.541064518000418104, 2.621784821874999949 ) ) ;
#24819 = CARTESIAN_POINT ( 'NONE',  ( 2.000000000000001332, 14.75000000000000178, 33.46410161513774995 ) ) ;
#24820 = CARTESIAN_POINT ( 'NONE',  ( 29.16562500061451502, 3.027376345333613106, -5.243569643749998122 ) ) ;
#24821 = CARTESIAN_POINT ( 'NONE',  ( 9.637500001229033941, 6.123233995736764310E-16, -4.999999999999998224 ) ) ;
#24822 = ORIENTED_EDGE ( 'NONE', *, *, #39310, .F. ) ;
#24823 = CARTESIAN_POINT ( 'NONE',  ( 5.550000001229032698, -2.886751345948125991, -5.000000000000000000 ) ) ;
#24824 = CARTESIAN_POINT ( 'NONE',  ( -3.999999999999999112, 16.85000000000000142, -30.00000000000000000 ) ) ;
#24825 = CARTESIAN_POINT ( 'NONE',  ( 25.61250000122903359, 0.000000000000000000, 4.999999999999998224 ) ) ;
#24826 = CARTESIAN_POINT ( 'NONE',  ( -1.878215178125001827, 13.50312499938548427, 33.25316411605952283 ) ) ;
#24827 = CARTESIAN_POINT ( 'NONE',  ( 6.496875000614517504, -3.027376345333614438, 5.243569643749998122 ) ) ;
#24828 = CARTESIAN_POINT ( 'NONE',  ( 1.999999999999998668, 10.06250000122903465, 26.53589838486224650 ) ) ;
#24829 = CARTESIAN_POINT ( 'NONE',  ( 14.84062500061451750, 6.054752690667223547, 3.707466751127219781E-16 ) ) ;
#24830 = CARTESIAN_POINT ( 'NONE',  ( 10.13437500061451679, -4.541064518000419881, 2.621784821874995952 ) ) ;
#24831 = CARTESIAN_POINT ( 'NONE',  ( 27.63750000122903216, 6.123233995736764310E-16, -4.999999999999998224 ) ) ;
#24832 = CARTESIAN_POINT ( 'NONE',  ( 17.29687500061451999, -3.027376345333614438, 5.243569643749998122 ) ) ;
#24833 = CARTESIAN_POINT ( 'NONE',  ( 8.559375000614515727, 4.541064518000418104, -2.621784821874998173 ) ) ;
#24834 = DIRECTION ( 'NONE',  ( 0.000000000000000000, 0.000000000000000000, 1.000000000000000000 ) ) ;
#24835 = CARTESIAN_POINT ( 'NONE',  ( 8.615625000614517859, 3.027376345333611329, 5.243569643749999010 ) ) ;
#24836 = CARTESIAN_POINT ( 'NONE',  ( 17.84062500061451573, -3.027376345333610441, -5.243569643749999898 ) ) ;
#24837 = ORIENTED_EDGE ( 'NONE', *, *, #71773, .F. ) ;
#24838 = CARTESIAN_POINT ( 'NONE',  ( 14.65312500061451573, -4.541064518000417216, -2.621784821875001281 ) ) ;
#24840 = B_SPLINE_CURVE_WITH_KNOTS ( 'NONE', 3,
 ( #36978, #59500, #30706, #70234, #14075, #29978, #8913, #47697, #35522, #31444 ),
 .UNSPECIFIED., .F., .F.,
 ( 4, 3, 3, 4 ),
 ( 0.000000000000000000, 0.0001572314549002369448, 0.0003212513203110487804, 0.0004853362698026408980 ),
 .UNSPECIFIED. ) ;
#24839 = CARTESIAN_POINT ( 'NONE',  ( 10.97812500061451679, -4.541064518000419881, 2.621784821874995952 ) ) ;
#24841 = CARTESIAN_POINT ( 'NONE',  ( 22.47187500061451715, 2.746126346562645981, -4.756430356249997438 ) ) ;
#24842 = CARTESIAN_POINT ( 'NONE',  ( 10.91250000000000320, 2.886751345948129099, -4.999999999999998224 ) ) ;
#24843 = EDGE_CURVE ( 'NONE', #56056, #65447, #57913, .T. ) ;
#24844 = CARTESIAN_POINT ( 'NONE',  ( 6.787500001229032520, -4.330127018922194537, 2.499999999999995559 ) ) ;
#24845 =( BOUNDED_CURVE ( )  B_SPLINE_CURVE ( 2, ( #45411, #51313, #5526, #11430, #22504, #35042, #29144 ),
 .UNSPECIFIED., .F., .F. ) 
 B_SPLINE_CURVE_WITH_KNOTS ( ( 3, 2, 2, 3 ),
 ( 0.3750000000000000000, 0.3777777777777777679, 0.3805555555555554803, 0.3833333333333333037 ),
 .UNSPECIFIED. ) 
 CURVE ( )  GEOMETRIC_REPRESENTATION_ITEM ( )  RATIONAL_B_SPLINE_CURVE ( ( 1.000000000000000000, 0.8660254037844387076, 1.000000000000000000, 0.8660254037844387076, 1.000000000000000000, 0.8660254037844413721, 0.9999999999999973355 ) ) 
 REPRESENTATION_ITEM ( '' )  );
#24846 = CARTESIAN_POINT ( 'NONE',  ( 13.80937500061451750, -4.541064518000417216, -2.621784821875001281 ) ) ;
#24847 = CARTESIAN_POINT ( 'NONE',  ( 15.93750000122903110, 6.123233995736764310E-16, -4.999999999999998224 ) ) ;
#24848 = CARTESIAN_POINT ( 'NONE',  ( 24.93750000000000355, 5.773502691896255534, 3.535250795749688894E-16 ) ) ;
#24849 = CARTESIAN_POINT ( 'NONE',  ( -2.121784821874999949, 19.72812500061451857, -33.67503911421598417 ) ) ;
#24850 = CARTESIAN_POINT ( 'NONE',  ( -3.137519842735245283E-14, 12.57500000122903572, -26.00000000000000711 ) ) ;
#24851 = LINE ( 'NONE', #36672, #60717 ) ;
#24852 = CARTESIAN_POINT ( 'NONE',  ( 23.40000000122902790, -2.886751345948114000, 5.000000000000024869 ) ) ;
#24853 = DIRECTION ( 'NONE',  ( -1.000000000000000000, -0.000000000000000000, -0.000000000000000000 ) ) ;
#24854 = CARTESIAN_POINT ( 'NONE',  ( 3.999999999999999112, 14.48750000122903536, 30.00000000000000000 ) ) ;
#24855 = CARTESIAN_POINT ( 'NONE',  ( 15.42187500061451821, 3.027376345333611329, 5.243569643749999010 ) ) ;
#24856 = CARTESIAN_POINT ( 'NONE',  ( 28.94999999999999929, 4.330127018922192761, -2.499999999999997780 ) ) ;
#24857 = CARTESIAN_POINT ( 'NONE',  ( 13.19062500061451537, -3.027376345333614438, 5.243569643749998122 ) ) ;
#24858 = CARTESIAN_POINT ( 'NONE',  ( 7.668750001229033053, -5.773502691896255534, -1.060575238724906372E-15 ) ) ;
#24859 = CARTESIAN_POINT ( 'NONE',  ( 24.57187500061451502, -6.054752690667223547, -1.112240025338166033E-15 ) ) ;
#24860 = CARTESIAN_POINT ( 'NONE',  ( 15.68437500061451573, 5.492252693125287522, 3.363034840372157021E-16 ) ) ;
#24861 = CARTESIAN_POINT ( 'NONE',  ( 10.90312500061451928, 0.000000000000000000, 5.243569643749999010 ) ) ;
#24862 = CARTESIAN_POINT ( 'NONE',  ( 15.94687500061451502, -3.027376345333614438, 5.243569643749998122 ) ) ;
#24863 = VERTEX_POINT ( 'NONE', #27180 ) ;
#24864 = CARTESIAN_POINT ( 'NONE',  ( 27.42187500061451644, 3.027376345333613106, -5.243569643749998122 ) ) ;
#24865 = CARTESIAN_POINT ( 'NONE',  ( 28.49062500061451431, -3.027376345333614438, 5.243569643749998122 ) ) ;
#24866 = CARTESIAN_POINT ( 'NONE',  ( 17.46562500061451217, 3.027376345333613106, -5.243569643749998122 ) ) ;
#24867 = DIRECTION ( 'NONE',  ( -0.000000000000000000, -1.000000000000000000, -0.000000000000000000 ) ) ;
#24868 = CARTESIAN_POINT ( 'NONE',  ( 1.071796769724476572, 14.73259618943233562, 34.00000000000000000 ) ) ;
#24869 = CARTESIAN_POINT ( 'NONE',  ( 7.500000000000000000, 0.000000000000000000, 4.999999999999998224 ) ) ;
#24870 = CARTESIAN_POINT ( 'NONE',  ( 19.31250000122903288, 0.000000000000000000, 4.999999999999998224 ) ) ;
#24871 = CARTESIAN_POINT ( 'NONE',  ( -2.556497649636125342E-15, 18.87500000122903288, -26.00000000000000000 ) ) ;
#24872 = CARTESIAN_POINT ( 'NONE',  ( 10.80937500061451573, 2.746126346562643317, 4.756430356249998326 ) ) ;
#24873 = ORIENTED_EDGE ( 'NONE', *, *, #15601, .T. ) ;
#24874 = CARTESIAN_POINT ( 'NONE',  ( 16.91250000000000142, 2.886751345948126879, 4.999999999999999112 ) ) ;
#24875 = CARTESIAN_POINT ( 'NONE',  ( 20.10000000000000142, 0.000000000000000000, 4.999999999999998224 ) ) ;
#24876 = CARTESIAN_POINT ( 'NONE',  ( 19.47187500061451360, 3.027376345333611329, 5.243569643749999010 ) ) ;
#24877 = CARTESIAN_POINT ( 'NONE',  ( 12.66562500061451502, 3.027376345333611329, 5.243569643749999010 ) ) ;
#24878 = EDGE_CURVE ( 'NONE', #9351, #69502, #12241, .T. ) ;
#24879 = ORIENTED_EDGE ( 'NONE', *, *, #66576, .F. ) ;
#24880 = CARTESIAN_POINT ( 'NONE',  ( -5.000000000000004441, 6.123233995736764310E-16, -4.999999999999998224 ) ) ;
#24881 = CARTESIAN_POINT ( 'NONE',  ( 6.403125000614517504, 0.000000000000000000, 5.243569643749999010 ) ) ;
#24882 = CARTESIAN_POINT ( 'NONE',  ( 65.00000000000000000, -5.218601775200058412, 7.332543590861138050 ) ) ;
#24883 = CARTESIAN_POINT ( 'NONE',  ( 12.44999999999999929, 0.000000000000000000, 4.999999999999998224 ) ) ;
#24884 = CARTESIAN_POINT ( 'NONE',  ( 29.63437500061451857, 5.492252693125287522, 3.363034840372157021E-16 ) ) ;
#24885 = CARTESIAN_POINT ( 'NONE',  ( 2.121784821875001281, 15.45312500061451644, 33.67503911421598417 ) ) ;
#24886 = CARTESIAN_POINT ( 'NONE',  ( 26.20312500061451644, 0.000000000000000000, 5.243569643749999010 ) ) ;
#24887 = CARTESIAN_POINT ( 'NONE',  ( 9.299999999999998934, 0.000000000000000000, 4.999999999999998224 ) ) ;
#24888 = CARTESIAN_POINT ( 'NONE',  ( 1.878215178125000495, 18.56562499938548427, 26.74683588394047007 ) ) ;
#24889 = CARTESIAN_POINT ( 'NONE',  ( 24.90937500061451715, 0.000000000000000000, 5.243569643749999010 ) ) ;
#24890 = ORIENTED_EDGE ( 'NONE', *, *, #66396, .F. ) ;
#24891 = CARTESIAN_POINT ( 'NONE',  ( 20.91562500061451502, -6.054752690667223547, -1.112240025338166033E-15 ) ) ;
#24892 = CARTESIAN_POINT ( 'NONE',  ( 22.58437500061451431, 4.541064518000418104, 2.621784821874999949 ) ) ;
#24893 = CARTESIAN_POINT ( 'NONE',  ( -2.121784821874996840, 16.72812500061459673, -26.32496088578401583 ) ) ;
#24894 = CARTESIAN_POINT ( 'NONE',  ( 5.428125000614517859, 4.541064518000418104, 2.621784821874999949 ) ) ;
#24895 = CARTESIAN_POINT ( 'NONE',  ( 27.12187500061451573, 2.746126346562643317, 4.756430356249998326 ) ) ;
#24896 = CARTESIAN_POINT ( 'NONE',  ( 24.14062500061451289, -3.027376345333610441, -5.243569643749999898 ) ) ;
#24897 = CARTESIAN_POINT ( 'NONE',  ( 9.721875000614517148, -5.492252693125287522, -1.008910452111647106E-15 ) ) ;
#24898 = CARTESIAN_POINT ( 'NONE',  ( -3.756430356249999214, 16.87812499938548427, 27.83122392262697531 ) ) ;
#24899 = CARTESIAN_POINT ( 'NONE',  ( 16.62187500061451573, 3.027376345333613106, -5.243569643749998122 ) ) ;
#24900 = CARTESIAN_POINT ( 'NONE',  ( 25.20937500061451431, 4.541064518000418104, -2.621784821874998173 ) ) ;
#24901 = CARTESIAN_POINT ( 'NONE',  ( -2.121784821874996840, 14.08437500061451786, 33.67503911421598417 ) ) ;
#24902 = CARTESIAN_POINT ( 'NONE',  ( 6.665625000614515905, 3.027376345333613106, -5.243569643749998122 ) ) ;
#24904 =( BOUNDED_CURVE ( )  B_SPLINE_CURVE ( 2, ( #39361, #21253, #10183, #44906, #11643, #72242, #32718 ),
 .UNSPECIFIED., .F., .F. ) 
 B_SPLINE_CURVE_WITH_KNOTS ( ( 3, 2, 2, 3 ),
 ( 0.8399999999999999689, 0.8433333333333334902, 0.8466666666666667895, 0.8500000000000001998 ),
 .UNSPECIFIED. ) 
 CURVE ( )  GEOMETRIC_REPRESENTATION_ITEM ( )  RATIONAL_B_SPLINE_CURVE ( ( 1.000000000000000000, 0.8660254037844387076, 1.000000000000000000, 0.8660254037844387076, 1.000000000000000000, 0.8660254037844298258, 1.000000000000008882 ) ) 
 REPRESENTATION_ITEM ( '' )  );
#24903 = CARTESIAN_POINT ( 'NONE',  ( 28.49062500061451431, -3.027376345333614438, 5.243569643749998122 ) ) ;
#24905 = CARTESIAN_POINT ( 'NONE',  ( 3.121875000614518836, 3.027376345333613106, -5.243569643749998122 ) ) ;
#24906 = CARTESIAN_POINT ( 'NONE',  ( -4.000000000000000000, 13.62500000000000000, 30.00000000000000000 ) ) ;
#24907 = CARTESIAN_POINT ( 'NONE',  ( 5.128125000614516260, -4.541064518000419881, 2.621784821874995952 ) ) ;
#24908 = CARTESIAN_POINT ( 'NONE',  ( 10.77187500061451786, 3.027376345333613106, -5.243569643749998122 ) ) ;
#24909 =( LENGTH_UNIT ( ) NAMED_UNIT ( * ) SI_UNIT ( .MILLI., .METRE. ) );
#24910 = CARTESIAN_POINT ( 'NONE',  ( 16.01250000122903216, 4.330127018922192761, -2.499999999999997780 ) ) ;
#24911 = CARTESIAN_POINT ( 'NONE',  ( 29.65312500061451573, 4.541064518000418104, -2.621784821874998173 ) ) ;
#24912 = CARTESIAN_POINT ( 'NONE',  ( 4.565625000614516260, 3.027376345333611329, 5.243569643749999010 ) ) ;
#24913 = CARTESIAN_POINT ( 'NONE',  ( 4.000000000000000000, 12.93124999877096570, 27.69059892324149530 ) ) ;
#24914 = CARTESIAN_POINT ( 'NONE',  ( 22.21875000122903643, 2.886751345948129099, -4.999999999999998224 ) ) ;
#24915 = AXIS2_PLACEMENT_3D ( 'NONE', #28784, #11440, #5537 ) ;
#24916 = CARTESIAN_POINT ( 'NONE',  ( 15.98437500061451821, -4.541064518000419881, 2.621784821874995952 ) ) ;
#24917 = DIRECTION ( 'NONE',  ( -1.000000000000000000, -0.000000000000000000, -0.000000000000000000 ) ) ;
#24918 = ORIENTED_EDGE ( 'NONE', *, *, #34570, .T. ) ;
#24919 = CARTESIAN_POINT ( 'NONE',  ( 21.70312500061451644, 0.000000000000000000, 5.243569643749999010 ) ) ;
#24920 = CARTESIAN_POINT ( 'NONE',  ( 9.290625000614515017, -3.027376345333610441, -5.243569643749999898 ) ) ;
#24921 = CARTESIAN_POINT ( 'NONE',  ( 23.93437500061451573, 4.541064518000418104, 2.621784821874999949 ) ) ;
#24922 = CARTESIAN_POINT ( 'NONE',  ( 8.090625000614515727, 6.054752690667223547, 3.707466751127219781E-16 ) ) ;
#24923 = CARTESIAN_POINT ( 'NONE',  ( 16.38750000122903216, 6.123233995736764310E-16, -4.999999999999998224 ) ) ;
#24924 = CARTESIAN_POINT ( 'NONE',  ( 9.300000001229035362, 5.773502691896255534, 3.535250795749688894E-16 ) ) ;
#24925 = CARTESIAN_POINT ( 'NONE',  ( 23.84062500061451928, 6.054752690667223547, 3.707466751127219781E-16 ) ) ;
#24926 = CARTESIAN_POINT ( 'NONE',  ( -2.121784821874999949, 10.72812500061451679, -33.67503911421598417 ) ) ;
#24927 = CARTESIAN_POINT ( 'NONE',  ( 13.68750000122903288, 6.123233995736764310E-16, -4.999999999999998224 ) ) ;
#24928 = CARTESIAN_POINT ( 'NONE',  ( 22.90312500061451573, 4.541064518000418104, -2.621784821874998173 ) ) ;
#24929 = CARTESIAN_POINT ( 'NONE',  ( 17.35312500061451502, -4.541064518000417216, -2.621784821875001281 ) ) ;
#24930 = DIRECTION ( 'NONE',  ( 0.000000000000000000, 0.000000000000000000, 1.000000000000000000 ) ) ;
#24931 = CARTESIAN_POINT ( 'NONE',  ( 18.00000000000000355, -4.330127018922190985, -2.500000000000001332 ) ) ;
#24932 = CARTESIAN_POINT ( 'NONE',  ( 12.67500000122903536, -5.773502691896255534, -1.060575238724906372E-15 ) ) ;
#24933 = CARTESIAN_POINT ( 'NONE',  ( 11.12812500061451715, 6.421520780324663323E-16, -5.243569643749999010 ) ) ;
#24934 =( GEOMETRIC_REPRESENTATION_CONTEXT ( 3 ) GLOBAL_UNCERTAINTY_ASSIGNED_CONTEXT ( ( #42491 ) ) GLOBAL_UNIT_ASSIGNED_CONTEXT ( ( #50473, #28653, #62630 ) ) REPRESENTATION_CONTEXT ( 'NONE', 'WORKASPACE' ) );
#24935 = CARTESIAN_POINT ( 'NONE',  ( 13.04062500061451502, 6.054752690667223547, 3.707466751127219781E-16 ) ) ;
#24936 = CARTESIAN_POINT ( 'NONE',  ( 23.43750000122902932, -4.330127018922194537, 2.499999999999995559 ) ) ;
#24937 = CARTESIAN_POINT ( 'NONE',  ( 22.02187500061452141, 3.027376345333613106, -5.243569643749998122 ) ) ;
#24938 = CARTESIAN_POINT ( 'NONE',  ( 21.42187500061451644, -6.054752690667223547, -1.112240025338166033E-15 ) ) ;
#24939 = CYLINDRICAL_SURFACE ( 'NONE', #67843, 4.999999999999998224 ) ;
#24940 = CARTESIAN_POINT ( 'NONE',  ( 8.025000001229035007, 2.886751345948126879, 4.999999999999999112 ) ) ;
#24941 = CARTESIAN_POINT ( 'NONE',  ( 6.571875000614517681, -6.054752690667223547, -1.112240025338166033E-15 ) ) ;
#24942 = CARTESIAN_POINT ( 'NONE',  ( 24.68437500061451573, 6.421520780324663323E-16, -5.243569643749999010 ) ) ;
#24943 = DIRECTION ( 'NONE',  ( -0.000000000000000000, -0.000000000000000000, -1.000000000000000000 ) ) ;
#24944 = EDGE_CURVE ( 'NONE', #10639, #56113, #51287, .T. ) ;
#24945 = CARTESIAN_POINT ( 'NONE',  ( 22.22812500061451502, -4.541064518000419881, 2.621784821874995952 ) ) ;
#24946 = CARTESIAN_POINT ( 'NONE',  ( 27.27187500061451431, -6.054752690667223547, -1.112240025338166033E-15 ) ) ;
#24947 = CARTESIAN_POINT ( 'NONE',  ( -1.878215178125001827, 17.10312499938548214, 33.25316411605952283 ) ) ;
#24948 = CARTESIAN_POINT ( 'NONE',  ( 3.241876093077143306, -3.806644978545103530, 3.422667876732838010 ) ) ;
#24949 = CARTESIAN_POINT ( 'NONE',  ( 27.71250000122903145, 4.330127018922192761, -2.499999999999997780 ) ) ;
#24950 = CARTESIAN_POINT ( 'NONE',  ( 5.746875000614517504, -3.027376345333610441, -5.243569643749999898 ) ) ;
#24951 = CARTESIAN_POINT ( 'NONE',  ( 16.56562500061451715, 3.027376345333613106, -5.243569643749998122 ) ) ;
#24952 = ORIENTED_EDGE ( 'NONE', *, *, #3046, .T. ) ;
#24953 = CARTESIAN_POINT ( 'NONE',  ( 11.32500000000000107, 6.123233995736764310E-16, -4.999999999999998224 ) ) ;
#24954 = CARTESIAN_POINT ( 'NONE',  ( 25.19062500061451715, 6.054752690667223547, 3.707466751127219781E-16 ) ) ;
#24955 = CARTESIAN_POINT ( 'NONE',  ( 3.759375000614517681, 0.000000000000000000, 5.243569643749999010 ) ) ;
#24956 = CARTESIAN_POINT ( 'NONE',  ( 4.670535407306061870, 1.785677299253563444, 4.864229956990654635 ) ) ;
#24957 = CARTESIAN_POINT ( 'NONE',  ( 17.17500000000000071, 6.123233995736764310E-16, -4.999999999999998224 ) ) ;
#24958 = CARTESIAN_POINT ( 'NONE',  ( 20.01562500061451644, -6.054752690667223547, -1.112240025338166033E-15 ) ) ;
#24959 = ORIENTED_EDGE ( 'NONE', *, *, #67238, .T. ) ;
#24960 = CARTESIAN_POINT ( 'NONE',  ( 23.73749999999999716, -2.886751345948129988, 4.999999999999997335 ) ) ;
#24961 = CARTESIAN_POINT ( 'NONE',  ( 25.05937500061451573, -4.541064518000417216, -2.621784821875001281 ) ) ;
#24962 = EDGE_CURVE ( 'NONE', #64001, #34347, #30092, .T. ) ;
#24963 = VERTEX_POINT ( 'NONE', #5737 ) ;
#24964 = CARTESIAN_POINT ( 'NONE',  ( 25.91250000000000142, 2.886751345948098901, 5.000000000000047073 ) ) ;
#24965 = CARTESIAN_POINT ( 'NONE',  ( 13.49062500061451608, 6.054752690667223547, 3.707466751127219781E-16 ) ) ;
#24966 = CARTESIAN_POINT ( 'NONE',  ( 5.915625000614515905, 3.027376345333611329, 5.243569643749999010 ) ) ;
#24967 = CARTESIAN_POINT ( 'NONE',  ( 15.64687500061451608, 4.119189519843966529, -2.378215178124998275 ) ) ;
#24968 = CARTESIAN_POINT ( 'NONE',  ( 28.64062500061451289, -3.027376345333610441, -5.243569643749999898 ) ) ;
#24969 = CARTESIAN_POINT ( 'NONE',  ( 14.51250000122903394, -4.330127018922190985, -2.500000000000001332 ) ) ;
#24970 = CARTESIAN_POINT ( 'NONE',  ( 19.04999999999999716, 4.330127018922192761, -2.499999999999997780 ) ) ;
#24971 = CARTESIAN_POINT ( 'NONE',  ( 27.71250000000000568, 2.886751345948126879, 4.999999999999999112 ) ) ;
#24972 = CARTESIAN_POINT ( 'NONE',  ( 4.192336996406676342, -2.724758798235080715, 4.480034832487019614 ) ) ;
#24973 = CARTESIAN_POINT ( 'NONE',  ( 10.32187500061451679, 3.027376345333613106, -5.243569643749998122 ) ) ;
#24974 = CARTESIAN_POINT ( 'NONE',  ( 18.72187500061451360, -6.054752690667223547, -1.112240025338166033E-15 ) ) ;
#24975 = CARTESIAN_POINT ( 'NONE',  ( 2.000000000000001332, 11.26250000122903394, 33.46410161513774995 ) ) ;
#24976 = ORIENTED_EDGE ( 'NONE', *, *, #3997, .F. ) ;
#24977 = CARTESIAN_POINT ( 'NONE',  ( 29.80312500061451431, 0.000000000000000000, 5.243569643749999010 ) ) ;
#24978 = CARTESIAN_POINT ( 'NONE',  ( 29.48437500061451644, -4.541064518000419881, 2.621784821874995952 ) ) ;
#24979 = CARTESIAN_POINT ( 'NONE',  ( 5.071875000614519458, 3.027376345333611329, 5.243569643749999010 ) ) ;
#24980 = CARTESIAN_POINT ( 'NONE',  ( 15.67500000000000071, -4.330127018922194537, 2.499999999999995559 ) ) ;
#24981 = CARTESIAN_POINT ( 'NONE',  ( 14.05312500061451431, 0.000000000000000000, 5.243569643749999010 ) ) ;
#24982 = CARTESIAN_POINT ( 'NONE',  ( 2.000000000000000444, 18.42500000000000071, 26.53589838486224650 ) ) ;
#24983 = CARTESIAN_POINT ( 'NONE',  ( 4.964961267422091318, 0.6791209066532012395, -5.083749661835663680 ) ) ;
#24984 = CARTESIAN_POINT ( 'NONE',  ( 8.306250001229031454, 4.330127018922192761, -2.499999999999997780 ) ) ;
#24985 = CARTESIAN_POINT ( 'NONE',  ( 17.96250000122903501, 0.000000000000000000, 4.999999999999998224 ) ) ;
#24986 = CARTESIAN_POINT ( 'NONE',  ( 0.4082266053725523425, 9.993705886960393414, 24.01047330894736831 ) ) ;
#24987 = CARTESIAN_POINT ( 'NONE',  ( 18.75937500061451857, -4.119189519843965641, -2.378215178125001383 ) ) ;
#24988 = CARTESIAN_POINT ( 'NONE',  ( 7.978125000614517681, 6.421520780324663323E-16, -5.243569643749999010 ) ) ;
#24989 = CARTESIAN_POINT ( 'NONE',  ( 23.33437500061451786, 6.421520780324663323E-16, -5.243569643749999010 ) ) ;
#24990 = EDGE_CURVE ( 'NONE', #66446, #1783, #5011, .T. ) ;
#24991 = CARTESIAN_POINT ( 'NONE',  ( 27.11250000122903359, -4.330127018922190985, -2.500000000000001332 ) ) ;
#24992 = CARTESIAN_POINT ( 'NONE',  ( 24.30937500061451573, 4.541064518000418104, -2.621784821874998173 ) ) ;
#24993 = CARTESIAN_POINT ( 'NONE',  ( 6.187500000000002665, -2.886751345948129988, 4.999999999999997335 ) ) ;
#24994 = CARTESIAN_POINT ( 'NONE',  ( -2.000000000000000000, 9.687500001229034652, 26.53589838486224650 ) ) ;
#24995 = CARTESIAN_POINT ( 'NONE',  ( 13.52812500061451750, 4.541064518000418104, 2.621784821874999949 ) ) ;
#24996 = CARTESIAN_POINT ( 'NONE',  ( 5.662500001229035185, 4.330127018922192761, -2.499999999999997780 ) ) ;
#24997 = VECTOR ( 'NONE', #10489, 1000.000000000000000 ) ;
#24998 = CARTESIAN_POINT ( 'NONE',  ( 10.20937500061451786, -4.541064518000417216, -2.621784821875001281 ) ) ;
#24999 = CARTESIAN_POINT ( 'NONE',  ( 1.071796769724497445, 15.02990381179670010, 26.00000000000000355 ) ) ;
#25000 = VERTEX_POINT ( 'NONE', #61153 ) ;
#25001 = CARTESIAN_POINT ( 'NONE',  ( 12.47812500061451502, 6.421520780324663323E-16, -5.243569643749999010 ) ) ;
#25002 = CARTESIAN_POINT ( 'NONE',  ( 14.02499999999999858, 6.123233995736764310E-16, -4.999999999999998224 ) ) ;
#25003 = CARTESIAN_POINT ( 'NONE',  ( 24.22500000122903430, 2.886751345948126879, 4.999999999999999112 ) ) ;
#25004 = CARTESIAN_POINT ( 'NONE',  ( 9.534375000614517148, 4.541064518000418104, 2.621784821874999949 ) ) ;
#25005 = CARTESIAN_POINT ( 'NONE',  ( 14.91562500061451679, 3.027376345333611329, 5.243569643749999010 ) ) ;
#25006 = CARTESIAN_POINT ( 'NONE',  ( 27.35625000122903216, 0.000000000000000000, 4.999999999999998224 ) ) ;
#25007 = CARTESIAN_POINT ( 'NONE',  ( 22.80937500061451573, -4.541064518000417216, -2.621784821875001281 ) ) ;
#25008 = CARTESIAN_POINT ( 'NONE',  ( 26.45625000122903003, 0.000000000000000000, 4.999999999999998224 ) ) ;
#25009 = FACE_OUTER_BOUND ( 'NONE', #64177, .T. ) ;
#25010 = CARTESIAN_POINT ( 'NONE',  ( 20.62500000122903643, 2.886751345948161074, 4.999999999999941380 ) ) ;
#25011 = CARTESIAN_POINT ( 'NONE',  ( -4.243569643749999898, 14.00937500061451857, -30.00000000000000000 ) ) ;
#25012 = CARTESIAN_POINT ( 'NONE',  ( 16.43437500061451573, -4.541064518000419881, 2.621784821874995952 ) ) ;
#25013 = CARTESIAN_POINT ( 'NONE',  ( 17.32500000122903216, 2.886751345948129099, -4.999999999999998224 ) ) ;
#25014 = CARTESIAN_POINT ( 'NONE',  ( 11.89687500061451608, -3.027376345333614438, 5.243569643749998122 ) ) ;
#25015 = CARTESIAN_POINT ( 'NONE',  ( 4.243569643749999898, 18.22812500061451502, -30.00000000000000000 ) ) ;
#25016 = CARTESIAN_POINT ( 'NONE',  ( 21.15000000122903145, -2.886751345948129988, 4.999999999999997335 ) ) ;
#25017 = CARTESIAN_POINT ( 'NONE',  ( 12.25312500061451537, 0.000000000000000000, 5.243569643749999010 ) ) ;
#25018 = ORIENTED_EDGE ( 'NONE', *, *, #69109, .F. ) ;
#25019 = ORIENTED_EDGE ( 'NONE', *, *, #15748, .F. ) ;
#25020 = CARTESIAN_POINT ( 'NONE',  ( 15.78749999999999964, -2.886751345948125991, -5.000000000000000000 ) ) ;
#25021 = CARTESIAN_POINT ( 'NONE',  ( 19.08750000122903145, 6.123233995736764310E-16, -4.999999999999998224 ) ) ;
#25022 = CARTESIAN_POINT ( 'NONE',  ( 13.05937500061451750, 4.541064518000418104, -2.621784821874998173 ) ) ;
#25023 = CARTESIAN_POINT ( 'NONE',  ( 3.182906284435134125, 3.860443623060027640, 27.56482146223813601 ) ) ;
#25024 = CARTESIAN_POINT ( 'NONE',  ( 12.37500000122903465, 2.886751345948129099, -4.999999999999998224 ) ) ;
#25025 = CARTESIAN_POINT ( 'NONE',  ( 20.36250000122903359, -4.330127018922190985, -2.500000000000001332 ) ) ;
#25026 = CARTESIAN_POINT ( 'NONE',  ( 16.45312500061451289, -4.541064518000417216, -2.621784821875001281 ) ) ;
#25027 = CARTESIAN_POINT ( 'NONE',  ( 20.84062500061451573, -3.027376345333614438, 5.243569643749998122 ) ) ;
#25028 = CARTESIAN_POINT ( 'NONE',  ( 28.61250000122903359, 4.330127018922192761, -2.499999999999997780 ) ) ;
#25029 = CARTESIAN_POINT ( 'NONE',  ( 28.35000000000000142, -4.330127018922190985, -2.500000000000001332 ) ) ;
#25030 = DIRECTION ( 'NONE',  ( -0.000000000000000000, -1.000000000000000000, -0.000000000000000000 ) ) ;
#25031 = CARTESIAN_POINT ( 'NONE',  ( 29.81250000000000000, 2.886751345948129099, -4.999999999999998224 ) ) ;
#25032 = CARTESIAN_POINT ( 'NONE',  ( 28.50937500061451502, 0.000000000000000000, 5.243569643749999010 ) ) ;
#25033 = CARTESIAN_POINT ( 'NONE',  ( -3.999999999999999556, 9.725000001229034297, -32.30940107675850470 ) ) ;
#25034 = CARTESIAN_POINT ( 'NONE',  ( 9.001249775931846008E-16, 16.82187500061451857, -25.09994784771203058 ) ) ;
#25035 = CARTESIAN_POINT ( 'NONE',  ( 2.850000001229036073, -2.886751345948125991, -5.000000000000000000 ) ) ;
#25036 = CARTESIAN_POINT ( 'NONE',  ( 6.337499999999998579, -2.886751345948125991, -5.000000000000000000 ) ) ;
#25037 = CARTESIAN_POINT ( 'NONE',  ( 2.850000001229036073, -2.886751345948125991, -5.000000000000000000 ) ) ;
#25038 = CARTESIAN_POINT ( 'NONE',  ( 10.65937500061451715, -4.541064518000417216, -2.621784821875001281 ) ) ;
#25039 = CARTESIAN_POINT ( 'NONE',  ( 29.12812500061451715, 6.421520780324663323E-16, -5.243569643749999010 ) ) ;
#25040 = DIRECTION ( 'NONE',  ( -1.000000000000000000, -0.000000000000000000, -0.000000000000000000 ) ) ;
#25041 = CARTESIAN_POINT ( 'NONE',  ( 30.00000000000000000, 6.123233995736764310E-16, -4.999999999999998224 ) ) ;
#25042 = CARTESIAN_POINT ( 'NONE',  ( 3.999999999999998668, 17.67500000122903359, -32.30940107675850470 ) ) ;
#25043 = EDGE_CURVE ( 'NONE', #5464, #45340, #17169, .T. ) ;
#25044 = CARTESIAN_POINT ( 'NONE',  ( 8.596875000614518925, 6.054752690667223547, 3.707466751127219781E-16 ) ) ;
#25045 = CARTESIAN_POINT ( 'NONE',  ( 10.99687500061451750, -3.027376345333614438, 5.243569643749998122 ) ) ;
#25046 = CARTESIAN_POINT ( 'NONE',  ( 5.175000000000002487, 4.330127018922191873, 2.499999999999999556 ) ) ;
#25047 = CARTESIAN_POINT ( 'NONE',  ( -2.121784821874999949, 15.22812500061459495, 26.32496088578401938 ) ) ;
#25048 = DIRECTION ( 'NONE',  ( -1.000000000000000000, -0.000000000000000000, -0.000000000000000000 ) ) ;
#25049 = CARTESIAN_POINT ( 'NONE',  ( 7.575000000000001954, -4.330127018922194537, 2.499999999999995559 ) ) ;
#25050 = CARTESIAN_POINT ( 'NONE',  ( 14.59687500061451537, -4.119189519843965641, -2.378215178125001383 ) ) ;
#25051 = CARTESIAN_POINT ( 'NONE',  ( 20.57812500061451644, 6.421520780324663323E-16, -5.243569643749999010 ) ) ;
#25052 = CARTESIAN_POINT ( 'NONE',  ( 12.70312500061451821, 0.000000000000000000, 5.243569643749999010 ) ) ;
#25053 = CARTESIAN_POINT ( 'NONE',  ( 24.75937500061451502, 2.746126346562643317, 4.756430356249998326 ) ) ;
#25054 = CARTESIAN_POINT ( 'NONE',  ( 9.384375000614518569, 6.421520780324663323E-16, -5.243569643749999010 ) ) ;
#25055 = CARTESIAN_POINT ( 'NONE',  ( 25.31250000000000000, 2.886751345948129099, -4.999999999999998224 ) ) ;
#25056 = CARTESIAN_POINT ( 'NONE',  ( 21.82500000122903572, 2.886751345948129099, -4.999999999999998224 ) ) ;
#25057 = LINE ( 'NONE', #70866, #34317 ) ;
#25058 = CARTESIAN_POINT ( 'NONE',  ( 8.709375000614517859, 0.000000000000000000, 5.243569643749999010 ) ) ;
#25059 = CARTESIAN_POINT ( 'NONE',  ( 27.12187500061451573, 3.027376345333611329, 5.243569643749999010 ) ) ;
#25060 = LINE ( 'NONE', #65318, #37125 ) ;
#25061 = CARTESIAN_POINT ( 'NONE',  ( 25.55625000122903501, 0.000000000000000000, 4.999999999999998224 ) ) ;
#25062 = CARTESIAN_POINT ( 'NONE',  ( 19.13437500061451857, -4.541064518000419881, 2.621784821874995952 ) ) ;
#25063 = CARTESIAN_POINT ( 'NONE',  ( 12.57187500061451857, 3.027376345333613106, -5.243569643749998122 ) ) ;
#25064 = CARTESIAN_POINT ( 'NONE',  ( 3.756430356250000102, 19.95312499938548356, 30.00000000000000000 ) ) ;
#25065 = CARTESIAN_POINT ( 'NONE',  ( 23.73749999999999716, -2.886751345948129988, 4.999999999999997335 ) ) ;
#25066 = CARTESIAN_POINT ( 'NONE',  ( 2.000000000000000444, 15.27500000000000036, 26.53589838486224650 ) ) ;
#25067 = CARTESIAN_POINT ( 'NONE',  ( -4.243569643749999898, 13.07187500061452035, -32.45002607614398471 ) ) ;
#25068 = CARTESIAN_POINT ( 'NONE',  ( 23.97187500061451360, 2.746126346562643317, 4.756430356249998326 ) ) ;
#25069 = CARTESIAN_POINT ( 'NONE',  ( 15.77812500061451573, 4.541064518000418104, 2.621784821874999949 ) ) ;
#25070 = CARTESIAN_POINT ( 'NONE',  ( 5.062500000000000888, 2.886751345948129099, -4.999999999999998224 ) ) ;
#25071 = FACE_OUTER_BOUND ( 'NONE', #10177, .T. ) ;
#25072 = CARTESIAN_POINT ( 'NONE',  ( 13.53749999999999964, -2.886751345948125991, -5.000000000000000000 ) ) ;
#25073 = CARTESIAN_POINT ( 'NONE',  ( -4.243569643749999898, 10.76562500061451644, 27.54997392385601529 ) ) ;
#25074 = CARTESIAN_POINT ( 'NONE',  ( 13.46250000122903323, 0.000000000000000000, 4.999999999999998224 ) ) ;
#25075 = CARTESIAN_POINT ( 'NONE',  ( 24.12187500061451217, -6.054752690667223547, -1.112240025338166033E-15 ) ) ;
#25076 = CARTESIAN_POINT ( 'NONE',  ( 17.82187500061451502, -6.054752690667223547, -1.112240025338166033E-15 ) ) ;
#25077 = CARTESIAN_POINT ( 'NONE',  ( 25.33125000122903003, 6.123233995736764310E-16, -4.999999999999998224 ) ) ;
#25078 = ORIENTED_EDGE ( 'NONE', *, *, #38684, .T. ) ;
#25079 = CARTESIAN_POINT ( 'NONE',  ( 19.71562500061451928, 3.027376345333613106, -5.243569643749998122 ) ) ;
#25080 = CARTESIAN_POINT ( 'NONE',  ( 4.528125000614516615, 4.541064518000418104, 2.621784821874999949 ) ) ;
#25081 = CARTESIAN_POINT ( 'NONE',  ( 17.44687500061451857, -3.027376345333610441, -5.243569643749999898 ) ) ;
#25082 = CARTESIAN_POINT ( 'NONE',  ( 28.73437500061451644, 6.421520780324663323E-16, -5.243569643749999010 ) ) ;
#25083 = CARTESIAN_POINT ( 'NONE',  ( 4.640625000614518214, -3.027376345333614438, 5.243569643749998122 ) ) ;
#25084 = CARTESIAN_POINT ( 'NONE',  ( 22.07812500061451644, 4.541064518000418104, 2.621784821874999949 ) ) ;
#25085 = CARTESIAN_POINT ( 'NONE',  ( 4.243569643749999898, 14.62812500061451715, 30.00000000000000000 ) ) ;
#25086 = CARTESIAN_POINT ( 'NONE',  ( 15.67500000122903181, 2.886751345948126879, 4.999999999999999112 ) ) ;
#25087 = CARTESIAN_POINT ( 'NONE',  ( 13.43437500061451750, 5.824947211148865298E-16, -4.756430356249998326 ) ) ;
#25088 = CARTESIAN_POINT ( 'NONE',  ( 7.190625000614518036, 6.054752690667223547, 3.707466751127219781E-16 ) ) ;
#25089 = CARTESIAN_POINT ( 'NONE',  ( 13.57500000000000107, 6.123233995736764310E-16, -4.999999999999998224 ) ) ;
#25090 = CARTESIAN_POINT ( 'NONE',  ( 28.97812500061451502, -4.541064518000419881, 2.621784821874995952 ) ) ;
#25091 = CARTESIAN_POINT ( 'NONE',  ( 23.97187500061451360, 3.027376345333611329, 5.243569643749999010 ) ) ;
#25092 = CARTESIAN_POINT ( 'NONE',  ( 15.51562500061451644, -6.054752690667223547, -1.112240025338166033E-15 ) ) ;
#25093 = CARTESIAN_POINT ( 'NONE',  ( 24.63750000122903216, 4.330127018922191873, 2.499999999999999556 ) ) ;
#25094 = CARTESIAN_POINT ( 'NONE',  ( 24.44062500061451715, -3.027376345333614438, 5.243569643749998122 ) ) ;
#25095 = CARTESIAN_POINT ( 'NONE',  ( 19.35937500061451644, 4.541064518000418104, -2.621784821874998173 ) ) ;
#25096 = CARTESIAN_POINT ( 'NONE',  ( 14.09062500061451750, -3.027376345333614438, 5.243569643749998122 ) ) ;
#25097 = CARTESIAN_POINT ( 'NONE',  ( -4.243569643749997233, 18.09687500061452070, 32.45002607614398471 ) ) ;
#25098 = CARTESIAN_POINT ( 'NONE',  ( 20.84062500061451573, -3.027376345333614438, 5.243569643749998122 ) ) ;
#25099 = CARTESIAN_POINT ( 'NONE',  ( 29.42812500061451431, -4.541064518000419881, 2.621784821874995952 ) ) ;
#25100 = ORIENTED_EDGE ( 'NONE', *, *, #63479, .T. ) ;
#25101 = CARTESIAN_POINT ( 'NONE',  ( 25.94999999999999929, 0.000000000000000000, 4.999999999999998224 ) ) ;
#25102 = CARTESIAN_POINT ( 'NONE',  ( -4.243569643749999898, 19.40937500061451715, -30.00000000000000000 ) ) ;
#25103 = CARTESIAN_POINT ( 'NONE',  ( 2.655984681222220721E-16, 19.61562499938548143, 25.66244784525396483 ) ) ;
#25104 = CARTESIAN_POINT ( 'NONE',  ( 27.32812500061451644, 6.421520780324663323E-16, -5.243569643749999010 ) ) ;
#25105 = CARTESIAN_POINT ( 'NONE',  ( 8.840625000614515727, -3.027376345333610441, -5.243569643749999898 ) ) ;
#25106 = CARTESIAN_POINT ( 'NONE',  ( 20.17500000122903359, 2.886751345948126879, 4.999999999999999112 ) ) ;
#25107 = CARTESIAN_POINT ( 'NONE',  ( 25.49062500061451786, -3.027376345333610441, -5.243569643749999898 ) ) ;
#25108 = CARTESIAN_POINT ( 'NONE',  ( 25.94999999999999929, 0.000000000000000000, 4.999999999999998224 ) ) ;
#25109 = CARTESIAN_POINT ( 'NONE',  ( 3.999999999999999112, 16.28750000122903430, -30.00000000000000000 ) ) ;
#25110 = CARTESIAN_POINT ( 'NONE',  ( 27.32812500061451644, 6.421520780324663323E-16, -5.243569643749999010 ) ) ;
#25111 = CARTESIAN_POINT ( 'NONE',  ( 7.865625000614516971, -6.054752690667223547, -1.112240025338166033E-15 ) ) ;
#25112 = ORIENTED_EDGE ( 'NONE', *, *, #29363, .T. ) ;
#25113 = EDGE_CURVE ( 'NONE', #403, #10458, #32406, .T. ) ;
#25114 = CARTESIAN_POINT ( 'NONE',  ( 26.31562500061451715, -6.054752690667223547, -1.112240025338166033E-15 ) ) ;
#25115 = CARTESIAN_POINT ( 'NONE',  ( 5.353125000614515905, 4.541064518000418104, -2.621784821874998173 ) ) ;
#25116 = CARTESIAN_POINT ( 'NONE',  ( 14.33437500061451786, 5.824947211148865298E-16, -4.756430356249998326 ) ) ;
#25117 = DIRECTION ( 'NONE',  ( 0.000000000000000000, 0.000000000000000000, 1.000000000000000000 ) ) ;
#25118 = CARTESIAN_POINT ( 'NONE',  ( 13.76250000000000107, 2.886751345948126879, 4.999999999999999112 ) ) ;
#25119 =( BOUNDED_CURVE ( )  B_SPLINE_CURVE ( 2, ( #11912, #29895, #41708, #475, #64232, #68074, #40000 ),
 .UNSPECIFIED., .F., .F. ) 
 B_SPLINE_CURVE_WITH_KNOTS ( ( 3, 2, 2, 3 ),
 ( 0.4900000000000001021, 0.4933333333333334569, 0.4966666666666667562, 0.5000000000000001110 ),
 .UNSPECIFIED. ) 
 CURVE ( )  GEOMETRIC_REPRESENTATION_ITEM ( )  RATIONAL_B_SPLINE_CURVE ( ( 0.9999999999999955591, 0.8660254037844431485, 1.000000000000000000, 0.8660254037844387076, 1.000000000000000000, 0.8660254037844342667, 1.000000000000004441 ) ) 
 REPRESENTATION_ITEM ( '' )  );
#25120 = CARTESIAN_POINT ( 'NONE',  ( 14.25937500061451679, -4.541064518000417216, -2.621784821875001281 ) ) ;
#25121 = CARTESIAN_POINT ( 'NONE',  ( 9.262500001229033941, 4.330127018922192761, -2.499999999999997780 ) ) ;
#25122 = CARTESIAN_POINT ( 'NONE',  ( 17.07187500061451502, 3.027376345333613106, -5.243569643749998122 ) ) ;
#25123 = CARTESIAN_POINT ( 'NONE',  ( 14.58750000000000036, 5.773502691896255534, 3.535250795749688894E-16 ) ) ;
#25124 = CARTESIAN_POINT ( 'NONE',  ( 7.584375000614516082, 6.421520780324663323E-16, -5.243569643749999010 ) ) ;
#25125 = CARTESIAN_POINT ( 'NONE',  ( -2.121784821874999949, 11.62812500061451715, -33.67503911421598417 ) ) ;
#25126 = CARTESIAN_POINT ( 'NONE',  ( 20.10000000000000142, 0.000000000000000000, 4.999999999999998224 ) ) ;
#25127 = EDGE_CURVE ( 'NONE', #9094, #66820, #24904, .T. ) ;
#25128 = CARTESIAN_POINT ( 'NONE',  ( 22.09687500061451360, 0.000000000000000000, 4.756430356249998326 ) ) ;
#25129 = CARTESIAN_POINT ( 'NONE',  ( 15.63749999999999929, -2.886751345948074920, 5.000000000000092371 ) ) ;
#25130 = CARTESIAN_POINT ( 'NONE',  ( 23.91562500061451502, 3.027376345333611329, 5.243569643749999010 ) ) ;
#25131 = CARTESIAN_POINT ( 'NONE',  ( 2.121784821874999061, 10.25937500061451857, 26.32496088578401583 ) ) ;
#25132 = CARTESIAN_POINT ( 'NONE',  ( 34.99999999999999289, 2.500000000000000444, 5.500000000000000000 ) ) ;
#25133 = CARTESIAN_POINT ( 'NONE',  ( 26.78437500061451360, -4.541064518000419881, 2.621784821874995952 ) ) ;
#25134 = CARTESIAN_POINT ( 'NONE',  ( 29.55937500061451573, -4.541064518000417216, -2.621784821875001281 ) ) ;
#25135 = CARTESIAN_POINT ( 'NONE',  ( 5.015625000614518214, 3.027376345333611329, 5.243569643749999010 ) ) ;
#25136 = CARTESIAN_POINT ( 'NONE',  ( 22.88437500061451502, 5.492252693125287522, 3.363034840372157021E-16 ) ) ;
#25137 = CARTESIAN_POINT ( 'NONE',  ( 17.82187500061451502, -6.054752690667223547, -1.112240025338166033E-15 ) ) ;
#25138 = CARTESIAN_POINT ( 'NONE',  ( 7.921875000614517326, 5.824947211148865298E-16, -4.756430356249998326 ) ) ;
#25139 = CARTESIAN_POINT ( 'NONE',  ( 3.365625000614516082, -6.054752690667223547, -1.112240025338166033E-15 ) ) ;
#25140 = CARTESIAN_POINT ( 'NONE',  ( 7.171875000614517326, 3.027376345333613106, -5.243569643749998122 ) ) ;
#25141 = CARTESIAN_POINT ( 'NONE',  ( 19.99687500061451573, -3.027376345333614438, 5.243569643749998122 ) ) ;
#25142 = CARTESIAN_POINT ( 'NONE',  ( -2.642701734113356959, 25.30472597034935944, 33.01399490227544220 ) ) ;
#25143 = CARTESIAN_POINT ( 'NONE',  ( 26.28749999999999432, 5.773502691896255534, 3.535250795749688894E-16 ) ) ;
#25145 = EDGE_CURVE ( 'NONE', #755, #35328, #62664, .T. ) ;
#25144 = CARTESIAN_POINT ( 'NONE',  ( 26.78437500061451360, -4.541064518000419881, 2.621784821874995952 ) ) ;
#25146 = CARTESIAN_POINT ( 'NONE',  ( 2.000000000000000444, 15.72499999999999964, 26.53589838486224650 ) ) ;
#25147 = CARTESIAN_POINT ( 'NONE',  ( 29.88749999999999929, 5.773502691896255534, 3.535250795749688894E-16 ) ) ;
#25148 = VERTEX_POINT ( 'NONE', #33077 ) ;
#25149 = CARTESIAN_POINT ( 'NONE',  ( 8.400000000000000355, 0.000000000000000000, 4.999999999999998224 ) ) ;
#25150 = CARTESIAN_POINT ( 'NONE',  ( 9.946875000614516793, 0.000000000000000000, 4.756430356249998326 ) ) ;
#25151 = CARTESIAN_POINT ( 'NONE',  ( 23.12812500061451360, -4.541064518000419881, 2.621784821874995952 ) ) ;
#25152 = CARTESIAN_POINT ( 'NONE',  ( 11.32500000000000107, 6.123233995736764310E-16, -4.999999999999998224 ) ) ;
#25153 = CARTESIAN_POINT ( 'NONE',  ( 8.287500001229034297, 6.123233995736764310E-16, -4.999999999999998224 ) ) ;
#25154 = CARTESIAN_POINT ( 'NONE',  ( 6.590625000614518392, -3.027376345333610441, -5.243569643749999898 ) ) ;
#25155 = CARTESIAN_POINT ( 'NONE',  ( 22.87500000000000000, -4.330127018922194537, 2.499999999999995559 ) ) ;
#25156 = CARTESIAN_POINT ( 'NONE',  ( 18.55312500061451431, 0.000000000000000000, 5.243569643749999010 ) ) ;
#25157 = CARTESIAN_POINT ( 'NONE',  ( 25.57500000122903216, 2.886751345948126879, 4.999999999999999112 ) ) ;
#25158 = CARTESIAN_POINT ( 'NONE',  ( 3.756430356249998770, 18.90312499938548285, 32.16877607737301759 ) ) ;
#25159 = CARTESIAN_POINT ( 'NONE',  ( 4.912499999999999645, -5.773502691896255534, -1.060575238724906372E-15 ) ) ;
#25160 = ORIENTED_EDGE ( 'NONE', *, *, #23644, .T. ) ;
#25161 = CARTESIAN_POINT ( 'NONE',  ( 18.89062500061451644, 6.054752690667223547, 3.707466751127219781E-16 ) ) ;
#25162 = CARTESIAN_POINT ( 'NONE',  ( 27.10312500061451502, 0.000000000000000000, 5.243569643749999010 ) ) ;
#25163 = CARTESIAN_POINT ( 'NONE',  ( 27.53437500061451360, 4.541064518000418104, 2.621784821874999949 ) ) ;
#25164 = CARTESIAN_POINT ( 'NONE',  ( 8.437500000000000000, -2.886751345948129988, 4.999999999999997335 ) ) ;
#25165 = CARTESIAN_POINT ( 'NONE',  ( 14.69062500061451537, -3.027376345333610441, -5.243569643749999898 ) ) ;
#25166 = CARTESIAN_POINT ( 'NONE',  ( 29.61562500061451431, 3.027376345333613106, -5.243569643749998122 ) ) ;
#25167 = CARTESIAN_POINT ( 'NONE',  ( 8.540625000614518569, 6.054752690667223547, 3.707466751127219781E-16 ) ) ;
#25168 = DIRECTION ( 'NONE',  ( 0.000000000000000000, 0.000000000000000000, -1.000000000000000000 ) ) ;
#25169 = CARTESIAN_POINT ( 'NONE',  ( 4.243569643749999898, 13.33437500061451786, 30.00000000000000000 ) ) ;
#25170 = CARTESIAN_POINT ( 'NONE',  ( 25.27500000122903145, -5.773502691896255534, -1.060575238724906372E-15 ) ) ;
#25171 = CARTESIAN_POINT ( 'NONE',  ( 19.84687500061451360, 5.492252693125287522, 3.363034840372157021E-16 ) ) ;
#25172 = CARTESIAN_POINT ( 'NONE',  ( 14.12812500061451715, -4.541064518000419881, 2.621784821874995952 ) ) ;
#25173 = CARTESIAN_POINT ( 'NONE',  ( 28.63125000122903074, 4.330127018922191873, 2.499999999999999556 ) ) ;
#25174 = CARTESIAN_POINT ( 'NONE',  ( 9.271875000614516082, -6.054752690667223547, -1.112240025338166033E-15 ) ) ;
#25175 = CARTESIAN_POINT ( 'NONE',  ( 9.384375000614518569, 6.421520780324663323E-16, -5.243569643749999010 ) ) ;
#25176 = CARTESIAN_POINT ( 'NONE',  ( 18.42187500061451644, 3.027376345333613106, -5.243569643749998122 ) ) ;
#25177 = EDGE_LOOP ( 'NONE', ( #25861, #1118, #34844, #60542 ) ) ;
#25178 = CARTESIAN_POINT ( 'NONE',  ( 20.87812500061451715, -4.541064518000419881, 2.621784821874995952 ) ) ;
#25179 = CARTESIAN_POINT ( 'NONE',  ( 16.35937500061451644, 0.000000000000000000, 5.243569643749999010 ) ) ;
#25180 = CARTESIAN_POINT ( 'NONE',  ( 22.79062500061451502, -3.027376345333610441, -5.243569643749999898 ) ) ;
#25181 = CARTESIAN_POINT ( 'NONE',  ( 2.000000000000001332, 13.85000000000000142, 33.46410161513774995 ) ) ;
#25182 = CARTESIAN_POINT ( 'NONE',  ( 27.29062500061451502, -3.027376345333610441, -5.243569643749999898 ) ) ;
#25183 = CARTESIAN_POINT ( 'NONE',  ( 7.800000001229035362, -2.886751345948125991, -5.000000000000000000 ) ) ;
#25184 = ORIENTED_EDGE ( 'NONE', *, *, #5473, .T. ) ;
#25185 = CARTESIAN_POINT ( 'NONE',  ( 3.675000001229035362, -5.773502691896255534, -1.060575238724906372E-15 ) ) ;
#25186 = CARTESIAN_POINT ( 'NONE',  ( 3.999999999999998668, 18.01249999999999929, -32.30940107675850470 ) ) ;
#25187 = CARTESIAN_POINT ( 'NONE',  ( 23.70000000122903216, 5.773502691896255534, 3.535250795749688894E-16 ) ) ;
#25188 = CARTESIAN_POINT ( 'NONE',  ( -4.000000000000000000, 19.86874999877096570, 30.00000000000000000 ) ) ;
#25189 = CARTESIAN_POINT ( 'NONE',  ( 8.109375000614518214, 4.541064518000418104, -2.621784821874998173 ) ) ;
#25190 = CARTESIAN_POINT ( 'NONE',  ( 4.307019252286369060, 2.539784937741765614, -4.371005586624799655 ) ) ;
#25191 = CARTESIAN_POINT ( 'NONE',  ( 15.55312500061451608, -4.541064518000417216, -2.621784821875001281 ) ) ;
#25192 = CARTESIAN_POINT ( 'NONE',  ( 8.821875000614518569, -6.054752690667223547, -1.112240025338166033E-15 ) ) ;
#25193 = CARTESIAN_POINT ( 'NONE',  ( 26.92500000122903359, 2.886751345948126879, 4.999999999999999112 ) ) ;
#25194 = CARTESIAN_POINT ( 'NONE',  ( 18.45937500061451431, 4.541064518000418104, -2.621784821874998173 ) ) ;
#25195 = CARTESIAN_POINT ( 'NONE',  ( 4.396875000614516971, -3.027376345333610441, -5.243569643749999898 ) ) ;
#25196 = CARTESIAN_POINT ( 'NONE',  ( 45.00000000000000000, 0.000000000000000000, 0.000000000000000000 ) ) ;
#25197 = CARTESIAN_POINT ( 'NONE',  ( 5.915625000614515905, 3.027376345333611329, 5.243569643749999010 ) ) ;
#25198 = CARTESIAN_POINT ( 'NONE',  ( 18.74062500061451431, -3.027376345333610441, -5.243569643749999898 ) ) ;
#25199 = ORIENTED_EDGE ( 'NONE', *, *, #11122, .F. ) ;
#25200 = CARTESIAN_POINT ( 'NONE',  ( 11.46562500061451573, -6.054752690667223547, -1.112240025338166033E-15 ) ) ;
#25201 = CARTESIAN_POINT ( 'NONE',  ( 6.225000001229036073, 2.886751345948126879, 4.999999999999999112 ) ) ;
#25202 = CARTESIAN_POINT ( 'NONE',  ( 10.45312500061451644, 0.000000000000000000, 5.243569643749999010 ) ) ;
#25203 = CARTESIAN_POINT ( 'NONE',  ( 21.27187500061451786, 2.746126346562643317, 4.756430356249998326 ) ) ;
#25204 = CARTESIAN_POINT ( 'NONE',  ( 11.02500000000000036, 4.330127018922191873, 2.499999999999999556 ) ) ;
#25205 = CARTESIAN_POINT ( 'NONE',  ( 5.812500001229035540, 0.000000000000000000, 4.999999999999998224 ) ) ;
#25206 = CARTESIAN_POINT ( 'NONE',  ( 19.76250000000000639, -5.773502691896255534, -1.060575238724906372E-15 ) ) ;
#25207 = EDGE_CURVE ( 'NONE', #10170, #67346, #35687, .T. ) ;
#25208 = CARTESIAN_POINT ( 'NONE',  ( 15.60937500061451644, -4.541064518000417216, -2.621784821875001281 ) ) ;
#25209 = CARTESIAN_POINT ( 'NONE',  ( 14.88750000122903394, -4.330127018922194537, 2.499999999999995559 ) ) ;
#25210 = CARTESIAN_POINT ( 'NONE',  ( 22.87500000000000000, -4.330127018922194537, 2.499999999999995559 ) ) ;
#25211 = CARTESIAN_POINT ( 'NONE',  ( 2.226602359779148887, 9.807522476441999260, -34.70164361699148259 ) ) ;
#25212 = CARTESIAN_POINT ( 'NONE',  ( 34.99999999999999289, -2.499999999999999556, 3.499999999999999556 ) ) ;
#25213 = CARTESIAN_POINT ( 'NONE',  ( 3.999999999999998668, 14.97500000122903252, -32.30940107675850470 ) ) ;
#25214 = DIRECTION ( 'NONE',  ( 0.000000000000000000, -8.673617379884037937E-17, -1.000000000000000000 ) ) ;
#25215 = DIRECTION ( 'NONE',  ( 0.000000000000000000, 0.000000000000000000, -1.000000000000000000 ) ) ;
#25216 = CARTESIAN_POINT ( 'NONE',  ( 3.891749269447642767, -3.139164435342899129, -4.200087063816749122 ) ) ;
#25217 = CARTESIAN_POINT ( 'NONE',  ( 16.32187500061451502, 3.027376345333611329, 5.243569643749999010 ) ) ;
#25218 = APPLICATION_CONTEXT ( 'automotive_design' ) ;
#25219 = CARTESIAN_POINT ( 'NONE',  ( 28.38749999999999929, -2.886751345948125991, -5.000000000000000000 ) ) ;
#25220 = CARTESIAN_POINT ( 'NONE',  ( 12.06562500061451537, 3.027376345333613106, -5.243569643749998122 ) ) ;
#25221 = CARTESIAN_POINT ( 'NONE',  ( 28.73437500061451644, 5.492252693125287522, 3.363034840372157021E-16 ) ) ;
#25222 = CARTESIAN_POINT ( 'NONE',  ( 23.03437500061451715, 4.541064518000418104, 2.621784821874999949 ) ) ;
#25223 = CARTESIAN_POINT ( 'NONE',  ( 15.00937500061451502, -5.492252693125287522, -1.008910452111647106E-15 ) ) ;
#25224 = CARTESIAN_POINT ( 'NONE',  ( 10.45312500061451644, 0.000000000000000000, 5.243569643749999010 ) ) ;
#25225 = CARTESIAN_POINT ( 'NONE',  ( 15.34687500061451537, 6.054752690667223547, 3.707466751127219781E-16 ) ) ;
#25226 = ORIENTED_EDGE ( 'NONE', *, *, #30129, .F. ) ;
#25227 = CARTESIAN_POINT ( 'NONE',  ( 25.17187500061451644, 3.027376345333613106, -5.243569643749998122 ) ) ;
#25228 = CARTESIAN_POINT ( 'NONE',  ( 27.25312500061451360, -4.541064518000417216, -2.621784821875001281 ) ) ;
#25229 = CARTESIAN_POINT ( 'NONE',  ( 18.59062500061451573, -3.027376345333614438, 5.243569643749998122 ) ) ;
#25230 = CARTESIAN_POINT ( 'NONE',  ( 28.86562500061451786, 3.027376345333611329, 5.243569643749999010 ) ) ;
#25231 = CARTESIAN_POINT ( 'NONE',  ( 24.20625000122903359, 0.000000000000000000, 4.999999999999998224 ) ) ;
#25232 = CARTESIAN_POINT ( 'NONE',  ( 6.787500000000001421, -2.886751345948125991, -5.000000000000000000 ) ) ;
#25233 = CARTESIAN_POINT ( 'NONE',  ( 18.90000000122902790, -2.886751345948129988, 4.999999999999997335 ) ) ;
#25234 = CARTESIAN_POINT ( 'NONE',  ( -3.999999999999997335, 18.80000000122903003, -27.69059892324149530 ) ) ;
#25235 = CARTESIAN_POINT ( 'NONE',  ( 7.509375000614516793, 2.746126346562645981, -4.756430356249997438 ) ) ;
#25236 = EDGE_LOOP ( 'NONE', ( #59080, #2948, #31606, #30664, #37305, #20434, #38714, #5198, #43902, #58025, #32633, #35601, #63440, #50070, #41430, #72977, #61728, #71874, #45980, #24376, #769, #5004, #7035, #4585, #31028, #63688, #9404, #37069, #1281, #58032, #34424, #60706, #21035, #15793, #11829, #33123, #20132, #44546, #23801, #67273, #56190, #25284, #55707, #34779, #7293, #1882, #21814, #66239 ) ) ;
#25237 = CARTESIAN_POINT ( 'NONE',  ( 14.84999999999999964, -4.330127018922190985, -2.500000000000001332 ) ) ;
#25238 = CARTESIAN_POINT ( 'NONE',  ( 19.68750000000000355, -2.886751345948129988, 4.999999999999997335 ) ) ;
#25239 = CARTESIAN_POINT ( 'NONE',  ( 15.68437500061451573, 6.421520780324663323E-16, -5.243569643749999010 ) ) ;
#25240 = CARTESIAN_POINT ( 'NONE',  ( 13.34062500061451750, -3.027376345333610441, -5.243569643749999898 ) ) ;
#25241 = VERTEX_POINT ( 'NONE', #45263 ) ;
#25242 = CARTESIAN_POINT ( 'NONE',  ( 4.243569643749999898, 16.03437500061451715, -30.00000000000000000 ) ) ;
#25243 = CARTESIAN_POINT ( 'NONE',  ( 5.953125000614519102, 0.000000000000000000, 5.243569643749999010 ) ) ;
#25244 = CARTESIAN_POINT ( 'NONE',  ( -3.756430356249999214, 12.82812499938548534, 27.83122392262697176 ) ) ;
#25245 = CARTESIAN_POINT ( 'NONE',  ( 11.70000000000000284, -4.330127018922190985, -2.500000000000001332 ) ) ;
#25246 = CARTESIAN_POINT ( 'NONE',  ( 29.14687500061451431, 4.119189519843966529, -2.378215178124998275 ) ) ;
#25247 = VECTOR ( 'NONE', #259, 1000.000000000000000 ) ;
#25248 = ORIENTED_EDGE ( 'NONE', *, *, #643, .T. ) ;
#25249 = CARTESIAN_POINT ( 'NONE',  ( 2.121784821875001281, 15.90312500061451573, 33.67503911421598417 ) ) ;
#25250 = CARTESIAN_POINT ( 'NONE',  ( 26.72812500061451502, -4.541064518000419881, 2.621784821874995952 ) ) ;
#25251 = CARTESIAN_POINT ( 'NONE',  ( 7.875000000000000000, 4.330127018922191873, 2.499999999999999556 ) ) ;
#25252 = CARTESIAN_POINT ( 'NONE',  ( 3.756430356249998770, 17.10312499938548214, 32.16877607737302469 ) ) ;
#25253 = CARTESIAN_POINT ( 'NONE',  ( 23.18437500061451573, -4.541064518000419881, 2.621784821874995952 ) ) ;
#25254 = CARTESIAN_POINT ( 'NONE',  ( 20.54062500061451502, -3.027376345333610441, -5.243569643749999898 ) ) ;
#25255 = EDGE_CURVE ( 'NONE', #25148, #48448, #55980, .T. ) ;
#25256 = CARTESIAN_POINT ( 'NONE',  ( -4.243569643749999898, 15.71562500061459211, -32.45002607614398471 ) ) ;
#25257 = CARTESIAN_POINT ( 'NONE',  ( 23.85000000122903430, -2.886751345948129988, 4.999999999999997335 ) ) ;
#25258 = EDGE_CURVE ( 'NONE', #17653, #50451, #33803, .T. ) ;
#25259 = CARTESIAN_POINT ( 'NONE',  ( 6.365625000614518747, 3.027376345333611329, 5.243569643749999010 ) ) ;
#25260 = CARTESIAN_POINT ( 'NONE',  ( 26.78437500061451360, -4.119189519843968306, 2.378215178124996054 ) ) ;
#25261 = CARTESIAN_POINT ( 'NONE',  ( 23.50312500061451360, 0.000000000000000000, 5.243569643749999010 ) ) ;
#25262 = CARTESIAN_POINT ( 'NONE',  ( 11.40937500061451892, 0.000000000000000000, 4.756430356249998326 ) ) ;
#25263 = CARTESIAN_POINT ( 'NONE',  ( -1.878215178124999163, 15.94062499938548427, 26.74683588394047007 ) ) ;
#25264 = CARTESIAN_POINT ( 'NONE',  ( 17.18437500061451573, 4.541064518000418104, 2.621784821874999949 ) ) ;
#25265 = CARTESIAN_POINT ( 'NONE',  ( 25.32187500061451857, 3.027376345333611329, 5.243569643749999010 ) ) ;
#25266 = CARTESIAN_POINT ( 'NONE',  ( -4.243569643749999898, 15.35937500061451644, 30.00000000000000000 ) ) ;
#25267 = CARTESIAN_POINT ( 'NONE',  ( 5.840625000614516615, 6.054752690667223547, 3.707466751127219781E-16 ) ) ;
#25268 = CARTESIAN_POINT ( 'NONE',  ( 29.65312500061451573, 4.541064518000418104, -2.621784821874998173 ) ) ;
#25269 = CARTESIAN_POINT ( 'NONE',  ( 29.72812500061451502, 4.541064518000418104, 2.621784821874999949 ) ) ;
#25270 = CARTESIAN_POINT ( 'NONE',  ( 0.000000000000000000, 10.00000000000000000, -36.00000000000000000 ) ) ;
#25271 = CARTESIAN_POINT ( 'NONE',  ( 3.382222646665033139, 4.052127219167644512, 2.981509777668850614 ) ) ;
#25272 = CARTESIAN_POINT ( 'NONE',  ( 2.840625000614518392, -3.027376345333614438, 5.243569643749998122 ) ) ;
#25273 = CARTESIAN_POINT ( 'NONE',  ( 6.759375000614516793, 4.541064518000418104, -2.621784821874998173 ) ) ;
#25274 = FILL_AREA_STYLE_COLOUR ( '', #49755 ) ;
#25275 = CARTESIAN_POINT ( 'NONE',  ( 17.88750000122903216, 4.330127018922191873, 2.499999999999999556 ) ) ;
#25276 = CARTESIAN_POINT ( 'NONE',  ( 4.134375000614517681, 4.541064518000418104, 2.621784821874999949 ) ) ;
#25277 = B_SPLINE_CURVE_WITH_KNOTS ( 'NONE', 3,
 ( #19478, #65654, #35754, #69744 ),
 .UNSPECIFIED., .F., .F.,
 ( 4, 4 ),
 ( 8.673617379884034509E-19, 0.001150238639792624086 ),
 .UNSPECIFIED. ) ;
#25278 = CARTESIAN_POINT ( 'NONE',  ( 11.55000000122903181, 5.773502691896255534, 3.535250795749688894E-16 ) ) ;
#25279 = CARTESIAN_POINT ( 'NONE',  ( 4.303125000614516971, -4.541064518000417216, -2.621784821875001281 ) ) ;
#25280 = FACE_OUTER_BOUND ( 'NONE', #48232, .T. ) ;
#25281 = CARTESIAN_POINT ( 'NONE',  ( 22.14375000122903359, -2.886751345948125991, -5.000000000000000000 ) ) ;
#25282 = CARTESIAN_POINT ( 'NONE',  ( 14.93437500061451750, 4.541064518000418104, 2.621784821874999949 ) ) ;
#25283 = FACE_OUTER_BOUND ( 'NONE', #35723, .T. ) ;
#25284 = ORIENTED_EDGE ( 'NONE', *, *, #826, .F. ) ;
#25285 = CARTESIAN_POINT ( 'NONE',  ( 22.30312500061451431, -4.541064518000417216, -2.621784821875001281 ) ) ;
#25286 = CARTESIAN_POINT ( 'NONE',  ( 8.203125000614518214, 0.000000000000000000, 5.243569643749999010 ) ) ;
#25287 = CARTESIAN_POINT ( 'NONE',  ( 25.13437500061451502, 6.421520780324663323E-16, -5.243569643749999010 ) ) ;
#25288 = CARTESIAN_POINT ( 'NONE',  ( 7.453125000614516438, -4.541064518000417216, -2.621784821875001281 ) ) ;
#25289 = CYLINDRICAL_SURFACE ( 'NONE', #40350, 4.000000000000000000 ) ;
#25290 =( BOUNDED_CURVE ( )  B_SPLINE_CURVE ( 2, ( #35757, #58278, #69747, #19115, #12507, #36126, #8053, #30587, #2510 ),
 .UNSPECIFIED., .F., .F. ) 
 B_SPLINE_CURVE_WITH_KNOTS ( ( 3, 2, 2, 2, 3 ),
 ( 0.5326086956521739468, 0.5362318840579710644, 0.5434782608695651884, 0.5507246376811594235, 0.5543478260869565410 ),
 .UNSPECIFIED. ) 
 CURVE ( )  GEOMETRIC_REPRESENTATION_ITEM ( )  RATIONAL_B_SPLINE_CURVE ( ( 0.9330127018922194093, 0.9330127018922194093, 1.000000000000000000, 0.8660254037844387076, 1.000000000000000000, 0.8660254037844387076, 1.000000000000000000, 0.9330127018922194093, 0.9330127018922194093 ) ) 
 REPRESENTATION_ITEM ( '' )  );
#25291 = CARTESIAN_POINT ( 'NONE',  ( 11.17500000122903536, 2.886751345948126879, 4.999999999999999112 ) ) ;
#25292 = CARTESIAN_POINT ( 'NONE',  ( 24.51562500061451289, -6.054752690667223547, -1.112240025338166033E-15 ) ) ;
#25293 = CARTESIAN_POINT ( 'NONE',  ( 4.000000000000000000, 19.40000000122903856, -27.69059892324149530 ) ) ;
#25294 = CARTESIAN_POINT ( 'NONE',  ( 9.825000001229033941, 2.886751345948126879, 4.999999999999999112 ) ) ;
#25295 = CARTESIAN_POINT ( 'NONE',  ( 20.65312500061451573, 4.541064518000418104, -2.621784821874998173 ) ) ;
#25296 = CARTESIAN_POINT ( 'NONE',  ( 16.86562500061451786, -6.054752690667223547, -1.112240025338166033E-15 ) ) ;
#25297 = CARTESIAN_POINT ( 'NONE',  ( 28.69687500061451502, -2.746126346562642428, -4.756430356249999214 ) ) ;
#25298 = CARTESIAN_POINT ( 'NONE',  ( 18.45000000000000284, -4.330127018922190985, -2.500000000000001332 ) ) ;
#25299 = CARTESIAN_POINT ( 'NONE',  ( 14.36250000122903359, 0.000000000000000000, 4.999999999999998224 ) ) ;
#25300 = CARTESIAN_POINT ( 'NONE',  ( 11.50312500061451892, -4.541064518000417216, -2.621784821875001281 ) ) ;
#25301 = EDGE_CURVE ( 'NONE', #68959, #13783, #55134, .T. ) ;
#25302 = CARTESIAN_POINT ( 'NONE',  ( 13.19062500061451537, -3.027376345333614438, 5.243569643749998122 ) ) ;
#25303 = CARTESIAN_POINT ( 'NONE',  ( 24.41250000122903430, -4.330127018922190985, -2.500000000000001332 ) ) ;
#25304 = AXIS2_PLACEMENT_3D ( 'NONE', #24577, #36031, #51587 ) ;
#25305 = CARTESIAN_POINT ( 'NONE',  ( 21.57187500061451502, 3.027376345333613106, -5.243569643749998122 ) ) ;
#25306 = CARTESIAN_POINT ( 'NONE',  ( 20.52187500061451786, -6.054752690667223547, -1.112240025338166033E-15 ) ) ;
#25307 = CARTESIAN_POINT ( 'NONE',  ( 14.75625000122903252, 0.000000000000000000, 4.999999999999998224 ) ) ;
#25308 = CARTESIAN_POINT ( 'NONE',  ( 8.587500001229035007, -4.330127018922194537, 2.499999999999995559 ) ) ;
#25309 = CARTESIAN_POINT ( 'NONE',  ( 6.534375000614517148, -4.541064518000419881, 2.621784821874995952 ) ) ;
#25310 = CARTESIAN_POINT ( 'NONE',  ( 23.33437500061451786, 6.421520780324663323E-16, -5.243569643749999010 ) ) ;
#25311 = CARTESIAN_POINT ( 'NONE',  ( 10.46250000000000036, 2.886751345948129099, -4.999999999999997335 ) ) ;
#25312 = AXIS2_PLACEMENT_3D ( 'NONE', #35322, #1721, #46783 ) ;
#25313 = CARTESIAN_POINT ( 'NONE',  ( 21.29062500061451502, -3.027376345333614438, 5.243569643749998122 ) ) ;
#25314 = CARTESIAN_POINT ( 'NONE',  ( 24.15937500061451715, -4.541064518000417216, -2.621784821875001281 ) ) ;
#25315 = CARTESIAN_POINT ( 'NONE',  ( 3.756430356249998770, 19.46562499938548285, 32.16877607737301759 ) ) ;
#25316 = CARTESIAN_POINT ( 'NONE',  ( 23.17500000000000071, 4.330127018922191873, 2.499999999999999556 ) ) ;
#25317 = CARTESIAN_POINT ( 'NONE',  ( 16.48125000122903216, 4.330127018922191873, 2.499999999999999556 ) ) ;
#25318 = CARTESIAN_POINT ( 'NONE',  ( 5.221875000614519813, -6.054752690667223547, -1.112240025338166033E-15 ) ) ;
#25319 = CARTESIAN_POINT ( 'NONE',  ( 18.17812500061451786, -4.541064518000419881, 2.621784821874995952 ) ) ;
#25320 = AXIS2_PLACEMENT_3D ( 'NONE', #53956, #9249, #31784 ) ;
#25321 = ORIENTED_EDGE ( 'NONE', *, *, #28761, .T. ) ;
#25322 = CARTESIAN_POINT ( 'NONE',  ( 11.43750000000000000, 5.773502691896255534, 3.535250795749688401E-16 ) ) ;
#25323 = CARTESIAN_POINT ( 'NONE',  ( 24.81562500061451715, 3.027376345333611329, 5.243569643749999010 ) ) ;
#25324 = CARTESIAN_POINT ( 'NONE',  ( 0.000000000000000000, 20.00000000000000000, 30.00000000000000000 ) ) ;
#25325 = CARTESIAN_POINT ( 'NONE',  ( 1.626862140677534273E-15, 17.86250000000000071, -26.00000000000000355 ) ) ;
#25326 = CARTESIAN_POINT ( 'NONE',  ( 3.999818103236636890, 3.000242528463001435, -30.14366030220596571 ) ) ;
#25327 = CARTESIAN_POINT ( 'NONE',  ( 14.51250000000000107, 2.886751345948129099, -4.999999999999998224 ) ) ;
#25328 = CARTESIAN_POINT ( 'NONE',  ( 25.53750000122903074, 4.330127018922191873, 2.499999999999999556 ) ) ;
#25329 = CARTESIAN_POINT ( 'NONE',  ( 21.51562500061451644, 3.027376345333613106, -5.243569643749998122 ) ) ;
#25330 = EDGE_LOOP ( 'NONE', ( #72511, #29285, #30049, #68871 ) ) ;
#25331 = CARTESIAN_POINT ( 'NONE',  ( 25.42500000000000071, 4.330127018922191873, 2.499999999999999556 ) ) ;
#25332 =( BOUNDED_CURVE ( )  B_SPLINE_CURVE ( 2, ( #22965, #45526, #68056, #17425, #39984, #24056, #22608 ),
 .UNSPECIFIED., .F., .F. ) 
 B_SPLINE_CURVE_WITH_KNOTS ( ( 3, 2, 2, 3 ),
 ( 0.9500000000000000666, 0.9533333333333334769, 0.9566666666666666652, 0.9599999999999999645 ),
 .UNSPECIFIED. ) 
 CURVE ( )  GEOMETRIC_REPRESENTATION_ITEM ( )  RATIONAL_B_SPLINE_CURVE ( ( 0.9999999999999955591, 0.8660254037844431485, 1.000000000000000000, 0.8660254037844387076, 1.000000000000000000, 0.8660254037844387076, 1.000000000000000000 ) ) 
 REPRESENTATION_ITEM ( '' )  );
#25333 = CARTESIAN_POINT ( 'NONE',  ( 23.78437500061451360, 6.421520780324663323E-16, -5.243569643749999010 ) ) ;
#25334 = EDGE_LOOP ( 'NONE', ( #43739, #72236, #21987, #71059 ) ) ;
#25335 = CARTESIAN_POINT ( 'NONE',  ( 4.898587196589411843E-16, 20.00000000000000000, 33.99999999999999289 ) ) ;
#25336 = CARTESIAN_POINT ( 'NONE',  ( 12.62812500061451537, 4.541064518000418104, 2.621784821874999949 ) ) ;
#25337 = CARTESIAN_POINT ( 'NONE',  ( 3.928125000614516527, 6.421520780324663323E-16, -5.243569643749999010 ) ) ;
#25338 = CARTESIAN_POINT ( 'NONE',  ( 16.73437500061451644, -2.746126346562646425, 4.756430356249996549 ) ) ;
#25339 = CARTESIAN_POINT ( 'NONE',  ( 28.26562500061451289, 3.027376345333613106, -5.243569643749998122 ) ) ;
#25340 = CARTESIAN_POINT ( 'NONE',  ( 14.06250000122903288, -4.330127018922190985, -2.500000000000001332 ) ) ;
#25341 = CARTESIAN_POINT ( 'NONE',  ( 18.59999999999999787, 4.330127018922192761, -2.499999999999997780 ) ) ;
#25342 = CARTESIAN_POINT ( 'NONE',  ( 27.86249999999999716, -5.773502691896255534, -1.060575238724906372E-15 ) ) ;
#25343 = CARTESIAN_POINT ( 'NONE',  ( 3.009375000614516793, -4.541064518000417216, -2.621784821875001281 ) ) ;
#25344 = CARTESIAN_POINT ( 'NONE',  ( 6.684375000614518392, 6.421520780324663323E-16, -5.243569643749999010 ) ) ;
#25345 = CARTESIAN_POINT ( 'NONE',  ( 20.44687500061451857, -3.027376345333614438, 5.243569643749998122 ) ) ;
#25346 = CARTESIAN_POINT ( 'NONE',  ( 26.13749999999999929, -2.886751345948109559, -5.000000000000028422 ) ) ;
#25347 = VERTEX_POINT ( 'NONE', #64043 ) ;
#25348 = CARTESIAN_POINT ( 'NONE',  ( 27.66562500061451146, -6.054752690667223547, -1.112240025338166033E-15 ) ) ;
#25349 = CARTESIAN_POINT ( 'NONE',  ( 29.55937500061451573, -4.541064518000417216, -2.621784821875001281 ) ) ;
#25350 = CARTESIAN_POINT ( 'NONE',  ( 3.609375000614516882, 4.541064518000418104, -2.621784821874998173 ) ) ;
#25351 = CARTESIAN_POINT ( 'NONE',  ( 15.48749999999999893, 5.773502691896255534, 3.535250795749688894E-16 ) ) ;
#25352 = CARTESIAN_POINT ( 'NONE',  ( 14.80312500061451608, 4.541064518000418104, -2.621784821874998173 ) ) ;
#25353 = CARTESIAN_POINT ( 'NONE',  ( 16.27499999999999858, 6.123233995736764310E-16, -4.999999999999998224 ) ) ;
#25354 = CARTESIAN_POINT ( 'NONE',  ( 5.000000000000000000, 6.176262757673013563E-16, -5.043301270189223473 ) ) ;
#25355 = CARTESIAN_POINT ( 'NONE',  ( 27.07499999999999929, 6.123233995736764310E-16, -4.999999999999998224 ) ) ;
#25356 = CARTESIAN_POINT ( 'NONE',  ( 17.43750000122903288, 4.330127018922191873, 2.499999999999999556 ) ) ;
#25357 = CARTESIAN_POINT ( 'NONE',  ( 8.906250001229031099, 0.000000000000000000, 4.999999999999998224 ) ) ;
#25358 = CARTESIAN_POINT ( 'NONE',  ( 17.59687500061451715, 5.492252693125287522, 3.363034840372157021E-16 ) ) ;
#25359 = CARTESIAN_POINT ( 'NONE',  ( 6.815625000614517148, 3.027376345333611329, 5.243569643749999010 ) ) ;
#25360 = CARTESIAN_POINT ( 'NONE',  ( 23.52187500061451786, 3.027376345333611329, 5.243569643749999010 ) ) ;
#25361 = CARTESIAN_POINT ( 'NONE',  ( 9.001249775931846008E-16, 16.37187500061451573, 34.90005215228797653 ) ) ;
#25362 = EDGE_CURVE ( 'NONE', #67359, #4004, #62956, .T. ) ;
#25363 = CARTESIAN_POINT ( 'NONE',  ( 24.79687500061451999, 6.054752690667223547, 3.707466751127219781E-16 ) ) ;
#25364 = CARTESIAN_POINT ( 'NONE',  ( 5.962500000000002132, 2.886751345948129099, -4.999999999999998224 ) ) ;
#25365 = CARTESIAN_POINT ( 'NONE',  ( -1.999999999999997113, 11.63750000122903394, 33.46410161513775705 ) ) ;
#25366 = CARTESIAN_POINT ( 'NONE',  ( 12.02812500061451573, 6.421520780324663323E-16, -5.243569643749999010 ) ) ;
#25367 = CARTESIAN_POINT ( 'NONE',  ( 5.175000001229033586, 2.886751345948129099, -4.999999999999998224 ) ) ;
#25368 = CARTESIAN_POINT ( 'NONE',  ( 8.784375000614518925, -4.541064518000419881, 2.621784821874995952 ) ) ;
#25369 = CARTESIAN_POINT ( 'NONE',  ( -2.065650683794913789, 4.559369103593685857, -26.56528590568888504 ) ) ;
#25370 = VERTEX_POINT ( 'NONE', #1649 ) ;
#25371 = CARTESIAN_POINT ( 'NONE',  ( 11.76562500061451644, 3.027376345333611329, 5.243569643749999010 ) ) ;
#25372 = LINE ( 'NONE', #35362, #53257 ) ;
#25373 = CARTESIAN_POINT ( 'NONE',  ( 22.80000000122903359, 5.773502691896255534, 3.535250795749688894E-16 ) ) ;
#25374 = CARTESIAN_POINT ( 'NONE',  ( 9.571875000614518569, 3.027376345333611329, 5.243569643749999010 ) ) ;
#25375 = CARTESIAN_POINT ( 'NONE',  ( 11.39062500061451644, -3.027376345333614438, 5.243569643749998122 ) ) ;
#25376 = CARTESIAN_POINT ( 'NONE',  ( 28.48125000122902861, 6.123233995736764310E-16, -4.999999999999998224 ) ) ;
#25377 = CARTESIAN_POINT ( 'NONE',  ( 21.53437500061451715, 6.421520780324663323E-16, -5.243569643749999010 ) ) ;
#25378 = CARTESIAN_POINT ( 'NONE',  ( 0.6522905807966048464, 20.75364847883808395, 33.69936292076899065 ) ) ;
#25379 = VECTOR ( 'NONE', #53047, 1000.000000000000000 ) ;
#25380 = CARTESIAN_POINT ( 'NONE',  ( 7.537500000000002309, -2.886751345948130876, 4.999999999999996447 ) ) ;
#25381 = CARTESIAN_POINT ( 'NONE',  ( 8.324999999999999289, 4.330127018922191873, 2.499999999999999556 ) ) ;
#25382 = CARTESIAN_POINT ( 'NONE',  ( -4.243569643749998122, 13.59687500061451892, -27.54997392385601174 ) ) ;
#25383 = CARTESIAN_POINT ( 'NONE',  ( 15.53437500061451715, -4.541064518000419881, 2.621784821874995952 ) ) ;
#25384 = CARTESIAN_POINT ( 'NONE',  ( 17.25000000122903288, -2.886751345948125991, -5.000000000000000000 ) ) ;
#25385 = AXIS2_PLACEMENT_3D ( 'NONE', #26451, #19057, #70780 ) ;
#25386 = CARTESIAN_POINT ( 'NONE',  ( 11.44687500061451857, -3.027376345333614438, 5.243569643749998122 ) ) ;
#25387 = CARTESIAN_POINT ( 'NONE',  ( 2.121784821874999061, 18.75312500061451715, -33.67503911421598417 ) ) ;
#25388 = CARTESIAN_POINT ( 'NONE',  ( 17.85000000122903430, 5.773502691896255534, 3.535250795749688894E-16 ) ) ;
#25389 = CARTESIAN_POINT ( 'NONE',  ( 11.76562500061451644, 3.027376345333611329, 5.243569643749999010 ) ) ;
#25390 = ORIENTED_EDGE ( 'NONE', *, *, #5722, .T. ) ;
#25391 = VECTOR ( 'NONE', #44191, 1000.000000000000000 ) ;
#25392 = CARTESIAN_POINT ( 'NONE',  ( 16.53750000000000142, -2.886751345948129988, 4.999999999999997335 ) ) ;
#25393 = DIRECTION ( 'NONE',  ( 0.000000000000000000, 0.000000000000000000, 1.000000000000000000 ) ) ;
#25394 = CARTESIAN_POINT ( 'NONE',  ( 12.15937500061451892, 4.541064518000418104, -2.621784821874998173 ) ) ;
#25395 = CYLINDRICAL_SURFACE ( 'NONE', #20861, 4.999999999999998224 ) ;
#25396 = CARTESIAN_POINT ( 'NONE',  ( 13.31250000122903288, 4.330127018922192761, -2.499999999999997780 ) ) ;
#25397 = CARTESIAN_POINT ( 'NONE',  ( 20.10000000122903074, 5.773502691896255534, 3.535250795749688894E-16 ) ) ;
#25398 = CARTESIAN_POINT ( 'NONE',  ( 17.46562500061451217, 3.027376345333613106, -5.243569643749998122 ) ) ;
#25399 = CARTESIAN_POINT ( 'NONE',  ( 20.12812500061451715, 6.421520780324663323E-16, -5.243569643749999010 ) ) ;
#25400 = CARTESIAN_POINT ( 'NONE',  ( 28.05000000122903359, -2.886751345948125991, -5.000000000000000000 ) ) ;
#25401 = EDGE_CURVE ( 'NONE', #10265, #48564, #32904, .T. ) ;
#25402 = CARTESIAN_POINT ( 'NONE',  ( 25.01249999999999929, 2.886751345948126879, 4.999999999999999112 ) ) ;
#25403 = DIRECTION ( 'NONE',  ( 0.000000000000000000, 0.000000000000000000, -1.000000000000000000 ) ) ;
#25404 = CARTESIAN_POINT ( 'NONE',  ( 28.91250000000000497, 2.886751345948129099, -4.999999999999998224 ) ) ;
#25405 = CARTESIAN_POINT ( 'NONE',  ( 29.10937500061451644, -4.541064518000417216, -2.621784821875001281 ) ) ;
#25406 = CARTESIAN_POINT ( 'NONE',  ( 26.53125000122902932, -4.330127018922194537, 2.499999999999995559 ) ) ;
#25407 = CARTESIAN_POINT ( 'NONE',  ( 9.001249775931846008E-16, 14.12187500061451750, -25.09994784771203058 ) ) ;
#25408 = CARTESIAN_POINT ( 'NONE',  ( 4.050000001229035362, -2.886751345948129988, 4.999999999999997335 ) ) ;
#25409 = CARTESIAN_POINT ( 'NONE',  ( 29.85937500061451644, 0.000000000000000000, 5.243569643749999010 ) ) ;
#25410 = CARTESIAN_POINT ( 'NONE',  ( 6.571875000614517681, -6.054752690667223547, -1.112240025338166033E-15 ) ) ;
#25411 = CARTESIAN_POINT ( 'NONE',  ( 27.77812500061451573, 6.421520780324663323E-16, -5.243569643749999010 ) ) ;
#25412 = CARTESIAN_POINT ( 'NONE',  ( 4.809375000614516615, -4.541064518000417216, -2.621784821875001281 ) ) ;
#25413 = CARTESIAN_POINT ( 'NONE',  ( 14.36249999999999893, -5.773502691896255534, -1.060575238724906372E-15 ) ) ;
#25414 = CARTESIAN_POINT ( 'NONE',  ( 7.500000000000000000, 0.000000000000000000, 4.999999999999998224 ) ) ;
#25415 = CARTESIAN_POINT ( 'NONE',  ( 5.184375000614516615, -4.541064518000419881, 2.621784821874995952 ) ) ;
#25416 = CARTESIAN_POINT ( 'NONE',  ( 12.04687500061451821, -3.027376345333610441, -5.243569643749999898 ) ) ;
#25417 = CARTESIAN_POINT ( 'NONE',  ( 4.949999999999999289, -4.330127018922190985, -2.500000000000001332 ) ) ;
#25418 = VECTOR ( 'NONE', #56358, 1000.000000000000000 ) ;
#25419 = CARTESIAN_POINT ( 'NONE',  ( -2.121784821874996840, 14.47812500061459495, 33.67503911421598417 ) ) ;
#25420 = CARTESIAN_POINT ( 'NONE',  ( 1.999999999999997335, 13.32499999999999929, 33.46410161513775705 ) ) ;
#25421 = CARTESIAN_POINT ( 'NONE',  ( 6.299999999999999822, -4.330127018922190985, -2.500000000000001332 ) ) ;
#25422 = CARTESIAN_POINT ( 'NONE',  ( 15.64687500061451608, 4.119189519843966529, -2.378215178124998275 ) ) ;
#25423 = CARTESIAN_POINT ( 'NONE',  ( 20.72812500061451502, 4.541064518000418104, 2.621784821874999949 ) ) ;
#25424 = CARTESIAN_POINT ( 'NONE',  ( 9.928125000614517859, 4.541064518000418104, 2.621784821874999949 ) ) ;
#25425 = CARTESIAN_POINT ( 'NONE',  ( 24.23437500061451644, 5.492252693125287522, 3.363034840372157021E-16 ) ) ;
#25426 = CARTESIAN_POINT ( 'NONE',  ( 9.684375000614517504, -4.541064518000419881, 2.621784821874995952 ) ) ;
#25427 = CARTESIAN_POINT ( 'NONE',  ( 25.12499999999999645, -4.330127018922194537, 2.499999999999995559 ) ) ;
#25428 = CARTESIAN_POINT ( 'NONE',  ( 21.26250000122903572, -4.330127018922190985, -2.500000000000001332 ) ) ;
#25429 = CARTESIAN_POINT ( 'NONE',  ( 28.30312500061451431, 4.541064518000418104, -2.621784821874998173 ) ) ;
#25430 = DIRECTION ( 'NONE',  ( 0.000000000000000000, 0.000000000000000000, -1.000000000000000000 ) ) ;
#25431 = AXIS2_PLACEMENT_3D ( 'NONE', #50625, #45084, #33982 ) ;
#25432 = CARTESIAN_POINT ( 'NONE',  ( 9.871875000614517504, 3.027376345333613106, -5.243569643749998122 ) ) ;
#25433 = CARTESIAN_POINT ( 'NONE',  ( 14.78437500061451715, 6.421520780324663323E-16, -5.243569643749999010 ) ) ;
#25434 = CARTESIAN_POINT ( 'NONE',  ( 26.44687500061451502, -3.027376345333610441, -5.243569643749999898 ) ) ;
#25435 = DIRECTION ( 'NONE',  ( 1.000000000000000000, -0.000000000000000000, -0.000000000000000000 ) ) ;
#25436 = CARTESIAN_POINT ( 'NONE',  ( 13.01249999999999929, -5.773502691896255534, -1.060575238724906372E-15 ) ) ;
#25437 = CARTESIAN_POINT ( 'NONE',  ( 21.15937500061451715, 4.541064518000418104, -2.621784821874998173 ) ) ;
#25438 = CARTESIAN_POINT ( 'NONE',  ( 12.87187500061451750, -6.054752690667223547, -1.112240025338166033E-15 ) ) ;
#25439 = CARTESIAN_POINT ( 'NONE',  ( 1.878215178124997609, 13.46562499938548285, 33.25316411605952993 ) ) ;
#25440 = CARTESIAN_POINT ( 'NONE',  ( 23.96249999999999858, 2.886751345948129099, -4.999999999999998224 ) ) ;
#25441 = CARTESIAN_POINT ( 'NONE',  ( 4.000000000000000000, 14.75000000000000178, 30.00000000000000000 ) ) ;
#25442 = CARTESIAN_POINT ( 'NONE',  ( -4.243569643749999898, 11.72187500061451892, -32.45002607614398471 ) ) ;
#25443 = CARTESIAN_POINT ( 'NONE',  ( 23.67187500061451999, -5.492252693125287522, -1.008910452111647106E-15 ) ) ;
#25444 = CARTESIAN_POINT ( 'NONE',  ( 14.31562500061451537, 3.027376345333613106, -5.243569643749998122 ) ) ;
#25445 = CARTESIAN_POINT ( 'NONE',  ( 3.600000000000002309, -4.330127018922190985, -2.500000000000001332 ) ) ;
#25446 = FACE_OUTER_BOUND ( 'NONE', #34479, .T. ) ;
#25447 = CARTESIAN_POINT ( 'NONE',  ( 25.72499999999999787, 6.123233995736764310E-16, -4.999999999999998224 ) ) ;
#25448 = CARTESIAN_POINT ( 'NONE',  ( 11.66249999999999964, -5.773502691896255534, -1.060575238724906372E-15 ) ) ;
#25449 = CARTESIAN_POINT ( 'NONE',  ( -1.999999999999997113, 17.48750000122903359, 33.46410161513775705 ) ) ;
#25450 = CARTESIAN_POINT ( 'NONE',  ( 11.43750000122903465, 6.123233995736764310E-16, -4.999999999999998224 ) ) ;
#25451 = CARTESIAN_POINT ( 'NONE',  ( 22.39687500061451075, -3.027376345333610441, -5.243569643749999898 ) ) ;
#25452 = CARTESIAN_POINT ( 'NONE',  ( 16.88437500061451502, -4.541064518000419881, 2.621784821874995952 ) ) ;
#25453 = CARTESIAN_POINT ( 'NONE',  ( -3.999999999999997335, 16.43750000000000000, -27.69059892324149530 ) ) ;
#25454 = ORIENTED_EDGE ( 'NONE', *, *, #46306, .F. ) ;
#25455 = CARTESIAN_POINT ( 'NONE',  ( 19.37812500061451715, 4.541064518000418104, 2.621784821874999949 ) ) ;
#25456 = CARTESIAN_POINT ( 'NONE',  ( 4.303125000614516971, -4.541064518000417216, -2.621784821875001281 ) ) ;
#25457 = CARTESIAN_POINT ( 'NONE',  ( 16.88437500061451502, -4.541064518000419881, 2.621784821874995952 ) ) ;
#25458 = CARTESIAN_POINT ( 'NONE',  ( 28.54687500061451644, -3.027376345333614438, 5.243569643749998122 ) ) ;
#25459 = CARTESIAN_POINT ( 'NONE',  ( 4.715625000614516615, -6.054752690667223547, -1.112240025338166033E-15 ) ) ;
#25460 = CARTESIAN_POINT ( 'NONE',  ( 20.54062500061451502, -3.027376345333610441, -5.243569643749999898 ) ) ;
#25461 = CARTESIAN_POINT ( 'NONE',  ( 2.121784821874999061, 15.15312500061451750, 26.32496088578401583 ) ) ;
#25462 = CARTESIAN_POINT ( 'NONE',  ( 17.13750000122903216, -4.330127018922194537, 2.499999999999995559 ) ) ;
#25463 = CARTESIAN_POINT ( 'NONE',  ( 12.00937500061451857, -4.119189519843965641, -2.378215178125001383 ) ) ;
#25464 = CARTESIAN_POINT ( 'NONE',  ( 6.628125000614517148, 6.421520780324663323E-16, -5.243569643749999010 ) ) ;
#25465 = CARTESIAN_POINT ( 'NONE',  ( 29.46562500061451573, -6.054752690667223547, -1.112240025338166033E-15 ) ) ;
#25466 = CARTESIAN_POINT ( 'NONE',  ( 24.12187500061451217, -6.054752690667223547, -1.112240025338166033E-15 ) ) ;
#25467 = CARTESIAN_POINT ( 'NONE',  ( 14.12812500061451715, -4.541064518000419881, 2.621784821874995952 ) ) ;
#25468 = CARTESIAN_POINT ( 'NONE',  ( 24.45000000122903572, -2.886751345948125991, -5.000000000000000000 ) ) ;
#25469 = CARTESIAN_POINT ( 'NONE',  ( 24.02812500061451573, -4.541064518000419881, 2.621784821874995952 ) ) ;
#25470 = CARTESIAN_POINT ( 'NONE',  ( 20.18437500061451573, 6.421520780324663323E-16, -5.243569643749999010 ) ) ;
#25471 = CARTESIAN_POINT ( 'NONE',  ( 14.46562500061451750, 3.027376345333611329, 5.243569643749999010 ) ) ;
#25472 = CARTESIAN_POINT ( 'NONE',  ( -2.121784821874996840, 14.98437500061451644, 33.67503911421598417 ) ) ;
#25473 = CARTESIAN_POINT ( 'NONE',  ( 20.09062500061451573, -3.027376345333610441, -5.243569643749999898 ) ) ;
#25474 = CARTESIAN_POINT ( 'NONE',  ( 29.20312500061451644, 4.541064518000418104, -2.621784821874998173 ) ) ;
#25475 = VERTEX_POINT ( 'NONE', #17526 ) ;
#25476 = EDGE_LOOP ( 'NONE', ( #56251, #14235, #24452, #25615 ) ) ;
#25477 = CARTESIAN_POINT ( 'NONE',  ( 23.47499999999999787, 6.123233995736764310E-16, -4.999999999999998224 ) ) ;
#25478 = CARTESIAN_POINT ( 'NONE',  ( 2.000000000000001332, 11.15000000000000213, -26.53589838486224650 ) ) ;
#25479 = CARTESIAN_POINT ( 'NONE',  ( 13.05000000122903536, -2.886751345948130876, 4.999999999999996447 ) ) ;
#25480 = CARTESIAN_POINT ( 'NONE',  ( 26.27812500061451573, -4.541064518000419881, 2.621784821874995952 ) ) ;
#25481 = CARTESIAN_POINT ( 'NONE',  ( 8.428125000614517859, 6.421520780324663323E-16, -5.243569643749999010 ) ) ;
#25482 = CARTESIAN_POINT ( 'NONE',  ( 19.50000000122903288, -2.886751345948125991, -5.000000000000000000 ) ) ;
#25483 = CARTESIAN_POINT ( 'NONE',  ( 26.01562500061451289, 3.027376345333613106, -5.243569643749998122 ) ) ;
#25484 = CARTESIAN_POINT ( 'NONE',  ( 25.76249999999999929, 2.886751345948129099, -4.999999999999998224 ) ) ;
#25485 = CARTESIAN_POINT ( 'NONE',  ( 27.25312500061451360, -4.541064518000417216, -2.621784821875001281 ) ) ;
#25486 = CARTESIAN_POINT ( 'NONE',  ( 7.490625000614516082, -3.027376345333610441, -5.243569643749999898 ) ) ;
#25487 = ORIENTED_EDGE ( 'NONE', *, *, #26658, .F. ) ;
#25488 = EDGE_CURVE ( 'NONE', #9351, #1970, #33331, .T. ) ;
#25489 = PRODUCT_DEFINITION_SHAPE ( 'NONE', 'NONE',  #73122 ) ;
#25490 = CARTESIAN_POINT ( 'NONE',  ( 23.05312500061451431, 0.000000000000000000, 5.243569643749999010 ) ) ;
#25491 = CARTESIAN_POINT ( 'NONE',  ( 4.303125000614516971, -4.541064518000417216, -2.621784821875001281 ) ) ;
#25492 = CARTESIAN_POINT ( 'NONE',  ( 13.24687500061451750, -2.746126346562646425, 4.756430356249996549 ) ) ;
#25493 = CARTESIAN_POINT ( 'NONE',  ( 29.17500000000000071, -4.330127018922194537, 2.499999999999995559 ) ) ;
#25494 = DIRECTION ( 'NONE',  ( -0.000000000000000000, -1.000000000000000000, -0.000000000000000000 ) ) ;
#25495 = CARTESIAN_POINT ( 'NONE',  ( 13.87500000000000178, -4.330127018922194537, 2.499999999999995559 ) ) ;
#25496 =( BOUNDED_CURVE ( )  B_SPLINE_CURVE ( 2, ( #26656, #70981, #9292, #19987, #71722, #3396, #43645, #20356, #37364 ),
 .UNSPECIFIED., .F., .F. ) 
 B_SPLINE_CURVE_WITH_KNOTS ( ( 3, 2, 2, 2, 3 ),
 ( 0.2083333333333333426, 0.2129629629629629650, 0.2222222222222222099, 0.2314814814814814825, 0.2361111111111111049 ),
 .UNSPECIFIED. ) 
 CURVE ( )  GEOMETRIC_REPRESENTATION_ITEM ( )  RATIONAL_B_SPLINE_CURVE ( ( 0.9330127018922194093, 0.9330127018922195203, 1.000000000000000000, 0.8660254037844387076, 1.000000000000000000, 0.8660254037844387076, 1.000000000000000000, 0.9330127018922194093, 0.9330127018922194093 ) ) 
 REPRESENTATION_ITEM ( '' )  );
#25497 = CARTESIAN_POINT ( 'NONE',  ( 14.55937500061451573, 0.000000000000000000, 5.243569643749999010 ) ) ;
#25498 = CARTESIAN_POINT ( 'NONE',  ( 9.562500001229032875, -4.330127018922190985, -2.500000000000001332 ) ) ;
#25499 = CARTESIAN_POINT ( 'NONE',  ( 15.64687500061451608, -3.027376345333610441, -5.243569643749999898 ) ) ;
#25500 = CARTESIAN_POINT ( 'NONE',  ( 14.81250000000000000, -5.773502691896255534, -1.060575238724906372E-15 ) ) ;
#25501 = CARTESIAN_POINT ( 'NONE',  ( 9.309375000614517504, -4.541064518000417216, -2.621784821875001281 ) ) ;
#25502 = CARTESIAN_POINT ( 'NONE',  ( -3.000416591977282496E-16, 11.59062500061451750, -34.90005215228797653 ) ) ;
#25503 = LINE ( 'NONE', #48048, #61880 ) ;
#25504 = CARTESIAN_POINT ( 'NONE',  ( 13.69687500061451679, -3.027376345333614438, 5.243569643749998122 ) ) ;
#25505 = DIRECTION ( 'NONE',  ( -1.000000000000000000, -0.000000000000000000, -0.000000000000000000 ) ) ;
#25506 = CARTESIAN_POINT ( 'NONE',  ( 21.44062500061452070, -3.027376345333610441, -5.243569643749999898 ) ) ;
#25507 = CARTESIAN_POINT ( 'NONE',  ( 45.00000000000000000, 6.363961030679004871, 4.863961030678849440 ) ) ;
#25508 = CARTESIAN_POINT ( 'NONE',  ( 21.30000000122903359, -2.886751345948126435, -5.000000000000000000 ) ) ;
#25509 = CARTESIAN_POINT ( 'NONE',  ( 25.95937500061451431, -4.541064518000417216, -2.621784821875001281 ) ) ;
#25510 = CARTESIAN_POINT ( 'NONE',  ( 4.978125000614518569, 4.541064518000418104, 2.621784821874999949 ) ) ;
#25511 = CARTESIAN_POINT ( 'NONE',  ( 22.80937500061451573, 2.746126346562645981, -4.756430356249997438 ) ) ;
#25512 = CARTESIAN_POINT ( 'NONE',  ( 17.18437500061451573, 4.541064518000418104, 2.621784821874999949 ) ) ;
#25513 = CARTESIAN_POINT ( 'NONE',  ( 9.871875000614517504, 4.119189519843966529, 2.378215178124999607 ) ) ;
#25514 = CARTESIAN_POINT ( 'NONE',  ( 29.10000000122903074, 5.773502691896255534, 3.535250795749688894E-16 ) ) ;
#25515 = CARTESIAN_POINT ( 'NONE',  ( 6.759375000614516793, 4.541064518000418104, -2.621784821874998173 ) ) ;
#25516 = CARTESIAN_POINT ( 'NONE',  ( 16.09687500061452070, -3.027376345333610441, -5.243569643749999898 ) ) ;
#25517 = CARTESIAN_POINT ( 'NONE',  ( -3.999940174399832848, 25.00001595349299421, 30.26464805816245729 ) ) ;
#25518 = CARTESIAN_POINT ( 'NONE',  ( 25.01249999999999929, 2.886751345948126879, 4.999999999999999112 ) ) ;
#25519 = CARTESIAN_POINT ( 'NONE',  ( 27.75937500061451502, -4.541064518000417216, -2.621784821875001281 ) ) ;
#25520 = CARTESIAN_POINT ( 'NONE',  ( 3.756430356250000546, 12.79062499938548392, 27.83122392262697886 ) ) ;
#25521 = CARTESIAN_POINT ( 'NONE',  ( 5.737500001229033586, 4.330127018922191873, 2.499999999999999556 ) ) ;
#25522 = ORIENTED_EDGE ( 'NONE', *, *, #15421, .T. ) ;
#25523 = CARTESIAN_POINT ( 'NONE',  ( 8.625000000000000000, 6.123233995736764310E-16, -4.999999999999998224 ) ) ;
#25524 = CARTESIAN_POINT ( 'NONE',  ( 10.39687500061451608, 0.000000000000000000, 4.756430356249998326 ) ) ;
#25525 = CARTESIAN_POINT ( 'NONE',  ( 21.74062500061451431, -3.027376345333614438, 5.243569643749998122 ) ) ;
#25526 = CARTESIAN_POINT ( 'NONE',  ( 11.51250000000000107, 2.886751345948126879, 4.999999999999999112 ) ) ;
#25527 = CARTESIAN_POINT ( 'NONE',  ( 5.990625000614517859, -3.027376345333614438, 5.243569643749998122 ) ) ;
#25528 = CARTESIAN_POINT ( 'NONE',  ( 19.16250000000000142, 2.886751345948126879, 4.999999999999999112 ) ) ;
#25529 = EDGE_CURVE ( 'NONE', #63939, #68252, #35609, .T. ) ;
#25530 = CARTESIAN_POINT ( 'NONE',  ( 19.30312500061451786, 4.541064518000418104, -2.621784821874998173 ) ) ;
#25531 = CARTESIAN_POINT ( 'NONE',  ( 28.53750000122903074, 6.123233995736764310E-16, -4.999999999999998224 ) ) ;
#25532 = CARTESIAN_POINT ( 'NONE',  ( 23.51250000122903216, -4.330127018922190985, -2.500000000000001332 ) ) ;
#25533 = CARTESIAN_POINT ( 'NONE',  ( -3.756430356250000102, 20.06562499938548072, 30.00000000000000000 ) ) ;
#25534 = CARTESIAN_POINT ( 'NONE',  ( 4.425000000000001599, -4.330127018922194537, 2.499999999999995559 ) ) ;
#25535 = ADVANCED_FACE ( 'NONE', ( #40440 ), #58492, .F. ) ;
#25536 = ORIENTED_EDGE ( 'NONE', *, *, #15762, .T. ) ;
#25537 = CARTESIAN_POINT ( 'NONE',  ( 20.27812500061451573, 4.541064518000418104, 2.621784821874999949 ) ) ;
#25538 = CARTESIAN_POINT ( 'NONE',  ( 26.69062500061451715, -3.027376345333614438, 5.243569643749998122 ) ) ;
#25539 = CARTESIAN_POINT ( 'NONE',  ( 24.04687500061451644, -3.027376345333614438, 5.243569643749998122 ) ) ;
#25540 = CARTESIAN_POINT ( 'NONE',  ( 7.950000000000001954, 0.000000000000000000, 4.999999999999998224 ) ) ;
#25541 = CARTESIAN_POINT ( 'NONE',  ( 12.14062500061451821, 6.054752690667223547, 3.707466751127219781E-16 ) ) ;
#25542 = CARTESIAN_POINT ( 'NONE',  ( 28.56562500061451715, -6.054752690667223547, -1.112240025338166033E-15 ) ) ;
#25543 = CARTESIAN_POINT ( 'NONE',  ( 16.92187500061451999, -6.054752690667223547, -1.112240025338166033E-15 ) ) ;
#25544 = CARTESIAN_POINT ( 'NONE',  ( 9.065625000614517148, 3.027376345333611329, 5.243569643749999010 ) ) ;
#25545 = CARTESIAN_POINT ( 'NONE',  ( 7.125000001229032875, 2.886751345948193936, 4.999999999999883649 ) ) ;
#25546 = CARTESIAN_POINT ( 'NONE',  ( -4.243569643749999898, 12.65937500061451715, 30.00000000000000000 ) ) ;
#25547 =( BOUNDED_CURVE ( )  B_SPLINE_CURVE ( 2, ( #22632, #22275, #39280, #5290, #49998, #45903, #33724 ),
 .UNSPECIFIED., .F., .F. ) 
 B_SPLINE_CURVE_WITH_KNOTS ( ( 3, 2, 2, 3 ),
 ( 0.3916666666666667740, 0.3944444444444444864, 0.3972222222222221433, 0.3999999999999999112 ),
 .UNSPECIFIED. ) 
 CURVE ( )  GEOMETRIC_REPRESENTATION_ITEM ( )  RATIONAL_B_SPLINE_CURVE ( ( 0.9999999999999946709, 0.8660254037844440367, 1.000000000000000000, 0.8660254037844387076, 1.000000000000000000, 0.8660254037844440367, 0.9999999999999946709 ) ) 
 REPRESENTATION_ITEM ( '' )  );
#25548 = CARTESIAN_POINT ( 'NONE',  ( 24.33750000122903145, -4.330127018922194537, 2.499999999999995559 ) ) ;
#25549 = CARTESIAN_POINT ( 'NONE',  ( 20.33437500061451786, 4.119189519843966529, 2.378215178124999607 ) ) ;
#25550 = CARTESIAN_POINT ( 'NONE',  ( 13.26562500061451289, -6.054752690667223547, -1.112240025338166033E-15 ) ) ;
#25551 = CARTESIAN_POINT ( 'NONE',  ( 10.50937500061451679, 0.000000000000000000, 5.243569643749999010 ) ) ;
#25552 = CARTESIAN_POINT ( 'NONE',  ( 9.459375000614517859, 4.541064518000418104, -2.621784821874998173 ) ) ;
#25554 = EDGE_CURVE ( 'NONE', #5101, #2103, #43266, .T. ) ;
#25553 = CARTESIAN_POINT ( 'NONE',  ( 17.25937500061451502, 0.000000000000000000, 5.243569643749999010 ) ) ;
#25555 = VERTEX_POINT ( 'NONE', #52607 ) ;
#25556 = CARTESIAN_POINT ( 'NONE',  ( 7.285825576177820915E-16, 10.00000000000000000, 36.00000000000000000 ) ) ;
#25557 = CARTESIAN_POINT ( 'NONE',  ( 22.45312500061451644, 4.541064518000418104, -2.621784821874998173 ) ) ;
#25558 = CARTESIAN_POINT ( 'NONE',  ( 16.20937500061451786, 4.541064518000418104, -2.621784821874998173 ) ) ;
#25559 = CARTESIAN_POINT ( 'NONE',  ( 22.60312500061451857, 0.000000000000000000, 5.243569643749999010 ) ) ;
#25560 = CARTESIAN_POINT ( 'NONE',  ( 1.999999999999998668, 13.10000000000000142, 26.53589838486224650 ) ) ;
#25561 = CARTESIAN_POINT ( 'NONE',  ( 27.17812500061451786, -4.541064518000419881, 2.621784821874995952 ) ) ;
#25562 = CARTESIAN_POINT ( 'NONE',  ( 6.750000001229033764, -2.886751345948129988, 4.999999999999997335 ) ) ;
#25563 = VERTEX_POINT ( 'NONE', #13422 ) ;
#25564 = CARTESIAN_POINT ( 'NONE',  ( 30.00000000000000000, 0.000000000000000000, 4.999999999999998224 ) ) ;
#25565 = CARTESIAN_POINT ( 'NONE',  ( -2.000000000000000000, 19.02499999999999858, -33.46410161513775705 ) ) ;
#25566 = CARTESIAN_POINT ( 'NONE',  ( 24.18750000122903288, 4.330127018922191873, 2.499999999999999556 ) ) ;
#25567 = CARTESIAN_POINT ( 'NONE',  ( 1.878215178124997609, 15.37812499938548427, 33.25316411605952993 ) ) ;
#25568 = EDGE_CURVE ( 'NONE', #60311, #26800, #40889, .T. ) ;
#25569 = CARTESIAN_POINT ( 'NONE',  ( 6.946875000614517681, -3.027376345333614438, 5.243569643749998122 ) ) ;
#25570 = CARTESIAN_POINT ( 'NONE',  ( 12.78749999999999787, 5.773502691896255534, 3.535250795749688401E-16 ) ) ;
#25571 = CARTESIAN_POINT ( 'NONE',  ( 14.61562500061451608, -6.054752690667223547, -1.112240025338166033E-15 ) ) ;
#25572 = CARTESIAN_POINT ( 'NONE',  ( 8.071875000614518569, 3.027376345333613106, -5.243569643749998122 ) ) ;
#25573 = CARTESIAN_POINT ( 'NONE',  ( 26.13750000122903216, -4.330127018922194537, 2.499999999999995559 ) ) ;
#25574 = CARTESIAN_POINT ( 'NONE',  ( 17.14687500061451786, 6.054752690667223547, 3.707466751127219781E-16 ) ) ;
#25575 = CARTESIAN_POINT ( 'NONE',  ( 4.546875000614517326, 6.054752690667223547, 3.707466751127219781E-16 ) ) ;
#25576 = CARTESIAN_POINT ( 'NONE',  ( 0.000000000000000000, 20.00000000000000000, 26.00000000000000000 ) ) ;
#25577 = CARTESIAN_POINT ( 'NONE',  ( 5.840625000614516615, 6.054752690667223547, 3.707466751127219781E-16 ) ) ;
#25578 = CARTESIAN_POINT ( 'NONE',  ( 14.31562500061451537, 3.027376345333613106, -5.243569643749998122 ) ) ;
#25579 =( BOUNDED_CURVE ( )  B_SPLINE_CURVE ( 2, ( #69372, #63451, #2484, #31290, #41646, #19455, #35371 ),
 .UNSPECIFIED., .F., .F. ) 
 B_SPLINE_CURVE_WITH_KNOTS ( ( 3, 2, 2, 3 ),
 ( 0.2250000000000000611, 0.2277777777777778290, 0.2305555555555555969, 0.2333333333333333648 ),
 .UNSPECIFIED. ) 
 CURVE ( )  GEOMETRIC_REPRESENTATION_ITEM ( )  RATIONAL_B_SPLINE_CURVE ( ( 0.9999999999999973355, 0.8660254037844413721, 1.000000000000000000, 0.8660254037844387076, 1.000000000000000000, 0.8660254037844373753, 1.000000000000001332 ) ) 
 REPRESENTATION_ITEM ( '' )  );
#25580 = EDGE_LOOP ( 'NONE', ( #12646, #39818, #13345, #62161 ) ) ;
#25581 = CARTESIAN_POINT ( 'NONE',  ( 12.21562500061451573, 3.027376345333611329, 5.243569643749999010 ) ) ;
#25582 = CARTESIAN_POINT ( 'NONE',  ( 4.725000001229034297, 2.886751345948129099, -4.999999999999998224 ) ) ;
#25583 = CARTESIAN_POINT ( 'NONE',  ( 9.703125000614514661, -4.541064518000417216, -2.621784821875001281 ) ) ;
#25584 = CARTESIAN_POINT ( 'NONE',  ( 21.75937500061451502, 0.000000000000000000, 4.756430356249998326 ) ) ;
#25585 = CARTESIAN_POINT ( 'NONE',  ( 10.01250000000000107, 2.886751345948129099, -4.999999999999998224 ) ) ;
#25586 = CARTESIAN_POINT ( 'NONE',  ( 5.137500001229033941, 6.123233995736764310E-16, -4.999999999999998224 ) ) ;
#25587 = CARTESIAN_POINT ( 'NONE',  ( 19.20000000000000284, 0.000000000000000000, 4.999999999999998224 ) ) ;
#25588 = CARTESIAN_POINT ( 'NONE',  ( 15.98437500061451821, -4.541064518000419881, 2.621784821874995952 ) ) ;
#25589 = CARTESIAN_POINT ( 'NONE',  ( 16.08750000122903501, 4.330127018922191873, 2.499999999999999556 ) ) ;
#25590 = CARTESIAN_POINT ( 'NONE',  ( 21.71249999999999858, 2.886751345948129099, -4.999999999999998224 ) ) ;
#25591 =( BOUNDED_CURVE ( )  B_SPLINE_CURVE ( 2, ( #44797, #66964, #43694, #66216, #71771, #54770, #15963 ),
 .UNSPECIFIED., .F., .F. ) 
 B_SPLINE_CURVE_WITH_KNOTS ( ( 3, 2, 2, 3 ),
 ( 0.2083333333333332871, 0.2111111111111110827, 0.2138888888888889062, 0.2166666666666667296 ),
 .UNSPECIFIED. ) 
 CURVE ( )  GEOMETRIC_REPRESENTATION_ITEM ( )  RATIONAL_B_SPLINE_CURVE ( ( 1.000000000000002665, 0.8660254037844360431, 1.000000000000000000, 0.8660254037844387076, 1.000000000000000000, 0.8660254037844360431, 1.000000000000002665 ) ) 
 REPRESENTATION_ITEM ( '' )  );
#25592 = CARTESIAN_POINT ( 'NONE',  ( 4.243569643749999010, 18.26562500061451644, -32.45002607614398471 ) ) ;
#25593 = CARTESIAN_POINT ( 'NONE',  ( 9.225000000000001421, 4.330127018922191873, 2.499999999999999556 ) ) ;
#25594 = FACE_OUTER_BOUND ( 'NONE', #39293, .T. ) ;
#25595 = CARTESIAN_POINT ( 'NONE',  ( 29.35312500061451502, 0.000000000000000000, 5.243569643749999010 ) ) ;
#25596 = CARTESIAN_POINT ( 'NONE',  ( 3.366080804335946919, -3.697228694398128290, 3.718268762498968094 ) ) ;
#25597 = CARTESIAN_POINT ( 'NONE',  ( -3.137519842735245283E-14, 14.37500000122903288, 34.00000000000000000 ) ) ;
#25598 = CARTESIAN_POINT ( 'NONE',  ( 16.47187500061452070, -6.054752690667223547, -1.112240025338166033E-15 ) ) ;
#25599 = CARTESIAN_POINT ( 'NONE',  ( 29.36250000000000071, 2.886751345948129099, -4.999999999999998224 ) ) ;
#25600 = CARTESIAN_POINT ( 'NONE',  ( 11.65312500061451573, 4.541064518000418104, -2.621784821874998173 ) ) ;
#25601 = CARTESIAN_POINT ( 'NONE',  ( 8.193750001229034297, -2.886751345948125991, -5.000000000000000000 ) ) ;
#25602 = CARTESIAN_POINT ( 'NONE',  ( 25.05937500061451573, -4.541064518000417216, -2.621784821875001281 ) ) ;
#25603 = CARTESIAN_POINT ( 'NONE',  ( 16.73437500061451644, -2.746126346562646425, 4.756430356249996549 ) ) ;
#25604 = CARTESIAN_POINT ( 'NONE',  ( 9.028125000614517504, 4.541064518000418104, 2.621784821874999949 ) ) ;
#25605 = CARTESIAN_POINT ( 'NONE',  ( 12.08437500061451608, 6.421520780324663323E-16, -5.243569643749999010 ) ) ;
#25606 = ORIENTED_EDGE ( 'NONE', *, *, #17223, .T. ) ;
#25607 = CARTESIAN_POINT ( 'NONE',  ( 24.27187500061452141, 3.027376345333613106, -5.243569643749998122 ) ) ;
#25608 = CARTESIAN_POINT ( 'NONE',  ( 27.74062500061451431, -3.027376345333610441, -5.243569643749999898 ) ) ;
#25609 = DIRECTION ( 'NONE',  ( 0.000000000000000000, 1.000000000000000000, 0.000000000000000000 ) ) ;
#25610 = CARTESIAN_POINT ( 'NONE',  ( 6.375000000000001776, 6.123233995736764310E-16, -4.999999999999998224 ) ) ;
#25611 = VECTOR ( 'NONE', #35367, 1000.000000000000000 ) ;
#25612 = CARTESIAN_POINT ( 'NONE',  ( 16.98750000122903359, 4.330127018922191873, 2.499999999999999556 ) ) ;
#25613 = CARTESIAN_POINT ( 'NONE',  ( 27.18750000122903288, 6.123233995736764310E-16, -4.999999999999998224 ) ) ;
#25614 = CARTESIAN_POINT ( 'NONE',  ( 7.621875000614515727, 4.119189519843966529, 2.378215178124999607 ) ) ;
#25615 = ORIENTED_EDGE ( 'NONE', *, *, #38259, .F. ) ;
#25616 = CARTESIAN_POINT ( 'NONE',  ( 16.16250000000000142, -5.773502691896255534, -1.060575238724906372E-15 ) ) ;
#25617 = CARTESIAN_POINT ( 'NONE',  ( 20.17499999999999716, -4.330127018922194537, 2.499999999999995559 ) ) ;
#25618 = CARTESIAN_POINT ( 'NONE',  ( 12.70312500061451821, 0.000000000000000000, 5.243569643749999010 ) ) ;
#25619 = ORIENTED_EDGE ( 'NONE', *, *, #9386, .F. ) ;
#25620 = CARTESIAN_POINT ( 'NONE',  ( -1.243387493232115393E-14, 16.21250000000000213, 26.00000000000000000 ) ) ;
#25621 = CARTESIAN_POINT ( 'NONE',  ( -4.243569643749997233, 15.84687500061451715, -27.54997392385601174 ) ) ;
#25622 = CARTESIAN_POINT ( 'NONE',  ( 5.990625000614517859, -3.027376345333614438, 5.243569643749998122 ) ) ;
#25623 = CARTESIAN_POINT ( 'NONE',  ( 1.878215178125000495, 13.16562499938548392, 26.74683588394047007 ) ) ;
#25624 = CARTESIAN_POINT ( 'NONE',  ( 12.37500000000000000, 4.330127018922191873, 2.499999999999999556 ) ) ;
#25625 = CARTESIAN_POINT ( 'NONE',  ( 27.98437500061451644, -2.746126346562646425, 4.756430356249996549 ) ) ;
#25626 = ORIENTED_EDGE ( 'NONE', *, *, #26495, .T. ) ;
#25627 = CARTESIAN_POINT ( 'NONE',  ( 9.001249775931846008E-16, 15.41562500061451679, 34.90005215228797653 ) ) ;
#25628 = CARTESIAN_POINT ( 'NONE',  ( 27.70312500061451289, -4.541064518000417216, -2.621784821875001281 ) ) ;
#25629 = CARTESIAN_POINT ( 'NONE',  ( 8.250000000000000000, 4.330127018922192761, -2.499999999999997780 ) ) ;
#25630 = CARTESIAN_POINT ( 'NONE',  ( -1.878215178124999163, 18.64062499938548356, 26.74683588394047007 ) ) ;
#25631 = CARTESIAN_POINT ( 'NONE',  ( 23.67187500061451999, -6.054752690667223547, -1.112240025338166033E-15 ) ) ;
#25632 = CARTESIAN_POINT ( 'NONE',  ( 18.47812500061451857, 4.541064518000418104, 2.621784821874999949 ) ) ;
#25633 = CARTESIAN_POINT ( 'NONE',  ( -2.121784821874999949, 13.42812500061459602, -33.67503911421598417 ) ) ;
#25634 = CARTESIAN_POINT ( 'NONE',  ( 23.02500000122903145, -5.773502691896255534, -1.060575238724906372E-15 ) ) ;
#25635 = CARTESIAN_POINT ( 'NONE',  ( 4.265625000614517326, -6.054752690667223547, -1.112240025338166033E-15 ) ) ;
#25636 = CARTESIAN_POINT ( 'NONE',  ( 26.59687500061451360, 5.492252693125287522, 3.363034840372157021E-16 ) ) ;
#25637 = CARTESIAN_POINT ( 'NONE',  ( 20.50312500061451715, -4.541064518000417216, -2.621784821875001281 ) ) ;
#25638 = CARTESIAN_POINT ( 'NONE',  ( 9.834375000614517859, 5.824947211148865298E-16, -4.756430356249998326 ) ) ;
#25639 = CARTESIAN_POINT ( 'NONE',  ( 3.756430356250000546, 14.92812499938548321, 27.83122392262697886 ) ) ;
#25641 = EDGE_CURVE ( 'NONE', #48104, #71409, #37646, .T. ) ;
#25640 = CARTESIAN_POINT ( 'NONE',  ( 17.52187500061451431, 3.027376345333613106, -5.243569643749998122 ) ) ;
#25642 = CARTESIAN_POINT ( 'NONE',  ( 16.77187500061451786, 3.027376345333611329, 5.243569643749999010 ) ) ;
#25643 = CARTESIAN_POINT ( 'NONE',  ( 23.82187500061451502, 3.027376345333613106, -5.243569643749998122 ) ) ;
#25644 = CARTESIAN_POINT ( 'NONE',  ( 9.001249775931846008E-16, 13.22187500061451892, 34.90005215228797653 ) ) ;
#25645 = CARTESIAN_POINT ( 'NONE',  ( 5.765625000614519102, 3.027376345333613106, -5.243569643749998122 ) ) ;
#25646 = CARTESIAN_POINT ( 'NONE',  ( 28.67812500061451431, 6.421520780324663323E-16, -5.243569643749999010 ) ) ;
#25647 = CARTESIAN_POINT ( 'NONE',  ( 28.52812500061451573, -4.541064518000419881, 2.621784821874995952 ) ) ;
#25648 = DIRECTION ( 'NONE',  ( -1.000000000000000000, -0.000000000000000000, -0.000000000000000000 ) ) ;
#25649 = CARTESIAN_POINT ( 'NONE',  ( 3.923201271487455344, -3.982966846201708488, -3.588438345016263131 ) ) ;
#25650 = CARTESIAN_POINT ( 'NONE',  ( 3.628125000614518036, 4.541064518000418104, 2.621784821874999949 ) ) ;
#25651 = CARTESIAN_POINT ( 'NONE',  ( 7.209375000614519635, 4.541064518000418104, -2.621784821874998173 ) ) ;
#25652 = APPLICATION_PROTOCOL_DEFINITION ( 'draft international standard', 'automotive_design', 1998, #43151 ) ;
#25653 = CARTESIAN_POINT ( 'NONE',  ( 15.45000000122903216, -2.886751345948125991, -5.000000000000000000 ) ) ;
#25654 = CARTESIAN_POINT ( 'NONE',  ( 3.684375000614518836, 4.541064518000418104, 2.621784821874999949 ) ) ;
#25655 = CARTESIAN_POINT ( 'NONE',  ( 11.17500000122903536, 2.886751345948126879, 4.999999999999999112 ) ) ;
#25656 = CARTESIAN_POINT ( 'NONE',  ( 4.453125000614517326, 4.541064518000418104, -2.621784821874998173 ) ) ;
#25657 = CARTESIAN_POINT ( 'NONE',  ( 45.00000000000000000, 2.500000000000000000, -3.500000000000000000 ) ) ;
#25658 = CARTESIAN_POINT ( 'NONE',  ( 20.04375000122902861, 5.773502691896255534, 3.535250795749688894E-16 ) ) ;
#25659 = CARTESIAN_POINT ( 'NONE',  ( 13.28437500061451715, -4.541064518000419881, 2.621784821874995952 ) ) ;
#25660 = FACE_OUTER_BOUND ( 'NONE', #9039, .T. ) ;
#25661 = ORIENTED_EDGE ( 'NONE', *, *, #56109, .F. ) ;
#25662 = CARTESIAN_POINT ( 'NONE',  ( 23.27812500061451573, 6.421520780324663323E-16, -5.243569643749999010 ) ) ;
#25663 = CARTESIAN_POINT ( 'NONE',  ( 6.928125000614516082, -4.541064518000419881, 2.621784821874995952 ) ) ;
#25664 = CARTESIAN_POINT ( 'NONE',  ( 23.89687500061451786, 6.054752690667223547, 3.707466751127219781E-16 ) ) ;
#25665 = CARTESIAN_POINT ( 'NONE',  ( 7.603125000614517681, 4.541064518000418104, -2.621784821874998173 ) ) ;
#25666 = CARTESIAN_POINT ( 'NONE',  ( 23.11875000122902790, 2.886751345948101122, -5.000000000000046185 ) ) ;
#25667 = CARTESIAN_POINT ( 'NONE',  ( 8.812500001229034652, 4.330127018922192761, -2.499999999999997780 ) ) ;
#25668 = CARTESIAN_POINT ( 'NONE',  ( 23.35312500061451857, 4.541064518000418104, -2.621784821874998173 ) ) ;
#25669 = CARTESIAN_POINT ( 'NONE',  ( -4.243569643749999898, 11.66562500061451679, -32.45002607614398471 ) ) ;
#25670 = CARTESIAN_POINT ( 'NONE',  ( 11.47500000122903252, 2.886751345948129099, -4.999999999999998224 ) ) ;
#25671 = CARTESIAN_POINT ( 'NONE',  ( 18.81562500061452070, 3.027376345333613106, -5.243569643749998122 ) ) ;
#25672 = CARTESIAN_POINT ( 'NONE',  ( 17.12812500061451715, 4.541064518000418104, 2.621784821874999949 ) ) ;
#25673 = CARTESIAN_POINT ( 'NONE',  ( 27.45937500061451786, 4.119189519843966529, -2.378215178124998275 ) ) ;
#25674 = CARTESIAN_POINT ( 'NONE',  ( 17.36249999999999716, 2.886751345948126879, 4.999999999999999112 ) ) ;
#25675 = CARTESIAN_POINT ( 'NONE',  ( 14.32500000122903394, 2.886751345948126879, 4.999999999999999112 ) ) ;
#25676 = EDGE_CURVE ( 'NONE', #31771, #32794, #26356, .T. ) ;
#25677 = AXIS2_PLACEMENT_3D ( 'NONE', #45724, #56786, #56439 ) ;
#25678 = CARTESIAN_POINT ( 'NONE',  ( 10.97812500061451679, -4.541064518000419881, 2.621784821874995952 ) ) ;
#25679 = CARTESIAN_POINT ( 'NONE',  ( 14.57812500061451644, -4.541064518000419881, 2.621784821874995952 ) ) ;
#25680 = AXIS2_PLACEMENT_3D ( 'NONE', #64748, #2700, #25215 ) ;
#25681 = CARTESIAN_POINT ( 'NONE',  ( 23.06250000122903288, -4.330127018922190985, -2.500000000000001332 ) ) ;
#25682 = CARTESIAN_POINT ( 'NONE',  ( 21.98437500061451644, 6.421520780324663323E-16, -5.243569643749999010 ) ) ;
#25683 = CARTESIAN_POINT ( 'NONE',  ( 20.48437500061451289, -4.541064518000419881, 2.621784821874995952 ) ) ;
#25684 = CARTESIAN_POINT ( 'NONE',  ( -4.000000000000000888, 18.61250000000000426, 32.30940107675850470 ) ) ;
#25685 = EDGE_CURVE ( 'NONE', #72457, #29842, #45218, .T. ) ;
#25686 = CARTESIAN_POINT ( 'NONE',  ( 6.937500001229033764, 6.123233995736764310E-16, -4.999999999999998224 ) ) ;
#25687 = CARTESIAN_POINT ( 'NONE',  ( 7.059375000614518392, -4.541064518000417216, -2.621784821875001281 ) ) ;
#25688 = CARTESIAN_POINT ( 'NONE',  ( 23.85937500061451644, 4.541064518000418104, -2.621784821874998173 ) ) ;
#25689 = DIRECTION ( 'NONE',  ( 1.000000000000000000, 0.000000000000000000, 0.000000000000000000 ) ) ;
#25690 = CARTESIAN_POINT ( 'NONE',  ( 18.70312500061451644, -4.541064518000417216, -2.621784821875001281 ) ) ;
#25691 = CARTESIAN_POINT ( 'NONE',  ( 25.20937500061451431, 4.541064518000418104, -2.621784821874998173 ) ) ;
#25692 = CARTESIAN_POINT ( 'NONE',  ( -3.756430356250000990, 20.66562499938548569, 32.16877607737301048 ) ) ;
#25693 = DIRECTION ( 'NONE',  ( -0.4999999999999975575, 0.000000000000000000, -0.8660254037844400399 ) ) ;
#25694 = CARTESIAN_POINT ( 'NONE',  ( 4.321875000614517681, -6.054752690667223547, -1.112240025338166033E-15 ) ) ;
#25695 = CARTESIAN_POINT ( 'NONE',  ( 16.86562500061451786, -6.054752690667223547, -1.112240025338166033E-15 ) ) ;
#25696 = VERTEX_POINT ( 'NONE', #59222 ) ;
#25697 = CARTESIAN_POINT ( 'NONE',  ( 0.000000000000000000, 20.00000000000000000, 30.00000000000000000 ) ) ;
#25698 = CARTESIAN_POINT ( 'NONE',  ( 25.94062500061451715, -3.027376345333610441, -5.243569643749999898 ) ) ;
#25699 = CARTESIAN_POINT ( 'NONE',  ( -1.999999999999997113, 10.73750000122903536, -26.53589838486224295 ) ) ;
#25700 = DIRECTION ( 'NONE',  ( 0.000000000000000000, 0.000000000000000000, 1.000000000000000000 ) ) ;
#25701 = CARTESIAN_POINT ( 'NONE',  ( 14.10000000000000142, 4.330127018922192761, -2.499999999999997780 ) ) ;
#25702 = CARTESIAN_POINT ( 'NONE',  ( 24.18750000122903288, 4.330127018922191873, 2.499999999999999556 ) ) ;
#25703 = CARTESIAN_POINT ( 'NONE',  ( 18.47812500061451857, 4.541064518000418104, 2.621784821874999949 ) ) ;
#25704 = ORIENTED_EDGE ( 'NONE', *, *, #15134, .T. ) ;
#25705 = CARTESIAN_POINT ( 'NONE',  ( 22.34999999999999787, 0.000000000000000000, 4.999999999999998224 ) ) ;
#25706 = CARTESIAN_POINT ( 'NONE',  ( 24.83437500061451431, 4.541064518000418104, 2.621784821874999949 ) ) ;
#25707 = ORIENTED_EDGE ( 'NONE', *, *, #17544, .T. ) ;
#25708 = CARTESIAN_POINT ( 'NONE',  ( 13.38750000122903394, 4.330127018922191873, 2.499999999999999556 ) ) ;
#25709 = CARTESIAN_POINT ( 'NONE',  ( 12.21562500061451573, 3.027376345333611329, 5.243569643749999010 ) ) ;
#25710 = CARTESIAN_POINT ( 'NONE',  ( 3.965625000614515727, 3.027376345333613106, -5.243569643749998122 ) ) ;
#25711 = CARTESIAN_POINT ( 'NONE',  ( 16.39687500061451431, -4.119189519843965641, -2.378215178125001383 ) ) ;
#25712 = CARTESIAN_POINT ( 'NONE',  ( 26.09062500061451573, 6.054752690667223547, 3.707466751127219781E-16 ) ) ;
#25713 = CARTESIAN_POINT ( 'NONE',  ( 11.88750000122903216, 6.123233995736764310E-16, -4.999999999999998224 ) ) ;
#25714 = CARTESIAN_POINT ( 'NONE',  ( 20.02500000000000213, 4.330127018922191873, 2.499999999999999556 ) ) ;
#25715 = CARTESIAN_POINT ( 'NONE',  ( 25.68750000000000000, -2.886751345948125991, -5.000000000000000000 ) ) ;
#25716 = CARTESIAN_POINT ( 'NONE',  ( 3.268712465558684332, -4.091009155385299856, -2.914164288643219081 ) ) ;
#25717 = CARTESIAN_POINT ( 'NONE',  ( 7.884375000614517681, -4.541064518000419881, 2.621784821874995952 ) ) ;
#25718 = CARTESIAN_POINT ( 'NONE',  ( 16.20937500061451786, 4.541064518000418104, -2.621784821874998173 ) ) ;
#25719 = CARTESIAN_POINT ( 'NONE',  ( 8.681250001229031454, 6.123233995736764310E-16, -4.999999999999998224 ) ) ;
#25720 = ORIENTED_EDGE ( 'NONE', *, *, #56271, .T. ) ;
#25721 = CARTESIAN_POINT ( 'NONE',  ( 27.51562500061451644, 3.027376345333611329, 5.243569643749999010 ) ) ;
#25722 = CARTESIAN_POINT ( 'NONE',  ( 26.55937500061451573, 4.541064518000418104, -2.621784821874998173 ) ) ;
#25723 = CARTESIAN_POINT ( 'NONE',  ( 2.896875000614518747, -3.027376345333614438, 5.243569643749998122 ) ) ;
#25724 = AXIS2_PLACEMENT_3D ( 'NONE', #40058, #17139, #29325 ) ;
#25725 = CARTESIAN_POINT ( 'NONE',  ( 15.00000000000000000, 4.330127018922192761, -2.499999999999997780 ) ) ;
#25726 = CARTESIAN_POINT ( 'NONE',  ( 13.97812500061451679, 4.541064518000418104, 2.621784821874999949 ) ) ;
#25727 = CARTESIAN_POINT ( 'NONE',  ( 45.00000000000000000, 6.123233995736764310E-16, -4.999999999999998224 ) ) ;
#25728 = CARTESIAN_POINT ( 'NONE',  ( 29.27812500061451573, 4.541064518000418104, 2.621784821874999949 ) ) ;
#25729 = CARTESIAN_POINT ( 'NONE',  ( 18.75000000122903288, 5.773502691896255534, 3.535250795749688894E-16 ) ) ;
#25730 = FACE_OUTER_BOUND ( 'NONE', #22702, .T. ) ;
#25731 = CARTESIAN_POINT ( 'NONE',  ( 16.99687500061451573, -2.746126346562642428, -4.756430356249999214 ) ) ;
#25732 = CARTESIAN_POINT ( 'NONE',  ( 4.753125000614515372, -4.541064518000417216, -2.621784821875001281 ) ) ;
#25733 = CARTESIAN_POINT ( 'NONE',  ( 24.94687500061451502, -3.027376345333614438, 5.243569643749998122 ) ) ;
#25735 = CARTESIAN_POINT ( 'NONE',  ( 4.243569643749999898, 17.38437500061451502, 30.00000000000000000 ) ) ;
#25734 =( BOUNDED_CURVE ( )  B_SPLINE_CURVE ( 2, ( #69664, #51953, #23862, #34587, #6527, #29059, #30860 ),
 .UNSPECIFIED., .F., .F. ) 
 B_SPLINE_CURVE_WITH_KNOTS ( ( 3, 2, 2, 3 ),
 ( 0.5300000000000000266, 0.5333333333333333259, 0.5366666666666667362, 0.5400000000000001465 ),
 .UNSPECIFIED. ) 
 CURVE ( )  GEOMETRIC_REPRESENTATION_ITEM ( )  RATIONAL_B_SPLINE_CURVE ( ( 1.000000000000000000, 0.8660254037844387076, 1.000000000000000000, 0.8660254037844387076, 1.000000000000000000, 0.8660254037844342667, 1.000000000000004441 ) ) 
 REPRESENTATION_ITEM ( '' )  );
#25736 = CARTESIAN_POINT ( 'NONE',  ( 24.27187500061452141, 3.027376345333613106, -5.243569643749998122 ) ) ;
#25737 = CARTESIAN_POINT ( 'NONE',  ( 5.025000000000002132, 6.123233995736764310E-16, -4.999999999999998224 ) ) ;
#25738 = CARTESIAN_POINT ( 'NONE',  ( 3.999999999999998668, 10.92500000122903536, 27.69059892324149175 ) ) ;
#25739 = CARTESIAN_POINT ( 'NONE',  ( 11.39062500061451644, -3.027376345333614438, 5.243569643749998122 ) ) ;
#25740 = CARTESIAN_POINT ( 'NONE',  ( 3.337500001229034563, 6.123233995736764310E-16, -4.999999999999998224 ) ) ;
#25741 = CARTESIAN_POINT ( 'NONE',  ( 10.09687500061451715, -3.027376345333614438, 5.243569643749998122 ) ) ;
#25742 = CARTESIAN_POINT ( 'NONE',  ( -1.092898315830475919, 4.886665047895959013, -26.14245196482272604 ) ) ;
#25743 = ORIENTED_EDGE ( 'NONE', *, *, #32902, .T. ) ;
#25744 = CARTESIAN_POINT ( 'NONE',  ( 10.45312500061451644, 0.000000000000000000, 5.243569643749999010 ) ) ;
#25745 = CARTESIAN_POINT ( 'NONE',  ( 14.37187500061451928, 3.027376345333613106, -5.243569643749998122 ) ) ;
#25746 = CYLINDRICAL_SURFACE ( 'NONE', #7279, 4.999999999999998224 ) ;
#25747 = CARTESIAN_POINT ( 'NONE',  ( 22.46250000122903501, 0.000000000000000000, 4.999999999999998224 ) ) ;
#25748 = CARTESIAN_POINT ( 'NONE',  ( 10.95937500061451964, 0.000000000000000000, 5.243569643749999010 ) ) ;
#25749 = CARTESIAN_POINT ( 'NONE',  ( 13.45312500061451466, 4.541064518000418104, -2.621784821874998173 ) ) ;
#25750 = CARTESIAN_POINT ( 'NONE',  ( 29.23125000122903216, -4.330127018922194537, 2.499999999999995559 ) ) ;
#25751 = CARTESIAN_POINT ( 'NONE',  ( 20.63437500061451857, 6.421520780324663323E-16, -5.243569643749999010 ) ) ;
#25752 = LINE ( 'NONE', #31661, #19491 ) ;
#25753 = CARTESIAN_POINT ( 'NONE',  ( -1.071796769724488563, 12.10490381179670116, -26.00000000000000000 ) ) ;
#25754 = CYLINDRICAL_SURFACE ( 'NONE', #24212, 4.999999999999998224 ) ;
#25755 = CARTESIAN_POINT ( 'NONE',  ( -2.121784821874999949, 13.48437500061451821, -33.67503911421598417 ) ) ;
#25756 = CARTESIAN_POINT ( 'NONE',  ( 14.93437500061451750, 4.541064518000418104, 2.621784821874999949 ) ) ;
#25757 = CARTESIAN_POINT ( 'NONE',  ( 14.96250000122903323, -4.330127018922190985, -2.500000000000001332 ) ) ;
#25758 = CARTESIAN_POINT ( 'NONE',  ( 12.23437500061451821, 4.541064518000418104, 2.621784821874999949 ) ) ;
#25759 = CARTESIAN_POINT ( 'NONE',  ( 4.243569643749999010, 18.26562500061451644, -32.45002607614398471 ) ) ;
#25760 = CARTESIAN_POINT ( 'NONE',  ( 17.43750000122903288, 4.330127018922191873, 2.499999999999999556 ) ) ;
#25761 = CARTESIAN_POINT ( 'NONE',  ( 11.46562500061451573, -6.054752690667223547, -1.112240025338166033E-15 ) ) ;
#25762 = ORIENTED_EDGE ( 'NONE', *, *, #67527, .F. ) ;
#25763 = CARTESIAN_POINT ( 'NONE',  ( 16.01249999999999929, 2.886751345948126879, 4.999999999999999112 ) ) ;
#25764 = CARTESIAN_POINT ( 'NONE',  ( 18.03749999999999787, -2.886751345948126435, -5.000000000000000000 ) ) ;
#25765 = CARTESIAN_POINT ( 'NONE',  ( 10.92187500061451644, 3.027376345333611329, 5.243569643749999010 ) ) ;
#25766 = DIRECTION ( 'NONE',  ( 0.000000000000000000, -1.000000000000000000, -0.000000000000000000 ) ) ;
#25767 = CARTESIAN_POINT ( 'NONE',  ( 12.07500000122903216, 2.886751345948126879, 4.999999999999999112 ) ) ;
#25768 = CARTESIAN_POINT ( 'NONE',  ( 20.40000000122903145, -2.886751345948125991, -5.000000000000000000 ) ) ;
#25769 = CARTESIAN_POINT ( 'NONE',  ( 18.62812500061451715, -4.541064518000419881, 2.621784821874995952 ) ) ;
#25770 = CARTESIAN_POINT ( 'NONE',  ( 20.09062500061451573, -3.027376345333610441, -5.243569643749999898 ) ) ;
#25771 = CARTESIAN_POINT ( 'NONE',  ( 27.56250000122902932, -4.330127018922190985, -2.500000000000001332 ) ) ;
#25772 = CARTESIAN_POINT ( 'NONE',  ( 3.965625000614515727, 3.027376345333613106, -5.243569643749998122 ) ) ;
#25773 = CARTESIAN_POINT ( 'NONE',  ( 24.71250000000000213, -5.773502691896255534, -1.060575238724906372E-15 ) ) ;
#25774 = DIRECTION ( 'NONE',  ( -0.000000000000000000, -1.000000000000000000, -0.000000000000000000 ) ) ;
#25775 = CARTESIAN_POINT ( 'NONE',  ( 7.434375000614519280, -4.119189519843968306, 2.378215178124996054 ) ) ;
#25776 = CARTESIAN_POINT ( 'NONE',  ( 28.35937500061451289, 4.541064518000418104, -2.621784821874998173 ) ) ;
#25777 = CARTESIAN_POINT ( 'NONE',  ( -3.000416591977282496E-16, 12.99687500061451750, -34.90005215228797653 ) ) ;
#25778 = EDGE_CURVE ( 'NONE', #55885, #7649, #28162, .T. ) ;
#25779 = CARTESIAN_POINT ( 'NONE',  ( 3.750000001229034652, -2.886751345948125991, -5.000000000000000000 ) ) ;
#25780 = CARTESIAN_POINT ( 'NONE',  ( 3.750000000000000000, 4.330127018922192761, -2.499999999999997780 ) ) ;
#25781 =( BOUNDED_CURVE ( )  B_SPLINE_CURVE ( 2, ( #54685, #55055, #14787, #42873, #70948, #61314, #54329 ),
 .UNSPECIFIED., .F., .F. ) 
 B_SPLINE_CURVE_WITH_KNOTS ( ( 3, 2, 2, 3 ),
 ( 0.008333333333333315870, 0.01111111111111108898, 0.01388888888888885863, 0.01666666666666663174 ),
 .UNSPECIFIED. ) 
 CURVE ( )  GEOMETRIC_REPRESENTATION_ITEM ( )  RATIONAL_B_SPLINE_CURVE ( ( 1.000000000000000888, 0.8660254037844378194, 1.000000000000000000, 0.8660254037844387076, 1.000000000000000000, 0.8660254037844403729, 0.9999999999999983347 ) ) 
 REPRESENTATION_ITEM ( '' )  );
#25782 = CARTESIAN_POINT ( 'NONE',  ( 16.38749999999999929, 5.773502691896255534, 3.535250795749688401E-16 ) ) ;
#25783 = CARTESIAN_POINT ( 'NONE',  ( 8.146875000614516082, 6.054752690667223547, 3.707466751127219781E-16 ) ) ;
#25784 = CARTESIAN_POINT ( 'NONE',  ( 25.04062500061451502, -3.027376345333610441, -5.243569643749999898 ) ) ;
#25785 = CYLINDRICAL_SURFACE ( 'NONE', #58978, 4.000000000000000000 ) ;
#25786 = CARTESIAN_POINT ( 'NONE',  ( -1.964573642069360249, 9.807014569943699911, -24.32727479091799694 ) ) ;
#25787 = CARTESIAN_POINT ( 'NONE',  ( -1.071796769724490339, 19.30490381179669868, 34.00000000000000000 ) ) ;
#25788 = CARTESIAN_POINT ( 'NONE',  ( 5.034375000614519813, 4.541064518000418104, 2.621784821874999949 ) ) ;
#25789 = CARTESIAN_POINT ( 'NONE',  ( 9.271875000614516082, -6.054752690667223547, -1.112240025338166033E-15 ) ) ;
#25790 = CARTESIAN_POINT ( 'NONE',  ( 4.200000000000001954, 4.330127018922192761, -2.499999999999997780 ) ) ;
#25791 = CARTESIAN_POINT ( 'NONE',  ( 4.243569643749999898, 11.44062500061459708, 32.45002607614398471 ) ) ;
#25792 = CARTESIAN_POINT ( 'NONE',  ( 29.09999999999999787, 0.000000000000000000, 4.999999999999998224 ) ) ;
#25793 = CARTESIAN_POINT ( 'NONE',  ( 5.325000000000000178, -4.330127018922194537, 2.499999999999995559 ) ) ;
#25794 = CARTESIAN_POINT ( 'NONE',  ( 15.68437500061451750, 5.492252693125287522, 3.363034840372157021E-16 ) ) ;
#25795 = ORIENTED_EDGE ( 'NONE', *, *, #46306, .T. ) ;
#25796 = CARTESIAN_POINT ( 'NONE',  ( 19.64062500061451644, -3.027376345333610441, -5.243569643749999898 ) ) ;
#25797 = CARTESIAN_POINT ( 'NONE',  ( 9.815625000614518925, 3.027376345333613106, -5.243569643749998122 ) ) ;
#25798 = CARTESIAN_POINT ( 'NONE',  ( 23.67187500061451289, 5.824947211148865298E-16, -4.756430356249998326 ) ) ;
#25799 = CARTESIAN_POINT ( 'NONE',  ( 5.934375000614517504, 4.541064518000418104, 2.621784821874999949 ) ) ;
#25800 = CARTESIAN_POINT ( 'NONE',  ( 26.51249999999999929, -5.773502691896255534, -1.060575238724906372E-15 ) ) ;
#25801 = CARTESIAN_POINT ( 'NONE',  ( 19.98750000122903359, 6.123233995736764310E-16, -4.999999999999998224 ) ) ;
#25802 = CARTESIAN_POINT ( 'NONE',  ( 28.37812500061451715, 4.541064518000418104, 2.621784821874999949 ) ) ;
#25803 = CARTESIAN_POINT ( 'NONE',  ( 0.000000000000000000, 12.50000000000000000, 30.00000000000000000 ) ) ;
#25804 = CARTESIAN_POINT ( 'NONE',  ( 9.309375000614517504, -4.541064518000417216, -2.621784821875001281 ) ) ;
#25805 = CARTESIAN_POINT ( 'NONE',  ( 13.88437500061451679, 6.421520780324663323E-16, -5.243569643749999010 ) ) ;
#25806 = CARTESIAN_POINT ( 'NONE',  ( 23.18437500061451573, -4.541064518000419881, 2.621784821874995952 ) ) ;
#25807 = CYLINDRICAL_SURFACE ( 'NONE', #2968, 4.999999999999998224 ) ;
#25808 = CARTESIAN_POINT ( 'NONE',  ( 13.83749999999999858, -2.886751345948129988, 4.999999999999997335 ) ) ;
#25809 = CARTESIAN_POINT ( 'NONE',  ( 20.55937500061451573, -4.541064518000417216, -2.621784821875001281 ) ) ;
#25810 = CARTESIAN_POINT ( 'NONE',  ( 12.68437500061451573, 4.541064518000418104, 2.621784821874999949 ) ) ;
#25811 = CARTESIAN_POINT ( 'NONE',  ( 2.655984681222220721E-16, 12.75312499938548427, 25.66244784525396483 ) ) ;
#25812 = CARTESIAN_POINT ( 'NONE',  ( 24.41250000000000142, 2.886751345948129099, -4.999999999999998224 ) ) ;
#25813 = CARTESIAN_POINT ( 'NONE',  ( 3.999999999999998668, 15.16250000000000142, 32.30940107675850470 ) ) ;
#25814 = CARTESIAN_POINT ( 'NONE',  ( -4.243569643749999898, 11.30937500061451928, -30.00000000000000000 ) ) ;
#25815 = CARTESIAN_POINT ( 'NONE',  ( 24.90937500061451715, 0.000000000000000000, 4.756430356249998326 ) ) ;
#25816 = CARTESIAN_POINT ( 'NONE',  ( 14.35312500061451679, 4.541064518000418104, -2.621784821874998173 ) ) ;
#25817 = CARTESIAN_POINT ( 'NONE',  ( 5.212500000000002132, 2.886751345948126879, 4.999999999999999112 ) ) ;
#25818 = CARTESIAN_POINT ( 'NONE',  ( -1.243387493232115393E-14, 16.15624999877096712, 26.00000000000000000 ) ) ;
#25819 = CARTESIAN_POINT ( 'NONE',  ( 45.00000000000000000, 0.000000000000000000, 0.000000000000000000 ) ) ;
#25820 = CARTESIAN_POINT ( 'NONE',  ( 11.77500000000000036, 6.123233995736764310E-16, -4.999999999999998224 ) ) ;
#25821 = EDGE_CURVE ( 'NONE', #33507, #54715, #30021, .T. ) ;
#25822 = CARTESIAN_POINT ( 'NONE',  ( -1.999999999999997113, 18.38750000122903572, 33.46410161513775705 ) ) ;
#25823 = CARTESIAN_POINT ( 'NONE',  ( 12.11250000122903181, 0.000000000000000000, 4.999999999999998224 ) ) ;
#25824 = CARTESIAN_POINT ( 'NONE',  ( 22.95937500061451431, 4.541064518000418104, -2.621784821874998173 ) ) ;
#25825 = CARTESIAN_POINT ( 'NONE',  ( 16.58437500061451786, 6.421520780324663323E-16, -5.243569643749999010 ) ) ;
#25826 = CARTESIAN_POINT ( 'NONE',  ( 7.143750001229036251, -2.886751345948130876, 4.999999999999996447 ) ) ;
#25827 = VERTEX_POINT ( 'NONE', #24882 ) ;
#25828 = CARTESIAN_POINT ( 'NONE',  ( 17.91562500061451502, 3.027376345333613106, -5.243569643749998122 ) ) ;
#25829 = CARTESIAN_POINT ( 'NONE',  ( 3.065625000614517592, 3.027376345333613106, -5.243569643749998122 ) ) ;
#25830 = CARTESIAN_POINT ( 'NONE',  ( 18.34687500061451715, -3.027376345333610441, -5.243569643749999898 ) ) ;
#25831 = CARTESIAN_POINT ( 'NONE',  ( 28.24687500061451573, -3.027376345333610441, -5.243569643749999898 ) ) ;
#25832 = CARTESIAN_POINT ( 'NONE',  ( 4.565625000614516260, 3.027376345333611329, 5.243569643749999010 ) ) ;
#25833 = CARTESIAN_POINT ( 'NONE',  ( 18.96562500061451573, 3.027376345333611329, 5.243569643749999010 ) ) ;
#25834 = CARTESIAN_POINT ( 'NONE',  ( -4.243569643749999898, 13.01562500061451999, 27.54997392385601529 ) ) ;
#25835 = CARTESIAN_POINT ( 'NONE',  ( 17.21250000122903145, -4.330127018922190985, -2.500000000000001332 ) ) ;
#25836 = CARTESIAN_POINT ( 'NONE',  ( 11.40937500061451892, 0.000000000000000000, 4.756430356249998326 ) ) ;
#25837 = CARTESIAN_POINT ( 'NONE',  ( 8.165625000614518569, 3.027376345333611329, 5.243569643749999010 ) ) ;
#25838 = CARTESIAN_POINT ( 'NONE',  ( 25.97812500061451502, 6.421520780324663323E-16, -5.243569643749999010 ) ) ;
#25839 = CARTESIAN_POINT ( 'NONE',  ( 9.074999999999999289, 6.123233995736764310E-16, -4.999999999999998224 ) ) ;
#25840 = CARTESIAN_POINT ( 'NONE',  ( 24.08437500061451786, -4.541064518000419881, 2.621784821874995952 ) ) ;
#25841 = CARTESIAN_POINT ( 'NONE',  ( 13.82812500061451466, 6.421520780324663323E-16, -5.243569643749999010 ) ) ;
#25842 = CARTESIAN_POINT ( 'NONE',  ( 25.98750000122903003, 4.330127018922191873, 2.499999999999999556 ) ) ;
#25843 = CARTESIAN_POINT ( 'NONE',  ( 23.05312500061451431, 0.000000000000000000, 5.243569643749999010 ) ) ;
#25844 = CARTESIAN_POINT ( 'NONE',  ( 18.90937500061451360, 4.541064518000418104, -2.621784821874998173 ) ) ;
#25845 = CARTESIAN_POINT ( 'NONE',  ( 15.85312500061451857, 0.000000000000000000, 5.243569643749999010 ) ) ;
#25846 = CARTESIAN_POINT ( 'NONE',  ( -4.243569643749999898, 14.00937500061451857, 30.00000000000000000 ) ) ;
#25847 = CARTESIAN_POINT ( 'NONE',  ( 20.95312500061451999, -4.541064518000417216, -2.621784821875001281 ) ) ;
#25848 = CARTESIAN_POINT ( 'NONE',  ( 28.97812500061451502, -4.541064518000419881, 2.621784821874995952 ) ) ;
#25849 = ORIENTED_EDGE ( 'NONE', *, *, #15556, .F. ) ;
#25850 = VERTEX_POINT ( 'NONE', #47427 ) ;
#25851 = CARTESIAN_POINT ( 'NONE',  ( 23.09999999999999787, 4.330127018922192761, -2.499999999999997780 ) ) ;
#25852 = CARTESIAN_POINT ( 'NONE',  ( -3.999999999999999112, 11.00000000000000178, -30.00000000000000000 ) ) ;
#25853 = CARTESIAN_POINT ( 'NONE',  ( 21.56250000122903288, 0.000000000000000000, 4.999999999999998224 ) ) ;
#25854 = CARTESIAN_POINT ( 'NONE',  ( 27.96562500061451928, 3.027376345333611329, 5.243569643749999010 ) ) ;
#25855 = CARTESIAN_POINT ( 'NONE',  ( 8.765625000614518214, -6.054752690667223547, -1.112240025338166033E-15 ) ) ;
#25856 = CARTESIAN_POINT ( 'NONE',  ( 19.08750000122903145, 6.123233995736764310E-16, -4.999999999999998224 ) ) ;
#25857 = CARTESIAN_POINT ( 'NONE',  ( 25.00312500061451715, -4.541064518000417216, -2.621784821875001281 ) ) ;
#25858 = CARTESIAN_POINT ( 'NONE',  ( 22.64999999999999858, 4.330127018922192761, -2.499999999999997780 ) ) ;
#25859 = CARTESIAN_POINT ( 'NONE',  ( 27.85312500061451502, 4.541064518000418104, -2.621784821874998173 ) ) ;
#25860 = CARTESIAN_POINT ( 'NONE',  ( 8.465625000614515727, 3.027376345333613106, -5.243569643749998122 ) ) ;
#25861 = ORIENTED_EDGE ( 'NONE', *, *, #27838, .T. ) ;
#25862 = CARTESIAN_POINT ( 'NONE',  ( 22.60312500061451857, 0.000000000000000000, 5.243569643749999010 ) ) ;
#25863 = CARTESIAN_POINT ( 'NONE',  ( 4.115625000614516082, 3.027376345333611329, 5.243569643749999010 ) ) ;
#25864 = CARTESIAN_POINT ( 'NONE',  ( 12.83437500061451786, -4.119189519843968306, 2.378215178124996054 ) ) ;
#25865 = CARTESIAN_POINT ( 'NONE',  ( 4.228125000614517681, -4.541064518000419881, 2.621784821874995952 ) ) ;
#25866 = CARTESIAN_POINT ( 'NONE',  ( 2.000000000000001332, 13.96250000122903323, -26.53589838486224650 ) ) ;
#25867 = LINE ( 'NONE', #43230, #11408 ) ;
#25868 = CARTESIAN_POINT ( 'NONE',  ( 11.17500000000000071, -4.330127018922194537, 2.499999999999995559 ) ) ;
#25869 = CARTESIAN_POINT ( 'NONE',  ( 11.67187500061451821, 3.027376345333613106, -5.243569643749998122 ) ) ;
#25870 = CARTESIAN_POINT ( 'NONE',  ( 9.412500001229034297, 0.000000000000000000, 4.999999999999998224 ) ) ;
#25871 = CARTESIAN_POINT ( 'NONE',  ( 14.67187500061451821, -6.054752690667223547, -1.112240025338166033E-15 ) ) ;
#25872 = CARTESIAN_POINT ( 'NONE',  ( 15.03749999999999964, 5.773502691896255534, 3.535250795749688894E-16 ) ) ;
#25873 = CARTESIAN_POINT ( 'NONE',  ( 5.746875000614517504, -3.027376345333610441, -5.243569643749999898 ) ) ;
#25874 = CARTESIAN_POINT ( 'NONE',  ( -6.275039685470489619E-15, 18.31250000000000000, 33.99999999999999289 ) ) ;
#25875 = CARTESIAN_POINT ( 'NONE',  ( 4.898587196589411843E-16, 20.00000000000000000, 33.99999999999999289 ) ) ;
#25876 = CARTESIAN_POINT ( 'NONE',  ( 12.27187500061451786, 3.027376345333611329, 5.243569643749999010 ) ) ;
#25877 = CARTESIAN_POINT ( 'NONE',  ( 30.00000000000000000, 0.000000000000000000, 0.000000000000000000 ) ) ;
#25878 = CARTESIAN_POINT ( 'NONE',  ( 21.81562500061451004, -6.054752690667223547, -1.112240025338166033E-15 ) ) ;
#25879 = CARTESIAN_POINT ( 'NONE',  ( -3.000416591977282496E-16, 10.74687500061451928, 25.09994784771203058 ) ) ;
#25880 = CARTESIAN_POINT ( 'NONE',  ( -2.121784821874999949, 19.27812500061459033, 26.32496088578401938 ) ) ;
#25881 = CARTESIAN_POINT ( 'NONE',  ( 26.14687500061451431, 6.054752690667223547, 3.707466751127219781E-16 ) ) ;
#25882 = DIRECTION ( 'NONE',  ( 0.000000000000000000, 0.000000000000000000, 1.000000000000000000 ) ) ;
#25883 = CARTESIAN_POINT ( 'NONE',  ( 5.465625000614517504, 3.027376345333611329, 5.243569643749999010 ) ) ;
#25884 = CARTESIAN_POINT ( 'NONE',  ( 21.72187500061451715, -4.119189519843968306, 2.378215178124996054 ) ) ;
#25885 = CARTESIAN_POINT ( 'NONE',  ( 17.70937500061451431, 0.000000000000000000, 5.243569643749999010 ) ) ;
#25886 = CARTESIAN_POINT ( 'NONE',  ( 7.659375000614513596, 2.746126346562643317, 4.756430356249998326 ) ) ;
#25887 = CARTESIAN_POINT ( 'NONE',  ( 26.66250000122903430, -4.330127018922190985, -2.500000000000001332 ) ) ;
#25888 = CARTESIAN_POINT ( 'NONE',  ( 7.021875000614518747, -6.054752690667223547, -1.112240025338166033E-15 ) ) ;
#25889 = CARTESIAN_POINT ( 'NONE',  ( 16.77187500061451786, 3.027376345333611329, 5.243569643749999010 ) ) ;
#25890 = CARTESIAN_POINT ( 'NONE',  ( 8.625000000000000000, 6.123233995736764310E-16, -4.999999999999998224 ) ) ;
#25891 = CARTESIAN_POINT ( 'NONE',  ( 24.67500000000000071, -4.330127018922194537, 2.499999999999995559 ) ) ;
#25892 = CARTESIAN_POINT ( 'NONE',  ( 2.775000001229033675, -5.773502691896255534, -1.060575238724906372E-15 ) ) ;
#25893 = CARTESIAN_POINT ( 'NONE',  ( 27.00937500061451857, 4.541064518000418104, -2.621784821874998173 ) ) ;
#25894 = CARTESIAN_POINT ( 'NONE',  ( -3.756430356250001434, 13.01562499938548534, 32.16877607737301048 ) ) ;
#25895 = LINE ( 'NONE', #20702, #7952 ) ;
#25896 = CARTESIAN_POINT ( 'NONE',  ( 9.187500000000001776, 5.773502691896255534, 3.535250795749688894E-16 ) ) ;
#25897 = CARTESIAN_POINT ( 'NONE',  ( 8.634375000614515017, -2.746126346562646425, 4.756430356249996549 ) ) ;
#25898 = CARTESIAN_POINT ( 'NONE',  ( 22.15312500061451573, 0.000000000000000000, 5.243569643749999010 ) ) ;
#25899 = CARTESIAN_POINT ( 'NONE',  ( 10.61250000000000071, 2.886751345948126879, 4.999999999999999112 ) ) ;
#25900 = CARTESIAN_POINT ( 'NONE',  ( 3.590625000614518836, 6.054752690667223547, 3.707466751127219781E-16 ) ) ;
#25901 = CARTESIAN_POINT ( 'NONE',  ( 20.06250000000000000, 2.886751345948126879, 4.999999999999999112 ) ) ;
#25902 = EDGE_CURVE ( 'NONE', #39550, #14695, #48441, .T. ) ;
#25903 = CARTESIAN_POINT ( 'NONE',  ( 19.11562500061451431, -6.054752690667223547, -1.112240025338166033E-15 ) ) ;
#25904 = CARTESIAN_POINT ( 'NONE',  ( 23.55000000000000071, 4.330127018922192761, -2.499999999999997780 ) ) ;
#25905 = CARTESIAN_POINT ( 'NONE',  ( 23.17500000122903359, 2.886751345948129099, -4.999999999999998224 ) ) ;
#25906 = CARTESIAN_POINT ( 'NONE',  ( -1.878215178125001827, 19.69062499938548072, 33.25316411605952283 ) ) ;
#25907 = CARTESIAN_POINT ( 'NONE',  ( 3.562500000000000444, -5.773502691896255534, -1.060575238724906372E-15 ) ) ;
#25908 = ORIENTED_EDGE ( 'NONE', *, *, #64257, .T. ) ;
#25909 = CARTESIAN_POINT ( 'NONE',  ( 19.00312500061451715, 0.000000000000000000, 5.243569643749999010 ) ) ;
#25910 = CARTESIAN_POINT ( 'NONE',  ( 23.35312500061451857, 4.541064518000418104, -2.621784821874998173 ) ) ;
#25911 = CARTESIAN_POINT ( 'NONE',  ( 24.72187500061451360, 3.027376345333613106, -5.243569643749998122 ) ) ;
#25912 = CARTESIAN_POINT ( 'NONE',  ( 9.712500000000002132, 2.886751345948126879, 4.999999999999999112 ) ) ;
#25913 = CARTESIAN_POINT ( 'NONE',  ( 12.29062500061451857, -3.027376345333614438, 5.243569643749998122 ) ) ;
#25914 = CARTESIAN_POINT ( 'NONE',  ( 26.12812500061451360, 4.541064518000418104, 2.621784821874999949 ) ) ;
#25915 = CARTESIAN_POINT ( 'NONE',  ( 16.43437500061451573, -4.541064518000419881, 2.621784821874995952 ) ) ;
#25916 = CARTESIAN_POINT ( 'NONE',  ( 9.253125000614517148, -4.541064518000417216, -2.621784821875001281 ) ) ;
#25917 = CARTESIAN_POINT ( 'NONE',  ( 22.94999999999999929, -4.330127018922190985, -2.500000000000001332 ) ) ;
#25918 = CARTESIAN_POINT ( 'NONE',  ( 2.121784821874999061, 11.15937500061451715, 26.32496088578401583 ) ) ;
#25919 = CARTESIAN_POINT ( 'NONE',  ( 24.00000000122902932, -2.886751345948125991, -5.000000000000000000 ) ) ;
#25920 = CARTESIAN_POINT ( 'NONE',  ( 18.53437500061451715, 4.119189519843966529, 2.378215178124999607 ) ) ;
#25921 = CARTESIAN_POINT ( 'NONE',  ( 15.51562500061451644, -6.054752690667223547, -1.112240025338166033E-15 ) ) ;
#25922 = CARTESIAN_POINT ( 'NONE',  ( 7.171875000614517326, 3.027376345333613106, -5.243569643749998122 ) ) ;
#25923 = CARTESIAN_POINT ( 'NONE',  ( 10.47187500061451715, 3.027376345333611329, 5.243569643749999010 ) ) ;
#25924 = ORIENTED_EDGE ( 'NONE', *, *, #23115, .T. ) ;
#25925 = CARTESIAN_POINT ( 'NONE',  ( 29.82187500061451502, 3.027376345333611329, 5.243569643749999010 ) ) ;
#25926 = CARTESIAN_POINT ( 'NONE',  ( 20.80312500061451431, 0.000000000000000000, 5.243569643749999010 ) ) ;
#25927 = CARTESIAN_POINT ( 'NONE',  ( 17.48437500061451999, 6.421520780324663323E-16, -5.243569643749999010 ) ) ;
#25928 = CARTESIAN_POINT ( 'NONE',  ( 22.49062500061451431, 6.054752690667223547, 3.707466751127219781E-16 ) ) ;
#25929 = CARTESIAN_POINT ( 'NONE',  ( 4.000000000000000000, 12.08750000000000036, 32.30940107675849049 ) ) ;
#25930 = CARTESIAN_POINT ( 'NONE',  ( 27.10312500061451502, 0.000000000000000000, 5.243569643749999010 ) ) ;
#25931 = CARTESIAN_POINT ( 'NONE',  ( 7.650000001229034119, -2.886751345948129988, 4.999999999999997335 ) ) ;
#25932 = EDGE_LOOP ( 'NONE', ( #42248, #67012, #67220, #16570 ) ) ;
#25933 = DIRECTION ( 'NONE',  ( -0.000000000000000000, -0.000000000000000000, -1.000000000000000000 ) ) ;
#25934 = CARTESIAN_POINT ( 'NONE',  ( 1.999999999999998668, 18.50000000000000000, -33.46410161513775705 ) ) ;
#25935 = CARTESIAN_POINT ( 'NONE',  ( 25.38750000122903216, 6.123233995736764310E-16, -4.999999999999998224 ) ) ;
#25936 = CARTESIAN_POINT ( 'NONE',  ( 3.756430356250000102, 14.10312499938548392, 30.00000000000000000 ) ) ;
#25937 = CARTESIAN_POINT ( 'NONE',  ( 6.984375000614516438, -4.541064518000419881, 2.621784821874995952 ) ) ;
#25938 = DIRECTION ( 'NONE',  ( 0.000000000000000000, 1.000000000000000000, 0.000000000000000000 ) ) ;
#25939 = CARTESIAN_POINT ( 'NONE',  ( 15.77812500061451573, 4.541064518000418104, 2.621784821874999949 ) ) ;
#25940 = CARTESIAN_POINT ( 'NONE',  ( 9.271875000614516082, -6.054752690667223547, -1.112240025338166033E-15 ) ) ;
#25941 = CARTESIAN_POINT ( 'NONE',  ( 27.93750000122903288, -4.330127018922194537, 2.499999999999995559 ) ) ;
#25942 = CARTESIAN_POINT ( 'NONE',  ( 17.74687500061451928, -3.027376345333614438, 5.243569643749998122 ) ) ;
#25943 = CARTESIAN_POINT ( 'NONE',  ( 5.409375000614516260, 4.541064518000418104, -2.621784821874998173 ) ) ;
#25944 = SHAPE_REPRESENTATION ( 'spindle', ( #23765 ), #1386 ) ;
#25945 = CARTESIAN_POINT ( 'NONE',  ( 5.203125000614518214, -4.541064518000417216, -2.621784821875001281 ) ) ;
#25946 = CARTESIAN_POINT ( 'NONE',  ( 15.32812500061451644, 4.541064518000418104, 2.621784821874999949 ) ) ;
#25947 = ORIENTED_EDGE ( 'NONE', *, *, #33660, .T. ) ;
#25948 = CARTESIAN_POINT ( 'NONE',  ( 11.76562500061451644, 3.027376345333611329, 5.243569643749999010 ) ) ;
#25949 = CARTESIAN_POINT ( 'NONE',  ( 5.550000001229032698, -2.886751345948125991, -5.000000000000000000 ) ) ;
#25950 = CARTESIAN_POINT ( 'NONE',  ( 10.71562500061451928, 3.027376345333613106, -5.243569643749998122 ) ) ;
#25951 = CARTESIAN_POINT ( 'NONE',  ( 22.32187500061451502, -5.492252693125287522, -1.008910452111647106E-15 ) ) ;
#25952 = CARTESIAN_POINT ( 'NONE',  ( 10.31250000000000355, -5.773502691896255534, -1.060575238724906372E-15 ) ) ;
#25953 = CARTESIAN_POINT ( 'NONE',  ( 3.337500001229034563, 6.123233995736764310E-16, -4.999999999999998224 ) ) ;
#25954 = CARTESIAN_POINT ( 'NONE',  ( 17.62500000000000000, 6.123233995736764310E-16, -4.999999999999998224 ) ) ;
#25955 = CARTESIAN_POINT ( 'NONE',  ( 17.70937500061451431, 0.000000000000000000, 5.243569643749999010 ) ) ;
#25956 = CARTESIAN_POINT ( 'NONE',  ( 15.18750000122903465, 4.330127018922191873, 2.499999999999999556 ) ) ;
#25957 = CARTESIAN_POINT ( 'NONE',  ( 21.33749999999999858, 5.773502691896255534, 3.535250795749688894E-16 ) ) ;
#25958 = CARTESIAN_POINT ( 'NONE',  ( -3.000416591977282496E-16, 15.64062500061451644, -34.90005215228797653 ) ) ;
#25959 = CARTESIAN_POINT ( 'NONE',  ( 9.074999999999999289, 6.123233995736764310E-16, -4.999999999999998224 ) ) ;
#25960 = CARTESIAN_POINT ( 'NONE',  ( 2.775000001229034119, -5.773502691896255534, -1.060575238724906372E-15 ) ) ;
#25961 = CARTESIAN_POINT ( 'NONE',  ( 28.90312500061451217, 0.000000000000000000, 5.243569643749999010 ) ) ;
#25962 = CARTESIAN_POINT ( 'NONE',  ( 12.01875000122903003, 2.886751345948182834, 4.999999999999902300 ) ) ;
#25963 = CYLINDRICAL_SURFACE ( 'NONE', #10146, 4.999999999999998224 ) ;
#25964 = CARTESIAN_POINT ( 'NONE',  ( 16.39687500061451786, -3.027376345333614438, 5.243569643749998122 ) ) ;
#25965 = CARTESIAN_POINT ( 'NONE',  ( 28.80000000000000071, -4.330127018922190985, -2.500000000000001332 ) ) ;
#25966 = CARTESIAN_POINT ( 'NONE',  ( 11.09062500061451573, -3.027376345333610441, -5.243569643749999898 ) ) ;
#25967 = CARTESIAN_POINT ( 'NONE',  ( 7.331250001229031810, 6.123233995736764310E-16, -4.999999999999998224 ) ) ;
#25968 = CARTESIAN_POINT ( 'NONE',  ( 24.98437500061451644, -4.541064518000419881, 2.621784821874995952 ) ) ;
#25969 = CARTESIAN_POINT ( 'NONE',  ( 15.53437500061451537, -2.746126346562641984, -4.756430356249999214 ) ) ;
#25970 = CARTESIAN_POINT ( 'NONE',  ( 7.528125000614515727, 6.421520780324663323E-16, -5.243569643749999010 ) ) ;
#25971 = CARTESIAN_POINT ( 'NONE',  ( 12.57187500061451857, 3.027376345333613106, -5.243569643749998122 ) ) ;
#25972 = ORIENTED_EDGE ( 'NONE', *, *, #24990, .T. ) ;
#25973 = CARTESIAN_POINT ( 'NONE',  ( 23.82187500061451502, 3.027376345333613106, -5.243569643749998122 ) ) ;
#25974 = CARTESIAN_POINT ( 'NONE',  ( 28.19062500061451715, -3.027376345333610441, -5.243569643749999898 ) ) ;
#25975 = EDGE_CURVE ( 'NONE', #60301, #38096, #20142, .T. ) ;
#25976 = CARTESIAN_POINT ( 'NONE',  ( 24.63749999999999929, -2.886751345948163738, 4.999999999999939604 ) ) ;
#25977 =( BOUNDED_CURVE ( )  B_SPLINE_CURVE ( 2, ( #69434, #2552, #64231, #1476, #23983, #29536, #35076 ),
 .UNSPECIFIED., .F., .F. ) 
 B_SPLINE_CURVE_WITH_KNOTS ( ( 3, 2, 2, 3 ),
 ( 0.6416666666666668295, 0.6444444444444445974, 0.6472222222222223653, 0.6500000000000001332 ),
 .UNSPECIFIED. ) 
 CURVE ( )  GEOMETRIC_REPRESENTATION_ITEM ( )  RATIONAL_B_SPLINE_CURVE ( ( 0.9999999999999946709, 0.8660254037844440367, 1.000000000000000000, 0.8660254037844387076, 1.000000000000000000, 0.8660254037844333785, 1.000000000000005329 ) ) 
 REPRESENTATION_ITEM ( '' )  );
#25978 = CARTESIAN_POINT ( 'NONE',  ( 7.537500000000002309, -2.886751345948129988, 4.999999999999997335 ) ) ;
#25979 = CARTESIAN_POINT ( 'NONE',  ( 17.73750000122903359, 6.123233995736764310E-16, -4.999999999999998224 ) ) ;
#25980 = DIRECTION ( 'NONE',  ( -1.000000000000000000, -0.000000000000000000, -0.000000000000000000 ) ) ;
#25981 = CARTESIAN_POINT ( 'NONE',  ( 8.184375000614515727, -2.746126346562646425, 4.756430356249996549 ) ) ;
#25982 = ORIENTED_EDGE ( 'NONE', *, *, #65786, .T. ) ;
#25983 = CARTESIAN_POINT ( 'NONE',  ( 14.92500000000000071, 6.123233995736764310E-16, -4.999999999999998224 ) ) ;
#25984 = CARTESIAN_POINT ( 'NONE',  ( 18.26249999999999929, 2.886751345948126879, 4.999999999999999112 ) ) ;
#25985 = CARTESIAN_POINT ( 'NONE',  ( 13.56562500061451892, 3.027376345333611329, 5.243569643749999010 ) ) ;
#25986 = ORIENTED_EDGE ( 'NONE', *, *, #26717, .T. ) ;
#25987 = CARTESIAN_POINT ( 'NONE',  ( 3.722978149461063424, -3.926822905430812582, -3.198543215468592216 ) ) ;
#25988 = CARTESIAN_POINT ( 'NONE',  ( -2.121784821874996840, 16.33437500061451786, -26.32496088578401583 ) ) ;
#25989 = CARTESIAN_POINT ( 'NONE',  ( 4.040625000614517681, 6.054752690667223547, 3.707466751127219781E-16 ) ) ;
#25990 = CARTESIAN_POINT ( 'NONE',  ( -2.000000000000001776, 14.15000000000000036, 33.46410161513775705 ) ) ;
#25991 = CARTESIAN_POINT ( 'NONE',  ( 9.750000000000001776, 0.000000000000000000, 4.999999999999998224 ) ) ;
#25992 = CARTESIAN_POINT ( 'NONE',  ( 28.77187500061451431, 4.119189519843966529, 2.378215178124999607 ) ) ;
#25993 = ORIENTED_EDGE ( 'NONE', *, *, #1055, .T. ) ;
#25994 = CARTESIAN_POINT ( 'NONE',  ( 9.001249775931846008E-16, 14.51562500061451466, 34.90005215228797653 ) ) ;
#25995 = CARTESIAN_POINT ( 'NONE',  ( 27.17812500061451786, -4.541064518000419881, 2.621784821874995952 ) ) ;
#25996 = CARTESIAN_POINT ( 'NONE',  ( 9.037499999999999645, -2.886751345948125991, -5.000000000000000000 ) ) ;
#25997 = CARTESIAN_POINT ( 'NONE',  ( 0.6522972858965978560, 20.64114861271052348, 33.69936173848522998 ) ) ;
#25998 = CARTESIAN_POINT ( 'NONE',  ( 23.29687500061451644, -3.027376345333610441, -5.243569643749999898 ) ) ;
#25999 = CARTESIAN_POINT ( 'NONE',  ( 19.71562500061451928, 3.027376345333613106, -5.243569643749998122 ) ) ;
#26000 = CARTESIAN_POINT ( 'NONE',  ( -3.000416591977282496E-16, 14.74062500061459424, -34.90005215228797653 ) ) ;
#26001 = CARTESIAN_POINT ( 'NONE',  ( 24.37500000122903288, -5.773502691896255534, -1.060575238724906372E-15 ) ) ;
#26002 = CARTESIAN_POINT ( 'NONE',  ( 3.740625000614516527, -3.027376345333614438, 5.243569643749998122 ) ) ;
#26003 = CARTESIAN_POINT ( 'NONE',  ( 25.99687500061451928, -2.746126346562641984, -4.756430356249999214 ) ) ;
#26004 = CARTESIAN_POINT ( 'NONE',  ( 21.40312500061451573, -4.541064518000417216, -2.621784821875001281 ) ) ;
#26005 = CARTESIAN_POINT ( 'NONE',  ( 11.03437500061451715, -4.119189519843968306, 2.378215178124996054 ) ) ;
#26006 = CARTESIAN_POINT ( 'NONE',  ( 3.756430356249998770, 15.75312499938548427, 32.16877607737302469 ) ) ;
#26007 = CARTESIAN_POINT ( 'NONE',  ( 17.85937500061451999, -4.541064518000417216, -2.621784821875001281 ) ) ;
#26008 = CARTESIAN_POINT ( 'NONE',  ( 15.72187500061451892, 3.027376345333613106, -5.243569643749998122 ) ) ;
#26009 = CARTESIAN_POINT ( 'NONE',  ( 25.39687500061451431, -3.027376345333614438, 5.243569643749998122 ) ) ;
#26010 = CARTESIAN_POINT ( 'NONE',  ( -4.243569643749998122, 15.39687500061451786, 32.45002607614398471 ) ) ;
#26011 = CARTESIAN_POINT ( 'NONE',  ( 4.828125000614518214, 6.421520780324663323E-16, -5.243569643749999010 ) ) ;
#26012 = CARTESIAN_POINT ( 'NONE',  ( 27.85312500061451502, 4.541064518000418104, -2.621784821874998173 ) ) ;
#26013 =( BOUNDED_CURVE ( )  B_SPLINE_CURVE ( 2, ( #68553, #33836, #51196, #28301, #34553, #51919, #57081 ),
 .UNSPECIFIED., .F., .F. ) 
 B_SPLINE_CURVE_WITH_KNOTS ( ( 3, 2, 2, 3 ),
 ( 0.9431886200030490386, 0.9444444444444444198, 0.9472222222222221877, 0.9483504900823832573 ),
 .UNSPECIFIED. ) 
 CURVE ( )  GEOMETRIC_REPRESENTATION_ITEM ( )  RATIONAL_B_SPLINE_CURVE ( ( 0.9336275693722517754, 0.9394305139167113960, 1.000000000000000000, 0.8660254037844387076, 1.000000000000000000, 0.9455826768442929797, 0.9353714217504458528 ) ) 
 REPRESENTATION_ITEM ( '' )  );
#26014 = CARTESIAN_POINT ( 'NONE',  ( 28.22812500061451502, 6.421520780324663323E-16, -5.243569643749999010 ) ) ;
#26015 = CARTESIAN_POINT ( 'NONE',  ( 1.999999999999998668, 19.84999999999999787, 26.53589838486224650 ) ) ;
#26016 = CARTESIAN_POINT ( 'NONE',  ( 6.384375000614516793, 4.541064518000418104, 2.621784821874999949 ) ) ;
#26017 = DIRECTION ( 'NONE',  ( 1.000000000000000000, 0.000000000000000000, 0.000000000000000000 ) ) ;
#26018 = CARTESIAN_POINT ( 'NONE',  ( 13.20000000122903394, -2.886751345948125991, -5.000000000000000000 ) ) ;
#26019 = CARTESIAN_POINT ( 'NONE',  ( 9.712500001229033231, 4.330127018922192761, -2.499999999999997780 ) ) ;
#26020 = CARTESIAN_POINT ( 'NONE',  ( 6.028125000614517504, -4.541064518000419881, 2.621784821874995952 ) ) ;
#26021 = CARTESIAN_POINT ( 'NONE',  ( -2.000000000000001776, 16.34374999877096712, 33.46410161513775705 ) ) ;
#26022 = CARTESIAN_POINT ( 'NONE',  ( 19.96875000122903288, 2.886751345948129099, -4.999999999999998224 ) ) ;
#26023 = CARTESIAN_POINT ( 'NONE',  ( 13.13437500061451857, 4.541064518000418104, 2.621784821874999949 ) ) ;
#26024 = CARTESIAN_POINT ( 'NONE',  ( 0.000000000000000000, 20.00000000000000000, -30.00000000000000000 ) ) ;
#26025 = ORIENTED_EDGE ( 'NONE', *, *, #65868, .T. ) ;
#26026 = CARTESIAN_POINT ( 'NONE',  ( 23.35312500061451857, 4.541064518000418104, -2.621784821874998173 ) ) ;
#26027 = CARTESIAN_POINT ( 'NONE',  ( 7.153125000614518392, 4.541064518000418104, -2.621784821874998173 ) ) ;
#26028 = CARTESIAN_POINT ( 'NONE',  ( 23.74687500061451573, -3.027376345333610441, -5.243569643749999898 ) ) ;
#26029 = CARTESIAN_POINT ( 'NONE',  ( 7.940625000614518036, -3.027376345333610441, -5.243569643749999898 ) ) ;
#26030 = CARTESIAN_POINT ( 'NONE',  ( 34.99999999999999289, 9.426999614876460059E-14, 7.499999999999999112 ) ) ;
#26031 = CARTESIAN_POINT ( 'NONE',  ( 7.687500001229033764, -4.330127018922194537, 2.499999999999995559 ) ) ;
#26032 = CARTESIAN_POINT ( 'NONE',  ( 22.45312500061451644, 4.541064518000418104, -2.621784821874998173 ) ) ;
#26033 = CARTESIAN_POINT ( 'NONE',  ( 9.001249775931846008E-16, 10.01562500061451644, -25.09994784771203058 ) ) ;
#26034 = CARTESIAN_POINT ( 'NONE',  ( 10.12500000122903465, 2.886751345948129099, -4.999999999999998224 ) ) ;
#26035 =( BOUNDED_CURVE ( )  B_SPLINE_CURVE ( 2, ( #41919, #46744, #47102, #64444, #13836, #20838, #15657, #71462, #64810 ),
 .UNSPECIFIED., .F., .F. ) 
 B_SPLINE_CURVE_WITH_KNOTS ( ( 3, 2, 2, 2, 3 ),
 ( 0.1847826086956521896, 0.1884057971014492794, 0.1956521739130434867, 0.2028985507246376940, 0.2065217391304347838 ),
 .UNSPECIFIED. ) 
 CURVE ( )  GEOMETRIC_REPRESENTATION_ITEM ( )  RATIONAL_B_SPLINE_CURVE ( ( 0.9330127018922194093, 0.9330127018922196314, 1.000000000000000000, 0.8660254037844387076, 1.000000000000000000, 0.8660254037844387076, 1.000000000000000000, 0.9330127018922194093, 0.9330127018922194093 ) ) 
 REPRESENTATION_ITEM ( '' )  );
#26036 = CARTESIAN_POINT ( 'NONE',  ( 19.60312500061451502, -4.541064518000417216, -2.621784821875001281 ) ) ;
#26037 = CARTESIAN_POINT ( 'NONE',  ( 17.31562500061451715, -6.054752690667223547, -1.112240025338166033E-15 ) ) ;
#26038 = CARTESIAN_POINT ( 'NONE',  ( 29.55937500061451573, -4.119189519843965641, -2.378215178125001383 ) ) ;
#26039 = CARTESIAN_POINT ( 'NONE',  ( 19.08750000000000213, 5.773502691896255534, 3.535250795749688894E-16 ) ) ;
#26040 = CARTESIAN_POINT ( 'NONE',  ( 10.87500000122903288, -5.773502691896255534, -1.060575238724906372E-15 ) ) ;
#26041 = CARTESIAN_POINT ( 'NONE',  ( 7.490625000614516082, -3.027376345333610441, -5.243569643749999898 ) ) ;
#26042 = CARTESIAN_POINT ( 'NONE',  ( 12.29062500061451857, -3.027376345333614438, 5.243569643749998122 ) ) ;
#26043 = EDGE_CURVE ( 'NONE', #45851, #14969, #73032, .T. ) ;
#26044 = CARTESIAN_POINT ( 'NONE',  ( 24.18750000122903288, 4.330127018922191873, 2.499999999999999556 ) ) ;
#26045 = CARTESIAN_POINT ( 'NONE',  ( 22.39687500061451075, -3.027376345333610441, -5.243569643749999898 ) ) ;
#26046 = CARTESIAN_POINT ( 'NONE',  ( 21.99375000122903145, -2.886751345948102898, 5.000000000000044409 ) ) ;
#26047 = CARTESIAN_POINT ( 'NONE',  ( 4.500000001229034652, -2.886751345948129988, 4.999999999999997335 ) ) ;
#26048 = CARTESIAN_POINT ( 'NONE',  ( 6.084375000614518747, -4.541064518000419881, 2.621784821874995952 ) ) ;
#26049 = CARTESIAN_POINT ( 'NONE',  ( 22.95937500061451431, 4.541064518000418104, -2.621784821874998173 ) ) ;
#26050 = EDGE_CURVE ( 'NONE', #68472, #66931, #16270, .T. ) ;
#26051 = CARTESIAN_POINT ( 'NONE',  ( -1.071796769724490783, 12.81740381056766864, 34.00000000000000711 ) ) ;
#26052 = CARTESIAN_POINT ( 'NONE',  ( 17.84062500061451573, -3.027376345333610441, -5.243569643749999898 ) ) ;
#26053 = CARTESIAN_POINT ( 'NONE',  ( 23.33437500061451786, 6.421520780324663323E-16, -5.243569643749999010 ) ) ;
#26054 = CARTESIAN_POINT ( 'NONE',  ( -3.756430356250000990, 19.76562499938548356, 32.16877607737301048 ) ) ;
#26055 = CARTESIAN_POINT ( 'NONE',  ( 3.459375000614519635, -4.541064518000417216, -2.621784821875001281 ) ) ;
#26056 = CARTESIAN_POINT ( 'NONE',  ( -3.999999999999999112, 13.36250000122903359, -30.00000000000000000 ) ) ;
#26057 = CARTESIAN_POINT ( 'NONE',  ( 5.184375000614516615, -4.541064518000419881, 2.621784821874995952 ) ) ;
#26058 = CARTESIAN_POINT ( 'NONE',  ( 15.89062500061451289, -3.027376345333614438, 5.243569643749998122 ) ) ;
#26059 = CARTESIAN_POINT ( 'NONE',  ( 13.54687500061451999, 6.054752690667223547, 3.707466751127219781E-16 ) ) ;
#26060 = ORIENTED_EDGE ( 'NONE', *, *, #20794, .T. ) ;
#26061 = CARTESIAN_POINT ( 'NONE',  ( 17.00625000122903074, 0.000000000000000000, 4.999999999999998224 ) ) ;
#26062 = CARTESIAN_POINT ( 'NONE',  ( 26.24062500061451431, -3.027376345333614438, 5.243569643749998122 ) ) ;
#26063 = CARTESIAN_POINT ( 'NONE',  ( 30.00000000000000000, 0.000000000000000000, 4.999999999999998224 ) ) ;
#26064 = CARTESIAN_POINT ( 'NONE',  ( 3.965171583692859603, 3.045884815923804556, 3.965171583692790325 ) ) ;
#26065 = CARTESIAN_POINT ( 'NONE',  ( 13.53749999999999964, -2.886751345948125991, -5.000000000000000000 ) ) ;
#26066 = CARTESIAN_POINT ( 'NONE',  ( 24.97500000122903430, 2.886751345948129099, -4.999999999999998224 ) ) ;
#26067 = CARTESIAN_POINT ( 'NONE',  ( 18.81562500061452070, 3.027376345333613106, -5.243569643749998122 ) ) ;
#26068 = ORIENTED_EDGE ( 'NONE', *, *, #59373, .F. ) ;
#26069 = CARTESIAN_POINT ( 'NONE',  ( 22.68750000000000000, 5.773502691896255534, 3.535250795749688894E-16 ) ) ;
#26070 = CARTESIAN_POINT ( 'NONE',  ( 23.52187500061451786, 3.027376345333611329, 5.243569643749999010 ) ) ;
#26071 = ORIENTED_EDGE ( 'NONE', *, *, #57999, .T. ) ;
#26072 = CARTESIAN_POINT ( 'NONE',  ( 18.18750000122903288, 6.123233995736764310E-16, -4.999999999999998224 ) ) ;
#26073 = CARTESIAN_POINT ( 'NONE',  ( 10.37812500061451715, 4.541064518000418104, 2.621784821874999949 ) ) ;
#26074 = CARTESIAN_POINT ( 'NONE',  ( 3.103125000614517237, 4.541064518000418104, -2.621784821874998173 ) ) ;
#26075 = CARTESIAN_POINT ( 'NONE',  ( 14.33437500061451431, 5.492252693125287522, 3.363034840372157021E-16 ) ) ;
#26076 = CARTESIAN_POINT ( 'NONE',  ( 27.96562500061451928, 3.027376345333611329, 5.243569643749999010 ) ) ;
#26077 = CARTESIAN_POINT ( 'NONE',  ( 19.16250000000000142, 2.886751345948126879, 4.999999999999999112 ) ) ;
#26078 = CARTESIAN_POINT ( 'NONE',  ( 26.96249999999999858, -5.773502691896255534, -1.060575238724906372E-15 ) ) ;
#26079 = CARTESIAN_POINT ( 'NONE',  ( 3.262500001229035718, -4.330127018922190985, -2.500000000000001332 ) ) ;
#26080 = CARTESIAN_POINT ( 'NONE',  ( 7.659375000614518036, 4.541064518000418104, -2.621784821874998173 ) ) ;
#26081 = CARTESIAN_POINT ( 'NONE',  ( 17.85937500061451999, -4.541064518000417216, -2.621784821875001281 ) ) ;
#26082 = CARTESIAN_POINT ( 'NONE',  ( 3.999999999999999112, 11.33750000122903501, 30.00000000000000000 ) ) ;
#26083 = ORIENTED_EDGE ( 'NONE', *, *, #72649, .F. ) ;
#26084 = CARTESIAN_POINT ( 'NONE',  ( 25.82812500061451644, -4.541064518000419881, 2.621784821874995952 ) ) ;
#26085 = CARTESIAN_POINT ( 'NONE',  ( 27.08437500061451786, 4.541064518000418104, 2.621784821874999949 ) ) ;
#26087 = ADVANCED_FACE ( 'NONE', ( #44376 ), #54713, .T. ) ;
#26086 = CARTESIAN_POINT ( 'NONE',  ( 4.898587196589412829E-16, 27.50000000000000000, 34.00000000000000000 ) ) ;
#26088 = CARTESIAN_POINT ( 'NONE',  ( 13.50000000000000178, -4.330127018922190985, -2.500000000000001332 ) ) ;
#26089 = CARTESIAN_POINT ( 'NONE',  ( 11.99062500061451608, -3.027376345333610441, -5.243569643749999898 ) ) ;
#26090 = CARTESIAN_POINT ( 'NONE',  ( 16.31249999999999645, 2.886751345948018077, -5.000000000000190070 ) ) ;
#26091 = CARTESIAN_POINT ( 'NONE',  ( -1.071796769724490339, 17.97634618820330132, 26.00000000000000000 ) ) ;
#26092 = CARTESIAN_POINT ( 'NONE',  ( 28.75312500061451715, 4.541064518000418104, -2.621784821874998173 ) ) ;
#26093 = CARTESIAN_POINT ( 'NONE',  ( 18.37500000122903288, 2.886751345948126879, 4.999999999999999112 ) ) ;
#26094 = CARTESIAN_POINT ( 'NONE',  ( 45.00000000000000000, 0.000000000000000000, 4.999999999999998224 ) ) ;
#26095 = CARTESIAN_POINT ( 'NONE',  ( 17.63437500061451502, 4.119189519843966529, 2.378215178124999607 ) ) ;
#26096 = CARTESIAN_POINT ( 'NONE',  ( 6.253125000614517148, 4.541064518000418104, -2.621784821874998173 ) ) ;
#26097 = CARTESIAN_POINT ( 'NONE',  ( 21.57187500061451502, 3.027376345333613106, -5.243569643749998122 ) ) ;
#26098 = CARTESIAN_POINT ( 'NONE',  ( -4.243569643749999898, 17.15937500061451715, 30.00000000000000000 ) ) ;
#26099 = CARTESIAN_POINT ( 'NONE',  ( 23.74687500061451573, -3.027376345333610441, -5.243569643749999898 ) ) ;
#26100 = CARTESIAN_POINT ( 'NONE',  ( 4.987500000000002487, -2.886751345948125991, -5.000000000000000000 ) ) ;
#26101 = CARTESIAN_POINT ( 'NONE',  ( 3.999999999999999112, 10.88750000122903394, 30.00000000000000000 ) ) ;
#26102 = CARTESIAN_POINT ( 'NONE',  ( 13.11562500061451786, 3.027376345333611329, 5.243569643749999010 ) ) ;
#26103 = CARTESIAN_POINT ( 'NONE',  ( 3.750000001229034652, -2.886751345948125991, -5.000000000000000000 ) ) ;
#26104 = CARTESIAN_POINT ( 'NONE',  ( 9.309375000614517504, -4.541064518000417216, -2.621784821875001281 ) ) ;
#26105 = CARTESIAN_POINT ( 'NONE',  ( 3.999999999999999112, 14.93750000122903288, 30.00000000000000000 ) ) ;
#26106 = CARTESIAN_POINT ( 'NONE',  ( 10.67812500061451608, 6.421520780324663323E-16, -5.243569643749999010 ) ) ;
#26107 = CARTESIAN_POINT ( 'NONE',  ( 14.03437500061451715, 4.541064518000418104, 2.621784821874999949 ) ) ;
#26108 = CARTESIAN_POINT ( 'NONE',  ( -4.000000000000000888, 19.06250000000000000, 32.30940107675850470 ) ) ;
#26109 = CARTESIAN_POINT ( 'NONE',  ( 21.15000000122903145, -2.886751345948129988, 4.999999999999997335 ) ) ;
#26110 = CARTESIAN_POINT ( 'NONE',  ( 11.55937500061451928, -4.541064518000417216, -2.621784821875001281 ) ) ;
#26111 = CARTESIAN_POINT ( 'NONE',  ( 12.77812500061451750, -4.541064518000419881, 2.621784821874995952 ) ) ;
#26112 = CARTESIAN_POINT ( 'NONE',  ( 28.29375000122902861, -2.886751345948129988, 4.999999999999997335 ) ) ;
#26113 = CARTESIAN_POINT ( 'NONE',  ( 21.87187500061451573, -6.054752690667223547, -1.112240025338166033E-15 ) ) ;
#26114 = FACE_OUTER_BOUND ( 'NONE', #9439, .T. ) ;
#26115 = DIRECTION ( 'NONE',  ( -0.9848086006944722914, -4.896307315423231436E-06, 0.1736433700842670569 ) ) ;
#26116 = FACE_OUTER_BOUND ( 'NONE', #12074, .T. ) ;
#26117 = CARTESIAN_POINT ( 'NONE',  ( 4.243569643749999898, 14.19687500061452035, -27.54997392385601529 ) ) ;
#26118 = CARTESIAN_POINT ( 'NONE',  ( 16.31250000122903288, -4.330127018922190985, -2.500000000000001332 ) ) ;
#26119 = CARTESIAN_POINT ( 'NONE',  ( 10.35937500061451644, 4.541064518000418104, -2.621784821874998173 ) ) ;
#26120 = CARTESIAN_POINT ( 'NONE',  ( -3.000416591977282496E-16, 18.34062500061451928, -34.90005215228797653 ) ) ;
#26121 = CARTESIAN_POINT ( 'NONE',  ( 17.17500000122903359, -5.773502691896255534, -1.060575238724906372E-15 ) ) ;
#26122 = CARTESIAN_POINT ( 'NONE',  ( 13.22812500061451502, -4.541064518000419881, 2.621784821874995952 ) ) ;
#26123 = ORIENTED_EDGE ( 'NONE', *, *, #35290, .F. ) ;
#26124 = CARTESIAN_POINT ( 'NONE',  ( 16.46249999999999503, 2.886751345948126879, 4.999999999999999112 ) ) ;
#26125 = CARTESIAN_POINT ( 'NONE',  ( 5.025000001229035895, -5.773502691896255534, -1.060575238724906372E-15 ) ) ;
#26126 = CARTESIAN_POINT ( 'NONE',  ( 9.121875000614517504, 3.027376345333611329, 5.243569643749999010 ) ) ;
#26127 = CARTESIAN_POINT ( 'NONE',  ( 4.342984975361706468, -2.477595912125914790, -4.621313785610477787 ) ) ;
#26128 = CARTESIAN_POINT ( 'NONE',  ( 11.13750000122903216, 4.330127018922191873, 2.499999999999999556 ) ) ;
#26129 = CARTESIAN_POINT ( 'NONE',  ( 18.33750000122903501, 4.330127018922191873, 2.499999999999999556 ) ) ;
#26130 = CARTESIAN_POINT ( 'NONE',  ( 16.64062500061451289, 6.054752690667223547, 3.707466751127219781E-16 ) ) ;
#26131 = CARTESIAN_POINT ( 'NONE',  ( 20.65312500061451573, 4.541064518000418104, -2.621784821874998173 ) ) ;
#26132 = CARTESIAN_POINT ( 'NONE',  ( 28.01250000122903216, -4.330127018922190985, -2.500000000000001332 ) ) ;
#26133 = CARTESIAN_POINT ( 'NONE',  ( 3.853125000614517681, -4.541064518000417216, -2.621784821875001281 ) ) ;
#26134 = CARTESIAN_POINT ( 'NONE',  ( 25.23749999999999716, -2.886751345948125991, -5.000000000000000000 ) ) ;
#26135 = CARTESIAN_POINT ( 'NONE',  ( 3.756430356250000102, 12.64062499938548356, 30.00000000000000000 ) ) ;
#26136 = CARTESIAN_POINT ( 'NONE',  ( 28.64999999999999858, 0.000000000000000000, 4.999999999999998224 ) ) ;
#26137 = CARTESIAN_POINT ( 'NONE',  ( 29.33437500061451431, 4.541064518000418104, 2.621784821874999949 ) ) ;
#26138 = CARTESIAN_POINT ( 'NONE',  ( 11.73750000000000071, -2.886751345948126435, -5.000000000000000000 ) ) ;
#26139 = CARTESIAN_POINT ( 'NONE',  ( 11.96250000122903501, 4.330127018922192761, -2.499999999999997780 ) ) ;
#26140 = CARTESIAN_POINT ( 'NONE',  ( 29.55937500061451573, -4.541064518000417216, -2.621784821875001281 ) ) ;
#26141 = ADVANCED_FACE ( 'NONE', ( #32908 ), #4482, .T. ) ;
#26142 = CARTESIAN_POINT ( 'NONE',  ( 65.00000000000000000, -3.142333204958820020E-14, -9.000000000000000000 ) ) ;
#26143 = CARTESIAN_POINT ( 'NONE',  ( 7.959375000614516971, -4.541064518000417216, -2.621784821875001281 ) ) ;
#26144 = CARTESIAN_POINT ( 'NONE',  ( 24.96562500061451573, -6.054752690667223547, -1.112240025338166033E-15 ) ) ;
#26145 = CARTESIAN_POINT ( 'NONE',  ( 9.168750001229033941, 2.886751345948129099, -4.999999999999997335 ) ) ;
#26146 = CARTESIAN_POINT ( 'NONE',  ( -2.152738742430647445, 9.767338418468105132, -24.39599078399185217 ) ) ;
#26147 = CARTESIAN_POINT ( 'NONE',  ( 3.723272892789626365, -3.337319327924350265, 3.976188005925537450 ) ) ;
#26148 = CARTESIAN_POINT ( 'NONE',  ( 4.359375000614517326, -4.541064518000417216, -2.621784821875001281 ) ) ;
#26149 = CARTESIAN_POINT ( 'NONE',  ( 8.109375000614518214, 4.541064518000418104, -2.621784821874998173 ) ) ;
#26150 = CARTESIAN_POINT ( 'NONE',  ( 5.325000000000000178, -4.330127018922194537, 2.499999999999995559 ) ) ;
#26151 = CARTESIAN_POINT ( 'NONE',  ( 4.243569643749999898, 11.89062500061459460, 32.45002607614398471 ) ) ;
#26152 = CARTESIAN_POINT ( 'NONE',  ( 20.69999999999999929, -4.330127018922190985, -2.500000000000001332 ) ) ;
#26153 = AXIS2_PLACEMENT_3D ( 'NONE', #55199, #66644, #38569 ) ;
#26154 = CARTESIAN_POINT ( 'NONE',  ( 29.32499999999999929, 6.123233995736764310E-16, -4.999999999999998224 ) ) ;
#26155 =( BOUNDED_CURVE ( )  B_SPLINE_CURVE ( 2, ( #30955, #15055, #26890, #60114, #49416, #59379, #9157 ),
 .UNSPECIFIED., .F., .F. ) 
 B_SPLINE_CURVE_WITH_KNOTS ( ( 3, 2, 2, 3 ),
 ( 0.3300000000000000711, 0.3333333333333333703, 0.3366666666666667251, 0.3400000000000000799 ),
 .UNSPECIFIED. ) 
 CURVE ( )  GEOMETRIC_REPRESENTATION_ITEM ( )  RATIONAL_B_SPLINE_CURVE ( ( 0.9999999999999977796, 0.8660254037844409281, 1.000000000000000000, 0.8660254037844387076, 1.000000000000000000, 0.8660254037844364872, 1.000000000000002220 ) ) 
 REPRESENTATION_ITEM ( '' )  );
#26156 = CARTESIAN_POINT ( 'NONE',  ( 4.050000000000001599, -4.330127018922190985, -2.500000000000001332 ) ) ;
#26157 = CARTESIAN_POINT ( 'NONE',  ( 11.93437500061451750, -2.746126346562642428, -4.756430356249999214 ) ) ;
#26158 = ORIENTED_EDGE ( 'NONE', *, *, #40501, .F. ) ;
#26159 = CARTESIAN_POINT ( 'NONE',  ( 21.25312500061451715, 0.000000000000000000, 5.243569643749999010 ) ) ;
#26160 = CARTESIAN_POINT ( 'NONE',  ( 9.665625000614515017, -6.054752690667223547, -1.112240025338166033E-15 ) ) ;
#26161 = CARTESIAN_POINT ( 'NONE',  ( 24.53437500061451715, -2.746126346562642428, -4.756430356249999214 ) ) ;
#26162 = CARTESIAN_POINT ( 'NONE',  ( 6.421875000614519102, 3.027376345333611329, 5.243569643749999010 ) ) ;
#26163 = CARTESIAN_POINT ( 'NONE',  ( 24.52499999999999858, 4.330127018922191873, 2.499999999999999556 ) ) ;
#26164 = CARTESIAN_POINT ( 'NONE',  ( 20.73750000122903359, -4.330127018922194537, 2.499999999999995559 ) ) ;
#26165 = CARTESIAN_POINT ( 'NONE',  ( 27.92812500061451431, 4.541064518000418104, 2.621784821874999949 ) ) ;
#26166 = CARTESIAN_POINT ( 'NONE',  ( 9.946875000614516793, 6.054752690667223547, 3.707466751127219781E-16 ) ) ;
#26167 = CARTESIAN_POINT ( 'NONE',  ( 13.28437500061451715, -4.541064518000419881, 2.621784821874995952 ) ) ;
#26168 = CARTESIAN_POINT ( 'NONE',  ( 24.98437500061451644, -4.541064518000419881, 2.621784821874995952 ) ) ;
#26169 = CARTESIAN_POINT ( 'NONE',  ( 3.999999999999999112, 18.08750000122903501, -30.00000000000000000 ) ) ;
#26170 = CARTESIAN_POINT ( 'NONE',  ( 12.22499999999999964, 6.123233995736764310E-16, -4.999999999999998224 ) ) ;
#26171 = CARTESIAN_POINT ( 'NONE',  ( 18.68437500061451928, -4.541064518000419881, 2.621784821874995952 ) ) ;
#26172 = CARTESIAN_POINT ( 'NONE',  ( 9.121875000614517504, 3.027376345333611329, 5.243569643749999010 ) ) ;
#26173 = CARTESIAN_POINT ( 'NONE',  ( -3.756430356249999214, 12.82812499938548534, 27.83122392262697531 ) ) ;
#26174 = CARTESIAN_POINT ( 'NONE',  ( 23.66250000000000142, 2.886751345948126879, 4.999999999999999112 ) ) ;
#26175 = CARTESIAN_POINT ( 'NONE',  ( 4.000000000000000000, 14.78750000000000142, 27.69059892324149530 ) ) ;
#26176 = CARTESIAN_POINT ( 'NONE',  ( -3.999999999999999112, 9.725000001229036073, -32.30940107675850470 ) ) ;
#26177 = CARTESIAN_POINT ( 'NONE',  ( 25.28437500061451715, 4.119189519843966529, 2.378215178124999607 ) ) ;
#26178 = CARTESIAN_POINT ( 'NONE',  ( 11.54062500061451857, -3.027376345333610441, -5.243569643749999898 ) ) ;
#26179 = CARTESIAN_POINT ( 'NONE',  ( 3.262500000000001510, 2.886751345948129099, -4.999999999999998224 ) ) ;
#26180 = DIRECTION ( 'NONE',  ( -0.000000000000000000, -1.000000000000000000, -0.000000000000000000 ) ) ;
#26181 = CARTESIAN_POINT ( 'NONE',  ( 45.00000000000000000, 0.000000000000000000, 0.000000000000000000 ) ) ;
#26182 = CARTESIAN_POINT ( 'NONE',  ( 11.32500000000000107, 6.123233995736764310E-16, -4.999999999999998224 ) ) ;
#26183 = CARTESIAN_POINT ( 'NONE',  ( -2.828200636599751609E-16, 19.10000000122903074, 25.38119784648299770 ) ) ;
#26184 = CARTESIAN_POINT ( 'NONE',  ( 10.42500000122903536, -5.773502691896255534, -1.060575238724906372E-15 ) ) ;
#26185 = CARTESIAN_POINT ( 'NONE',  ( 21.60937500061451644, 4.541064518000418104, -2.621784821874998173 ) ) ;
#26186 = CARTESIAN_POINT ( 'NONE',  ( 16.20937500061451786, 4.541064518000418104, -2.621784821874998173 ) ) ;
#26187 = CARTESIAN_POINT ( 'NONE',  ( 7.181250001229034119, -4.330127018922194537, 2.499999999999995559 ) ) ;
#26188 = VERTEX_POINT ( 'NONE', #66902 ) ;
#26189 = CARTESIAN_POINT ( 'NONE',  ( 17.01562500061451644, 3.027376345333613106, -5.243569643749998122 ) ) ;
#26190 = CARTESIAN_POINT ( 'NONE',  ( 28.83750000122903145, -4.330127018922194537, 2.499999999999995559 ) ) ;
#26191 = CARTESIAN_POINT ( 'NONE',  ( 16.95937500061451786, -4.541064518000417216, -2.621784821875001281 ) ) ;
#26192 = CARTESIAN_POINT ( 'NONE',  ( 29.55937500061451573, -4.541064518000417216, -2.621784821875001281 ) ) ;
#26193 = CARTESIAN_POINT ( 'NONE',  ( 5.615625000614517859, -6.054752690667223547, -1.112240025338166033E-15 ) ) ;
#26194 = CARTESIAN_POINT ( 'NONE',  ( 18.40312500061451573, 4.541064518000418104, -2.621784821874998173 ) ) ;
#26195 = EDGE_CURVE ( 'NONE', #6463, #4282, #50826, .T. ) ;
#26196 = CARTESIAN_POINT ( 'NONE',  ( 28.13437500061451502, -4.541064518000419881, 2.621784821874995952 ) ) ;
#26197 = CARTESIAN_POINT ( 'NONE',  ( -3.000416591977282496E-16, 13.84062500061451928, 25.09994784771203058 ) ) ;
#26198 = CARTESIAN_POINT ( 'NONE',  ( 16.31250000122903288, -4.330127018922190985, -2.500000000000001332 ) ) ;
#26199 = CARTESIAN_POINT ( 'NONE',  ( 10.84687500061451715, 5.492252693125287522, 3.363034840372157021E-16 ) ) ;
#26200 = CARTESIAN_POINT ( 'NONE',  ( 7.640625000614517326, 6.054752690667223547, 3.707466751127219781E-16 ) ) ;
#26201 = CARTESIAN_POINT ( 'NONE',  ( 26.95312500061451644, 4.541064518000418104, -2.621784821874998173 ) ) ;
#26202 = CARTESIAN_POINT ( 'NONE',  ( 9.750000001229032875, 5.773502691896255534, 3.535250795749688401E-16 ) ) ;
#26203 = CARTESIAN_POINT ( 'NONE',  ( 22.02187500061452141, 3.027376345333613106, -5.243569643749998122 ) ) ;
#26204 = CARTESIAN_POINT ( 'NONE',  ( 11.99062500061451608, -3.027376345333610441, -5.243569643749999898 ) ) ;
#26205 = CARTESIAN_POINT ( 'NONE',  ( 22.38750000122903216, 4.330127018922191873, 2.499999999999999556 ) ) ;
#26206 = CARTESIAN_POINT ( 'NONE',  ( 23.27812500061451573, 6.421520780324663323E-16, -5.243569643749999010 ) ) ;
#26207 = CARTESIAN_POINT ( 'NONE',  ( 16.77187500061451786, 3.027376345333611329, 5.243569643749999010 ) ) ;
#26208 = CARTESIAN_POINT ( 'NONE',  ( 12.85312500061451502, -4.541064518000417216, -2.621784821875001281 ) ) ;
#26209 = CARTESIAN_POINT ( 'NONE',  ( -3.000416591977282496E-16, 14.79687500061451821, 25.09994784771203058 ) ) ;
#26210 = CARTESIAN_POINT ( 'NONE',  ( 20.87812500061451715, -4.541064518000419881, 2.621784821874995952 ) ) ;
#26211 = CARTESIAN_POINT ( 'NONE',  ( 10.16250000000000320, 2.886751345948126879, 4.999999999999998224 ) ) ;
#26212 = VERTEX_POINT ( 'NONE', #9646 ) ;
#26213 = ORIENTED_EDGE ( 'NONE', *, *, #14786, .F. ) ;
#26214 = CARTESIAN_POINT ( 'NONE',  ( 23.92499999999999716, 6.123233995736764310E-16, -4.999999999999998224 ) ) ;
#26215 = CARTESIAN_POINT ( 'NONE',  ( -2.121784821874999949, 18.43437500061451928, -33.67503911421598417 ) ) ;
#26216 = CARTESIAN_POINT ( 'NONE',  ( 16.19999999999999929, -4.330127018922190985, -2.500000000000001332 ) ) ;
#26217 = CARTESIAN_POINT ( 'NONE',  ( 25.94062500061451715, -3.027376345333610441, -5.243569643749999898 ) ) ;
#26218 = CARTESIAN_POINT ( 'NONE',  ( 4.528125000614516615, 4.541064518000418104, 2.621784821874999949 ) ) ;
#26219 = CARTESIAN_POINT ( 'NONE',  ( 19.27500000122903145, 2.886751345948126879, 4.999999999999999112 ) ) ;
#26220 = CARTESIAN_POINT ( 'NONE',  ( 24.14062500061451289, -3.027376345333610441, -5.243569643749999898 ) ) ;
#26221 = CARTESIAN_POINT ( 'NONE',  ( 23.28750000000000142, -2.886751345948129988, 4.999999999999997335 ) ) ;
#26222 = CARTESIAN_POINT ( 'NONE',  ( 28.04062500061451502, -3.027376345333614438, 5.243569643749998122 ) ) ;
#26223 = CARTESIAN_POINT ( 'NONE',  ( 7.190625000614518036, 6.054752690667223547, 3.707466751127219781E-16 ) ) ;
#26224 =( BOUNDED_CURVE ( )  B_SPLINE_CURVE ( 2, ( #38226, #16780, #72222, #50779, #182, #10887, #39338 ),
 .UNSPECIFIED., .F., .F. ) 
 B_SPLINE_CURVE_WITH_KNOTS ( ( 3, 2, 2, 3 ),
 ( 0.7399999999999999911, 0.7433333333333332904, 0.7466666666666667007, 0.7500000000000000000 ),
 .UNSPECIFIED. ) 
 CURVE ( )  GEOMETRIC_REPRESENTATION_ITEM ( )  RATIONAL_B_SPLINE_CURVE ( ( 1.000000000000000000, 0.8660254037844387076, 1.000000000000000000, 0.8660254037844387076, 1.000000000000000000, 0.8660254037844387076, 1.000000000000000000 ) ) 
 REPRESENTATION_ITEM ( '' )  );
#26225 = ORIENTED_EDGE ( 'NONE', *, *, #63349, .F. ) ;
#26226 = VECTOR ( 'NONE', #35186, 1000.000000000000000 ) ;
#26227 = CARTESIAN_POINT ( 'NONE',  ( 23.50312500061451360, 0.000000000000000000, 5.243569643749999010 ) ) ;
#26228 = CARTESIAN_POINT ( 'NONE',  ( 6.028125000614517504, -4.541064518000419881, 2.621784821874995952 ) ) ;
#26229 = CARTESIAN_POINT ( 'NONE',  ( 12.87187500061451750, -5.492252693125287522, -1.008910452111647106E-15 ) ) ;
#26230 = LINE ( 'NONE', #48768, #9926 ) ;
#26231 = CARTESIAN_POINT ( 'NONE',  ( 4.000000000000000000, 13.10000000122903430, -27.69059892324149530 ) ) ;
#26232 = CARTESIAN_POINT ( 'NONE',  ( 19.65000000000000213, 0.000000000000000000, 4.999999999999998224 ) ) ;
#26233 = EDGE_CURVE ( 'NONE', #64681, #24253, #65792, .T. ) ;
#26234 = CARTESIAN_POINT ( 'NONE',  ( 9.825000000000001066, -4.330127018922194537, 2.499999999999995559 ) ) ;
#26235 = CARTESIAN_POINT ( 'NONE',  ( 11.33437500061451608, 4.541064518000418104, 2.621784821874999949 ) ) ;
#26236 = CARTESIAN_POINT ( 'NONE',  ( 6.562500001229032875, 4.330127018922192761, -2.499999999999997780 ) ) ;
#26237 = CARTESIAN_POINT ( 'NONE',  ( 13.62187500061451750, 3.027376345333611329, 5.243569643749999010 ) ) ;
#26238 = CARTESIAN_POINT ( 'NONE',  ( 15.75000000000000000, -4.330127018922190985, -2.500000000000001332 ) ) ;
#26239 = CARTESIAN_POINT ( 'NONE',  ( 6.834375000614518747, 4.541064518000418104, 2.621784821874999949 ) ) ;
#26240 = CARTESIAN_POINT ( 'NONE',  ( -2.121784821874999949, 10.27812500061451750, -33.67503911421598417 ) ) ;
#26241 = CARTESIAN_POINT ( 'NONE',  ( 1.626862140677534273E-15, 9.875000001229034652, -26.00000000000000355 ) ) ;
#26242 = CARTESIAN_POINT ( 'NONE',  ( 12.45937500061451786, -4.541064518000417216, -2.621784821875001281 ) ) ;
#26243 = DIRECTION ( 'NONE',  ( -0.000000000000000000, -1.000000000000000000, -0.000000000000000000 ) ) ;
#26244 = CARTESIAN_POINT ( 'NONE',  ( 21.89062500061451289, -3.027376345333610441, -5.243569643749999898 ) ) ;
#26245 = CARTESIAN_POINT ( 'NONE',  ( 4.243569643749999898, 11.04687500061451644, 32.45002607614398471 ) ) ;
#26246 = CARTESIAN_POINT ( 'NONE',  ( 20.15625000122903288, 0.000000000000000000, 4.999999999999998224 ) ) ;
#26247 = CARTESIAN_POINT ( 'NONE',  ( 27.08437500061451786, 4.541064518000418104, 2.621784821874999949 ) ) ;
#26248 = CARTESIAN_POINT ( 'NONE',  ( -5.000000000000000000, 0.000000000000000000, -50.00000000000000000 ) ) ;
#26249 = CARTESIAN_POINT ( 'NONE',  ( 5.128125000614516260, -4.541064518000419881, 2.621784821874995952 ) ) ;
#26250 = CARTESIAN_POINT ( 'NONE',  ( 23.03437500061451360, -2.746126346562646425, 4.756430356249996549 ) ) ;
#26251 = CARTESIAN_POINT ( 'NONE',  ( 14.97187500061451892, 3.027376345333611329, 5.243569643749999010 ) ) ;
#26252 = CARTESIAN_POINT ( 'NONE',  ( 26.17500000122903359, -5.773502691896255534, -1.060575238724906372E-15 ) ) ;
#26253 = CARTESIAN_POINT ( 'NONE',  ( 28.05000000122903359, -2.886751345948125991, -5.000000000000000000 ) ) ;
#26254 = CARTESIAN_POINT ( 'NONE',  ( 5.596875000614516260, -3.027376345333614438, 5.243569643749998122 ) ) ;
#26255 = CARTESIAN_POINT ( 'NONE',  ( 16.73437500061451644, 4.541064518000418104, 2.621784821874999949 ) ) ;
#26256 = CARTESIAN_POINT ( 'NONE',  ( 30.00000000000000000, 0.000000000000000000, 0.000000000000000000 ) ) ;
#26257 = CARTESIAN_POINT ( 'NONE',  ( 23.81250000000000000, -5.773502691896255534, -1.060575238724906372E-15 ) ) ;
#26258 = CARTESIAN_POINT ( 'NONE',  ( 2.700000001229035718, -2.886751345948129988, 4.999999999999997335 ) ) ;
#26259 = CARTESIAN_POINT ( 'NONE',  ( 27.45937500061451786, 4.541064518000418104, -2.621784821874998173 ) ) ;
#26260 = CARTESIAN_POINT ( 'NONE',  ( -3.756430356249999214, 14.74062499938548498, 27.83122392262697531 ) ) ;
#26261 = FACE_OUTER_BOUND ( 'NONE', #10856, .T. ) ;
#26262 = CARTESIAN_POINT ( 'NONE',  ( 6.975000000000002309, 4.330127018922191873, 2.499999999999999556 ) ) ;
#26263 = CARTESIAN_POINT ( 'NONE',  ( 10.20937500061451608, 2.746126346562645981, -4.756430356249997438 ) ) ;
#26264 = CARTESIAN_POINT ( 'NONE',  ( 18.81562500061452070, 3.027376345333613106, -5.243569643749998122 ) ) ;
#26265 = CARTESIAN_POINT ( 'NONE',  ( 11.73750000000000249, -2.886751345948125991, -5.000000000000000000 ) ) ;
#26266 = CARTESIAN_POINT ( 'NONE',  ( 3.553125000614516082, 4.541064518000418104, -2.621784821874998173 ) ) ;
#26267 = CARTESIAN_POINT ( 'NONE',  ( 18.89999999999999858, -4.330127018922190985, -2.500000000000001332 ) ) ;
#26268 = CARTESIAN_POINT ( 'NONE',  ( 19.15312500061451573, -4.541064518000417216, -2.621784821875001281 ) ) ;
#26269 = CARTESIAN_POINT ( 'NONE',  ( 15.63750000122903216, 4.330127018922191873, 2.499999999999999556 ) ) ;
#26270 = CARTESIAN_POINT ( 'NONE',  ( 22.42500000122903359, 2.886751345948126879, 4.999999999999999112 ) ) ;
#26271 = CARTESIAN_POINT ( 'NONE',  ( -3.756430356249999214, 20.02812499938548285, 27.83122392262697176 ) ) ;
#26272 = CARTESIAN_POINT ( 'NONE',  ( 29.25937500061451502, 4.541064518000418104, -2.621784821874998173 ) ) ;
#26273 = ORIENTED_EDGE ( 'NONE', *, *, #62569, .T. ) ;
#26274 = CARTESIAN_POINT ( 'NONE',  ( 18.59062500061451573, -3.027376345333614438, 5.243569643749998122 ) ) ;
#26275 = CARTESIAN_POINT ( 'NONE',  ( 25.52812500061451573, 6.421520780324663323E-16, -5.243569643749999010 ) ) ;
#26276 = CARTESIAN_POINT ( 'NONE',  ( 25.13437500061451502, 6.421520780324663323E-16, -5.243569643749999010 ) ) ;
#26277 = CARTESIAN_POINT ( 'NONE',  ( 8.587500000000002132, -2.886751345948125991, -5.000000000000000000 ) ) ;
#26278 = CARTESIAN_POINT ( 'NONE',  ( 12.51562500061451821, 3.027376345333613106, -5.243569643749998122 ) ) ;
#26279 = CARTESIAN_POINT ( 'NONE',  ( 25.75312500061451715, 0.000000000000000000, 5.243569643749999010 ) ) ;
#26280 = CARTESIAN_POINT ( 'NONE',  ( 16.80937500061451573, 0.000000000000000000, 5.243569643749999010 ) ) ;
#26281 = CARTESIAN_POINT ( 'NONE',  ( 7.903125000614515727, -4.541064518000417216, -2.621784821875001281 ) ) ;
#26282 = DIRECTION ( 'NONE',  ( -0.000000000000000000, -1.000000000000000000, -0.000000000000000000 ) ) ;
#26283 = CARTESIAN_POINT ( 'NONE',  ( -0.7368881354385758975, 9.859898613939513723, 25.82089971438751519 ) ) ;
#26284 = CARTESIAN_POINT ( 'NONE',  ( 22.91250000122903430, 0.000000000000000000, 4.999999999999998224 ) ) ;
#26285 = CARTESIAN_POINT ( 'NONE',  ( 17.52187500061451431, 2.746126346562645981, -4.756430356249997438 ) ) ;
#26286 = CARTESIAN_POINT ( 'NONE',  ( 14.65312500061451573, -4.541064518000417216, -2.621784821875001281 ) ) ;
#26287 = CARTESIAN_POINT ( 'NONE',  ( 7.884375000614517681, -4.541064518000419881, 2.621784821874995952 ) ) ;
#26288 = CARTESIAN_POINT ( 'NONE',  ( 7.246875000614518392, 6.054752690667223547, 3.707466751127219781E-16 ) ) ;
#26289 = ORIENTED_EDGE ( 'NONE', *, *, #51085, .F. ) ;
#26290 = EDGE_CURVE ( 'NONE', #30796, #50879, #61570, .T. ) ;
#26291 = CARTESIAN_POINT ( 'NONE',  ( 29.14687500061451075, -3.027376345333610441, -5.243569643749999898 ) ) ;
#26292 = CARTESIAN_POINT ( 'NONE',  ( 22.67812500061451431, -4.541064518000419881, 2.621784821874995952 ) ) ;
#26293 = CARTESIAN_POINT ( 'NONE',  ( 16.54687500061451644, -3.027376345333610441, -5.243569643749999898 ) ) ;
#26294 = CARTESIAN_POINT ( 'NONE',  ( 19.56562500061451715, -6.054752690667223547, -1.112240025338166033E-15 ) ) ;
#26295 = CARTESIAN_POINT ( 'NONE',  ( 3.999999999999998668, 11.26250000000000107, 27.69059892324149175 ) ) ;
#26296 = CARTESIAN_POINT ( 'NONE',  ( 26.31562500061451715, -6.054752690667223547, -1.112240025338166033E-15 ) ) ;
#26297 = CARTESIAN_POINT ( 'NONE',  ( 8.025000001229035007, 2.886751345948126879, 4.999999999999999112 ) ) ;
#26298 = ORIENTED_EDGE ( 'NONE', *, *, #13854, .F. ) ;
#26299 = CARTESIAN_POINT ( 'NONE',  ( 29.84999999999999787, 4.330127018922192761, -2.499999999999997780 ) ) ;
#26300 = CARTESIAN_POINT ( 'NONE',  ( -1.999999999999997113, 18.27499999999999858, -26.53589838486224295 ) ) ;
#26301 = CARTESIAN_POINT ( 'NONE',  ( 24.33750000122903145, -4.330127018922194537, 2.499999999999995559 ) ) ;
#26302 = CARTESIAN_POINT ( 'NONE',  ( -3.756430356250000102, 14.32812499938548356, 30.00000000000000000 ) ) ;
#26303 = CARTESIAN_POINT ( 'NONE',  ( 6.646875000614518747, -3.027376345333610441, -5.243569643749999898 ) ) ;
#26304 = CARTESIAN_POINT ( 'NONE',  ( 30.00000000000000000, 0.000000000000000000, 0.000000000000000000 ) ) ;
#26305 = CARTESIAN_POINT ( 'NONE',  ( 13.07812500061451821, 4.541064518000418104, 2.621784821874999949 ) ) ;
#26306 = CARTESIAN_POINT ( 'NONE',  ( 8.596875000614518925, 6.054752690667223547, 3.707466751127219781E-16 ) ) ;
#26307 = CARTESIAN_POINT ( 'NONE',  ( 27.30000000122903359, 5.773502691896255534, 3.535250795749688894E-16 ) ) ;
#26308 = CARTESIAN_POINT ( 'NONE',  ( 16.69687500061451502, 6.054752690667223547, 3.707466751127219781E-16 ) ) ;
#26309 = CARTESIAN_POINT ( 'NONE',  ( 5.071875000614519458, 3.027376345333611329, 5.243569643749999010 ) ) ;
#26310 = CARTESIAN_POINT ( 'NONE',  ( -5.810221930991193690E-16, 10.88749999999999929, 26.00000000000000355 ) ) ;
#26311 = CARTESIAN_POINT ( 'NONE',  ( 5.653125000614517504, -4.541064518000417216, -2.621784821875001281 ) ) ;
#26312 = CARTESIAN_POINT ( 'NONE',  ( 16.15312500061451573, 4.541064518000418104, -2.621784821874998173 ) ) ;
#26313 = ORIENTED_EDGE ( 'NONE', *, *, #3226, .T. ) ;
#26314 = CARTESIAN_POINT ( 'NONE',  ( 11.61562500061451608, 3.027376345333613106, -5.243569643749998122 ) ) ;
#26315 = CARTESIAN_POINT ( 'NONE',  ( 5.775000001229033231, 2.886751345948126879, 4.999999999999999112 ) ) ;
#26316 = CARTESIAN_POINT ( 'NONE',  ( 8.615625000614517859, 3.027376345333611329, 5.243569643749999010 ) ) ;
#26317 = CARTESIAN_POINT ( 'NONE',  ( 22.35937500061451644, -4.119189519843965641, -2.378215178125001383 ) ) ;
#26318 = CARTESIAN_POINT ( 'NONE',  ( 8.775000000000002132, 4.330127018922191873, 2.499999999999999556 ) ) ;
#26319 = CARTESIAN_POINT ( 'NONE',  ( 3.187500001229033764, -4.330127018922194537, 2.499999999999995559 ) ) ;
#26320 = EDGE_CURVE ( 'NONE', #51781, #56470, #27733, .T. ) ;
#26321 = CARTESIAN_POINT ( 'NONE',  ( 17.06250000000000000, -5.773502691896255534, -1.060575238724906372E-15 ) ) ;
#26322 = ADVANCED_FACE ( 'NONE', ( #57871 ), #16990, .T. ) ;
#26323 = CARTESIAN_POINT ( 'NONE',  ( 17.48437500061451999, 6.421520780324663323E-16, -5.243569643749999010 ) ) ;
#26324 = CARTESIAN_POINT ( 'NONE',  ( 15.90000000122903501, -2.886751345948125991, -5.000000000000000000 ) ) ;
#26325 = CARTESIAN_POINT ( 'NONE',  ( 22.31250000000000000, 2.886751345948126879, 4.999999999999999112 ) ) ;
#26326 = CARTESIAN_POINT ( 'NONE',  ( -2.121784821874999949, 15.67812500061451608, -33.67503911421598417 ) ) ;
#26327 = CARTESIAN_POINT ( 'NONE',  ( 3.228971818887576006, 3.817556940351970685, 3.594618424259643508 ) ) ;
#26328 = CARTESIAN_POINT ( 'NONE',  ( 20.38125000122903430, 6.123233995736764310E-16, -4.999999999999998224 ) ) ;
#26329 = CARTESIAN_POINT ( 'NONE',  ( 28.11562500061451431, -6.054752690667223547, -1.112240025338166033E-15 ) ) ;
#26330 = CARTESIAN_POINT ( 'NONE',  ( 20.02500000122902790, 2.886751345948095793, -5.000000000000055067 ) ) ;
#26331 = CARTESIAN_POINT ( 'NONE',  ( 4.000000000000000000, 14.45000000122903572, 32.30940107675849760 ) ) ;
#26332 = CARTESIAN_POINT ( 'NONE',  ( 15.12187500061451750, -6.054752690667223547, -1.112240025338166033E-15 ) ) ;
#26333 = CARTESIAN_POINT ( 'NONE',  ( 29.21249999999999858, -5.773502691896255534, -1.060575238724906372E-15 ) ) ;
#26334 = CARTESIAN_POINT ( 'NONE',  ( 12.77812500061451750, -4.541064518000419881, 2.621784821874995952 ) ) ;
#26335 = CARTESIAN_POINT ( 'NONE',  ( 7.556250001229035007, 0.000000000000000000, 4.999999999999998224 ) ) ;
#26336 = CARTESIAN_POINT ( 'NONE',  ( 21.23437500061451644, 4.541064518000418104, 2.621784821874999949 ) ) ;
#26337 = CARTESIAN_POINT ( 'NONE',  ( 15.60937500061451644, 2.746126346562645981, -4.756430356249997438 ) ) ;
#26338 = CARTESIAN_POINT ( 'NONE',  ( 8.390625000614518214, -3.027376345333610441, -5.243569643749999898 ) ) ;
#26339 = CARTESIAN_POINT ( 'NONE',  ( 13.92187500061451644, 3.027376345333613106, -5.243569643749998122 ) ) ;
#26340 = VERTEX_POINT ( 'NONE', #47170 ) ;
#26341 = CARTESIAN_POINT ( 'NONE',  ( 23.33437500061451786, 6.421520780324663323E-16, -5.243569643749999010 ) ) ;
#26342 = CARTESIAN_POINT ( 'NONE',  ( 27.06562500061451004, 3.027376345333611329, 5.243569643749999010 ) ) ;
#26343 = FACE_BOUND ( 'NONE', #62914, .T. ) ;
#26344 = CARTESIAN_POINT ( 'NONE',  ( 8.099999999999999645, -4.330127018922190985, -2.500000000000001332 ) ) ;
#26345 = CARTESIAN_POINT ( 'NONE',  ( 17.70000000122903216, -2.886751345948125991, -5.000000000000000000 ) ) ;
#26346 = CARTESIAN_POINT ( 'NONE',  ( 7.320879633048903241E-15, 17.75000000122903288, -34.00000000000000000 ) ) ;
#26347 = CARTESIAN_POINT ( 'NONE',  ( 8.296875000614518214, -4.119189519843965641, -2.378215178125001383 ) ) ;
#26348 = ORIENTED_EDGE ( 'NONE', *, *, #66600, .T. ) ;
#26349 = CARTESIAN_POINT ( 'NONE',  ( 15.90000000000000036, 4.330127018922192761, -2.499999999999997780 ) ) ;
#26350 = CARTESIAN_POINT ( 'NONE',  ( 18.33749999999999858, -2.886751345948129988, 4.999999999999997335 ) ) ;
#26351 = CARTESIAN_POINT ( 'NONE',  ( 12.02812500061451573, 6.421520780324663323E-16, -5.243569643749999010 ) ) ;
#26352 = VERTEX_POINT ( 'NONE', #29810 ) ;
#26353 = CARTESIAN_POINT ( 'NONE',  ( -2.000000000000000000, 10.92500000000000071, -33.46410161513775705 ) ) ;
#26354 = CARTESIAN_POINT ( 'NONE',  ( 4.243569643749999010, 16.52187500061451786, -32.45002607614398471 ) ) ;
#26355 = CARTESIAN_POINT ( 'NONE',  ( 4.228125000614517681, -4.541064518000419881, 2.621784821874995952 ) ) ;
#26356 = LINE ( 'NONE', #15261, #41837 ) ;
#26357 = CARTESIAN_POINT ( 'NONE',  ( 10.01250000000000107, 2.886751345948129099, -4.999999999999998224 ) ) ;
#26358 = CARTESIAN_POINT ( 'NONE',  ( 20.77500000000000213, 6.123233995736764310E-16, -4.999999999999998224 ) ) ;
#26359 = ORIENTED_EDGE ( 'NONE', *, *, #27838, .F. ) ;
#26360 = CARTESIAN_POINT ( 'NONE',  ( 2.121784821875001281, 13.20312500061451821, 33.67503911421598417 ) ) ;
#26361 = CARTESIAN_POINT ( 'NONE',  ( 25.90312500061451573, -4.541064518000417216, -2.621784821875001281 ) ) ;
#26362 = LINE ( 'NONE', #61070, #49028 ) ;
#26363 = FACE_OUTER_BOUND ( 'NONE', #42619, .T. ) ;
#26364 = CARTESIAN_POINT ( 'NONE',  ( 20.48437500061451289, -4.541064518000419881, 2.621784821874995952 ) ) ;
#26365 = CARTESIAN_POINT ( 'NONE',  ( 19.19062500061452070, -3.027376345333610441, -5.243569643749999898 ) ) ;
#26366 = CARTESIAN_POINT ( 'NONE',  ( 4.243569643749999898, 13.27812500061459566, -30.00000000000000000 ) ) ;
#26367 = CARTESIAN_POINT ( 'NONE',  ( 24.52500000122903145, 2.886751345948129099, -4.999999999999998224 ) ) ;
#26368 = CARTESIAN_POINT ( 'NONE',  ( 3.140625000614516882, 6.054752690667223547, 3.707466751127219781E-16 ) ) ;
#26369 = CARTESIAN_POINT ( 'NONE',  ( 27.53437500061451360, 4.119189519843966529, 2.378215178124999607 ) ) ;
#26370 = CARTESIAN_POINT ( 'NONE',  ( 21.44062500061452070, -3.027376345333610441, -5.243569643749999898 ) ) ;
#26371 = CARTESIAN_POINT ( 'NONE',  ( 45.00000000000000000, 0.000000000000000000, 0.000000000000000000 ) ) ;
#26372 = CARTESIAN_POINT ( 'NONE',  ( -3.756430356249999214, 16.42812499938548143, 27.83122392262697531 ) ) ;
#26373 =( BOUNDED_CURVE ( )  B_SPLINE_CURVE ( 2, ( #49671, #10140, #33033, #27500, #26397, #48939, #72198 ),
 .UNSPECIFIED., .F., .F. ) 
 B_SPLINE_CURVE_WITH_KNOTS ( ( 3, 2, 2, 3 ),
 ( 0.8499999999999999778, 0.8527777777777777457, 0.8555555555555555136, 0.8583333333333332815 ),
 .UNSPECIFIED. ) 
 CURVE ( )  GEOMETRIC_REPRESENTATION_ITEM ( )  RATIONAL_B_SPLINE_CURVE ( ( 1.000000000000000000, 0.8660254037844387076, 1.000000000000000000, 0.8660254037844387076, 1.000000000000000000, 0.8660254037844387076, 1.000000000000000000 ) ) 
 REPRESENTATION_ITEM ( '' )  );
#26374 = CARTESIAN_POINT ( 'NONE',  ( 14.48437500061451821, 4.541064518000418104, 2.621784821874999949 ) ) ;
#26375 = CARTESIAN_POINT ( 'NONE',  ( 15.23437500061451644, 6.421520780324663323E-16, -5.243569643749999010 ) ) ;
#26376 = CARTESIAN_POINT ( 'NONE',  ( 25.77187500061451075, 3.027376345333611329, 5.243569643749999010 ) ) ;
#26377 = CARTESIAN_POINT ( 'NONE',  ( -2.121784821874999949, 14.83437500061451786, 26.32496088578401938 ) ) ;
#26378 = CARTESIAN_POINT ( 'NONE',  ( 4.940625000614515372, 6.054752690667223547, 3.707466751127219781E-16 ) ) ;
#26379 = CARTESIAN_POINT ( 'NONE',  ( 28.94062500061452070, -3.027376345333614438, 5.243569643749998122 ) ) ;
#26380 = CARTESIAN_POINT ( 'NONE',  ( 28.04062500061451502, -3.027376345333614438, 5.243569643749998122 ) ) ;
#26381 = CARTESIAN_POINT ( 'NONE',  ( 3.999999999999999112, 16.28750000122903430, -30.00000000000000000 ) ) ;
#26382 = CARTESIAN_POINT ( 'NONE',  ( -2.000000000000000000, 19.92500000000000071, 26.53589838486224650 ) ) ;
#26383 = CARTESIAN_POINT ( 'NONE',  ( 7.134375000614516793, 6.421520780324663323E-16, -5.243569643749999010 ) ) ;
#26384 = APPLICATION_PROTOCOL_DEFINITION ( 'draft international standard', 'automotive_design', 1998, #46934 ) ;
#26385 = CARTESIAN_POINT ( 'NONE',  ( 15.07500000122903394, 2.886751345948129099, -4.999999999999998224 ) ) ;
#26386 = CARTESIAN_POINT ( 'NONE',  ( 10.42500000122903536, -5.773502691896255534, -1.060575238724906372E-15 ) ) ;
#26387 = CARTESIAN_POINT ( 'NONE',  ( 4.603125000614518569, 0.000000000000000000, 5.243569643749999010 ) ) ;
#26388 = CARTESIAN_POINT ( 'NONE',  ( -2.000000000000001776, 16.79374999877096641, 33.46410161513775705 ) ) ;
#26389 = CARTESIAN_POINT ( 'NONE',  ( 19.51875000122903359, 2.886751345948129099, -4.999999999999998224 ) ) ;
#26390 = CARTESIAN_POINT ( 'NONE',  ( 13.58437500061451786, 4.541064518000418104, 2.621784821874999949 ) ) ;
#26391 = CARTESIAN_POINT ( 'NONE',  ( 21.03750000000000142, -2.886751345948096681, 5.000000000000054179 ) ) ;
#26392 = ORIENTED_EDGE ( 'NONE', *, *, #59010, .T. ) ;
#26393 = CARTESIAN_POINT ( 'NONE',  ( 22.67812500061451431, -4.541064518000419881, 2.621784821874995952 ) ) ;
#26394 = CARTESIAN_POINT ( 'NONE',  ( 8.278125000614515727, -4.541064518000419881, 2.621784821874995952 ) ) ;
#26395 = CARTESIAN_POINT ( 'NONE',  ( 25.69687500061451502, 6.054752690667223547, 3.707466751127219781E-16 ) ) ;
#26396 = CARTESIAN_POINT ( 'NONE',  ( 8.053125000614516082, 4.541064518000418104, -2.621784821874998173 ) ) ;
#26397 = CARTESIAN_POINT ( 'NONE',  ( 6.562500001229032875, 4.330127018922192761, -2.499999999999997780 ) ) ;
#26398 = CARTESIAN_POINT ( 'NONE',  ( 8.512500001229033941, 0.000000000000000000, 4.999999999999998224 ) ) ;
#26399 = CARTESIAN_POINT ( 'NONE',  ( 23.69062500061451004, -3.027376345333610441, -5.243569643749999898 ) ) ;
#26400 = CARTESIAN_POINT ( 'NONE',  ( -4.243569643749999898, 10.76562500061451644, -32.45002607614398471 ) ) ;
#26401 = CARTESIAN_POINT ( 'NONE',  ( 10.65000000122903323, 5.773502691896255534, 3.535250795749688894E-16 ) ) ;
#26402 = CARTESIAN_POINT ( 'NONE',  ( 18.70312500061451644, -4.541064518000417216, -2.621784821875001281 ) ) ;
#26403 = CARTESIAN_POINT ( 'NONE',  ( 14.46562500061451750, 3.027376345333611329, 5.243569643749999010 ) ) ;
#26404 = CARTESIAN_POINT ( 'NONE',  ( 28.17187500061451644, -5.492252693125287522, -1.008910452111647106E-15 ) ) ;
#26405 = CARTESIAN_POINT ( 'NONE',  ( 14.84999999999999964, -4.330127018922190985, -2.500000000000001332 ) ) ;
#26406 = CARTESIAN_POINT ( 'NONE',  ( 10.27500000122903323, 2.886751345948126879, 4.999999999999999112 ) ) ;
#26407 = CARTESIAN_POINT ( 'NONE',  ( 7.565625000614518036, 3.027376345333613106, -5.243569643749998122 ) ) ;
#26408 = CARTESIAN_POINT ( 'NONE',  ( 11.42812500061451608, -4.541064518000419881, 2.621784821874995952 ) ) ;
#26409 = EDGE_CURVE ( 'NONE', #12792, #45611, #58338, .T. ) ;
#26410 = CARTESIAN_POINT ( 'NONE',  ( 22.16250000122903074, -4.330127018922190985, -2.500000000000001332 ) ) ;
#26411 = CARTESIAN_POINT ( 'NONE',  ( 19.39687500061451786, 6.054752690667223547, 3.707466751127219781E-16 ) ) ;
#26412 = CARTESIAN_POINT ( 'NONE',  ( 65.00000000000000000, 6.363961030679004871, 6.363961030678849440 ) ) ;
#26413 = CARTESIAN_POINT ( 'NONE',  ( 4.312500001229034652, 4.330127018922192761, -2.499999999999997780 ) ) ;
#26414 =( BOUNDED_CURVE ( )  B_SPLINE_CURVE ( 2, ( #50104, #34181, #38655, #62270, #10574, #10933, #50825 ),
 .UNSPECIFIED., .F., .F. ) 
 B_SPLINE_CURVE_WITH_KNOTS ( ( 3, 2, 2, 3 ),
 ( 0.9699999999999999734, 0.9733333333333333837, 0.9766666666666666829, 0.9799999999999999822 ),
 .UNSPECIFIED. ) 
 CURVE ( )  GEOMETRIC_REPRESENTATION_ITEM ( )  RATIONAL_B_SPLINE_CURVE ( ( 1.000000000000000000, 0.8660254037844387076, 1.000000000000000000, 0.8660254037844387076, 1.000000000000000000, 0.8660254037844387076, 1.000000000000000000 ) ) 
 REPRESENTATION_ITEM ( '' )  );
#26415 = CARTESIAN_POINT ( 'NONE',  ( 4.846875000614519813, -3.027376345333610441, -5.243569643749999898 ) ) ;
#26416 = CARTESIAN_POINT ( 'NONE',  ( 24.38437500061451502, 4.541064518000418104, 2.621784821874999949 ) ) ;
#26417 =( BOUNDED_CURVE ( )  B_SPLINE_CURVE ( 2, ( #17695, #21, #17343, #39533, #56156, #38811, #34697 ),
 .UNSPECIFIED., .F., .F. ) 
 B_SPLINE_CURVE_WITH_KNOTS ( ( 3, 2, 2, 3 ),
 ( 0.4249999999999999889, 0.4277777777777777568, 0.4305555555555555802, 0.4333333333333333481 ),
 .UNSPECIFIED. ) 
 CURVE ( )  GEOMETRIC_REPRESENTATION_ITEM ( )  RATIONAL_B_SPLINE_CURVE ( ( 1.000000000000000000, 0.8660254037844387076, 1.000000000000000000, 0.8660254037844387076, 1.000000000000000000, 0.8660254037844387076, 1.000000000000000000 ) ) 
 REPRESENTATION_ITEM ( '' )  );
#26418 = LINE ( 'NONE', #2421, #19687 ) ;
#26419 = CARTESIAN_POINT ( 'NONE',  ( 19.71562500061451928, 3.027376345333613106, -5.243569643749998122 ) ) ;
#26420 = CARTESIAN_POINT ( 'NONE',  ( 25.43437500061451573, -4.541064518000419881, 2.621784821874995952 ) ) ;
#26421 = CARTESIAN_POINT ( 'NONE',  ( -7.967954043666661671E-16, 20.29062499938548569, 34.33755215474603517 ) ) ;
#26422 = CARTESIAN_POINT ( 'NONE',  ( 12.33750000122903145, 6.123233995736764310E-16, -4.999999999999998224 ) ) ;
#26423 = LINE ( 'NONE', #48964, #44273 ) ;
#26424 = CARTESIAN_POINT ( 'NONE',  ( 4.584375000614516971, 4.541064518000418104, 2.621784821874999949 ) ) ;
#26425 = AXIS2_PLACEMENT_3D ( 'NONE', #67141, #16499, #10969 ) ;
#26426 = CARTESIAN_POINT ( 'NONE',  ( 15.06562500061451537, -6.054752690667223547, -1.112240025338166033E-15 ) ) ;
#26427 = CARTESIAN_POINT ( 'NONE',  ( 13.47187500061451537, 3.027376345333613106, -5.243569643749998122 ) ) ;
#26428 = ORIENTED_EDGE ( 'NONE', *, *, #57573, .T. ) ;
#26429 = CARTESIAN_POINT ( 'NONE',  ( 9.225000000000001421, 4.330127018922191873, 2.499999999999999556 ) ) ;
#26430 = CARTESIAN_POINT ( 'NONE',  ( 26.05312500061451431, 4.541064518000418104, -2.621784821874998173 ) ) ;
#26431 = CARTESIAN_POINT ( 'NONE',  ( 3.447219858367251533, 3.621695079390137018, -3.577502417051553696 ) ) ;
#26432 = CARTESIAN_POINT ( 'NONE',  ( -3.999999999999997335, 11.60000000122903430, -27.69059892324149530 ) ) ;
#26433 = CARTESIAN_POINT ( 'NONE',  ( 13.98750000000000249, -2.886751345948125991, -5.000000000000000000 ) ) ;
#26434 = CARTESIAN_POINT ( 'NONE',  ( 23.96250000122903145, -4.330127018922190985, -2.500000000000001332 ) ) ;
#26435 = CARTESIAN_POINT ( 'NONE',  ( 18.44062500061451715, 6.054752690667223547, 3.707466751127219781E-16 ) ) ;
#26436 = EDGE_LOOP ( 'NONE', ( #35002, #41040, #69143, #10915 ) ) ;
#26437 = CARTESIAN_POINT ( 'NONE',  ( 23.17500000000000071, 4.330127018922191873, 2.499999999999999556 ) ) ;
#26438 = CARTESIAN_POINT ( 'NONE',  ( 23.97187500061451360, 3.027376345333611329, 5.243569643749999010 ) ) ;
#26439 =( BOUNDED_CURVE ( )  B_SPLINE_CURVE ( 2, ( #9811, #61874, #11281, #5735, #48981, #71510, #32343 ),
 .UNSPECIFIED., .F., .F. ) 
 B_SPLINE_CURVE_WITH_KNOTS ( ( 3, 2, 2, 3 ),
 ( 0.4799999999999999267, 0.4833333333333333370, 0.4866666666666667473, 0.4900000000000001021 ),
 .UNSPECIFIED. ) 
 CURVE ( )  GEOMETRIC_REPRESENTATION_ITEM ( )  RATIONAL_B_SPLINE_CURVE ( ( 1.000000000000002220, 0.8660254037844364872, 1.000000000000000000, 0.8660254037844387076, 1.000000000000000000, 0.8660254037844342667, 1.000000000000004441 ) ) 
 REPRESENTATION_ITEM ( '' )  );
#26440 = VERTEX_POINT ( 'NONE', #18705 ) ;
#26441 = CARTESIAN_POINT ( 'NONE',  ( 3.002593080208402654, -3.998053875910604127, -3.392725720445497473 ) ) ;
#26442 = CARTESIAN_POINT ( 'NONE',  ( 11.01562500061451821, -6.054752690667223547, -1.112240025338166033E-15 ) ) ;
#26443 = CARTESIAN_POINT ( 'NONE',  ( 2.915625000614516793, -6.054752690667223547, -1.112240025338166033E-15 ) ) ;
#26444 = CARTESIAN_POINT ( 'NONE',  ( 14.85937500061451999, 2.746126346562643317, 4.756430356249998326 ) ) ;
#26445 = CARTESIAN_POINT ( 'NONE',  ( 27.92812500061451431, 4.541064518000418104, 2.621784821874999949 ) ) ;
#26446 = CARTESIAN_POINT ( 'NONE',  ( 18.07499999999999929, 6.123233995736764310E-16, -4.999999999999998224 ) ) ;
#26447 = CARTESIAN_POINT ( 'NONE',  ( 25.94999999999999929, 0.000000000000000000, 4.999999999999998224 ) ) ;
#26448 = CARTESIAN_POINT ( 'NONE',  ( 4.000000000000000000, 10.73750000000000071, -27.69059892324149885 ) ) ;
#26449 = CARTESIAN_POINT ( 'NONE',  ( 7.246875000614518392, 6.054752690667223547, 3.707466751127219781E-16 ) ) ;
#26450 = CARTESIAN_POINT ( 'NONE',  ( 18.00937500061451502, 4.541064518000418104, -2.621784821874998173 ) ) ;
#26451 = CARTESIAN_POINT ( 'NONE',  ( 30.00000000000000000, 0.000000000000000000, 0.000000000000000000 ) ) ;
#26452 = ORIENTED_EDGE ( 'NONE', *, *, #72086, .F. ) ;
#26453 = CARTESIAN_POINT ( 'NONE',  ( 27.47812500061451502, 4.541064518000418104, 2.621784821874999949 ) ) ;
#26454 = CARTESIAN_POINT ( 'NONE',  ( 26.89687500061451431, -3.027376345333610441, -5.243569643749999898 ) ) ;
#26455 = CARTESIAN_POINT ( 'NONE',  ( 16.81875000122903074, 2.886751345948073588, -5.000000000000094147 ) ) ;
#26456 = CARTESIAN_POINT ( 'NONE',  ( 13.42499999999999893, -4.330127018922194537, 2.499999999999995559 ) ) ;
#26457 = CARTESIAN_POINT ( 'NONE',  ( 10.37812500061451715, 4.541064518000418104, 2.621784821874999949 ) ) ;
#26458 = CARTESIAN_POINT ( 'NONE',  ( -1.071796769724492115, 19.56740381056766509, 34.00000000000000000 ) ) ;
#26459 = CARTESIAN_POINT ( 'NONE',  ( -1.626862140677534273E-15, 18.18124999877096215, 34.00000000000000000 ) ) ;
#26460 = CARTESIAN_POINT ( 'NONE',  ( -0.7368881354385758975, 9.803648613939513368, -34.17910028561248481 ) ) ;
#26461 = CARTESIAN_POINT ( 'NONE',  ( 16.08750000122903501, 4.330127018922191873, 2.499999999999999556 ) ) ;
#26462 = CARTESIAN_POINT ( 'NONE',  ( 15.15000000122903323, 5.773502691896255534, 3.535250795749688401E-16 ) ) ;
#26463 = CARTESIAN_POINT ( 'NONE',  ( 15.23437500061451644, 5.824947211148865298E-16, -4.756430356249998326 ) ) ;
#26464 = CARTESIAN_POINT ( 'NONE',  ( 4.415625000614518569, 3.027376345333613106, -5.243569643749998122 ) ) ;
#26465 = CARTESIAN_POINT ( 'NONE',  ( 22.02187500061452141, 3.027376345333613106, -5.243569643749998122 ) ) ;
#26466 = CARTESIAN_POINT ( 'NONE',  ( 4.243569643749999898, 18.24687500061451928, 32.45002607614398471 ) ) ;
#26467 = CARTESIAN_POINT ( 'NONE',  ( 23.18437500061451573, -4.541064518000419881, 2.621784821874995952 ) ) ;
#26468 = CARTESIAN_POINT ( 'NONE',  ( 4.575000000000002842, 6.123233995736764310E-16, -4.999999999999998224 ) ) ;
#26469 = CARTESIAN_POINT ( 'NONE',  ( -3.999999999999997335, 10.70000000122903394, 32.30940107675850470 ) ) ;
#26470 = CARTESIAN_POINT ( 'NONE',  ( 12.25312500061451537, 0.000000000000000000, 5.243569643749999010 ) ) ;
#26471 = CARTESIAN_POINT ( 'NONE',  ( 4.950000001229033941, -2.886751345948129988, 4.999999999999997335 ) ) ;
#26472 = EDGE_CURVE ( 'NONE', #18997, #32666, #41269, .T. ) ;
#26473 = CARTESIAN_POINT ( 'NONE',  ( 9.084375000614517859, 4.541064518000418104, 2.621784821874999949 ) ) ;
#26474 = CARTESIAN_POINT ( 'NONE',  ( 9.440625000614517148, 6.054752690667223547, 3.707466751127219781E-16 ) ) ;
#26475 = CARTESIAN_POINT ( 'NONE',  ( 13.99687500061451928, 6.054752690667223547, 3.707466751127219781E-16 ) ) ;
#26476 = CARTESIAN_POINT ( 'NONE',  ( -1.999999999999999112, 18.95000000000000284, 26.53589838486224650 ) ) ;
#26477 = CARTESIAN_POINT ( 'NONE',  ( 21.33750000122903145, 6.123233995736764310E-16, -4.999999999999998224 ) ) ;
#26478 = CARTESIAN_POINT ( 'NONE',  ( 10.13437500061451679, -4.541064518000419881, 2.621784821874995952 ) ) ;
#26479 = CARTESIAN_POINT ( 'NONE',  ( 13.15312500061451750, 0.000000000000000000, 5.243569643749999010 ) ) ;
#26480 = CARTESIAN_POINT ( 'NONE',  ( 28.21875000122903288, 2.886751345948126879, 4.999999999999999112 ) ) ;
#26481 = CARTESIAN_POINT ( 'NONE',  ( 21.83437500061451786, -4.541064518000419881, 2.621784821874995952 ) ) ;
#26482 = CARTESIAN_POINT ( 'NONE',  ( 25.50000000122903288, 5.773502691896255534, 3.535250795749688401E-16 ) ) ;
#26483 = CARTESIAN_POINT ( 'NONE',  ( -3.963752180954429605, 3.047823949009539124, 30.55459436224499115 ) ) ;
#26484 = CARTESIAN_POINT ( 'NONE',  ( 3.274239950736235638, 3.778839813355128641, -3.307020945026925673 ) ) ;
#26485 = CARTESIAN_POINT ( 'NONE',  ( 2.121784821875001281, 11.45937500061451786, -26.32496088578401938 ) ) ;
#26486 = CARTESIAN_POINT ( 'NONE',  ( 15.63750000122903216, 4.330127018922191873, 2.499999999999999556 ) ) ;
#26487 = CARTESIAN_POINT ( 'NONE',  ( 10.54687500061451644, -3.027376345333614438, 5.243569643749998122 ) ) ;
#26488 = CARTESIAN_POINT ( 'NONE',  ( -3.000416591977282496E-16, 17.44062500061451360, -34.90005215228797653 ) ) ;
#26489 = CARTESIAN_POINT ( 'NONE',  ( 18.15000000122903501, -2.886751345948125991, -5.000000000000000000 ) ) ;
#26490 = CARTESIAN_POINT ( 'NONE',  ( 10.86562500061451431, 3.027376345333611329, 5.243569643749999010 ) ) ;
#26491 = VERTEX_POINT ( 'NONE', #11466 ) ;
#26492 = CARTESIAN_POINT ( 'NONE',  ( 15.07499999999999929, 4.330127018922191873, 2.499999999999999556 ) ) ;
#26493 = CARTESIAN_POINT ( 'NONE',  ( 4.678147931978664076, 1.767710935909229342, -4.678147931978664076 ) ) ;
#26494 = CARTESIAN_POINT ( 'NONE',  ( 10.80937500061451928, 4.541064518000418104, -2.621784821874998173 ) ) ;
#26495 = EDGE_CURVE ( 'NONE', #43576, #12632, #40465, .T. ) ;
#26496 = CARTESIAN_POINT ( 'NONE',  ( 2.972982959257041813, 4.020181188108474579, -3.027672370053282158 ) ) ;
#26497 = CARTESIAN_POINT ( 'NONE',  ( 9.337500001229033231, 4.330127018922191873, 2.499999999999999556 ) ) ;
#26498 = CARTESIAN_POINT ( 'NONE',  ( 18.11250000122903359, -4.330127018922190985, -2.500000000000001332 ) ) ;
#26499 = VECTOR ( 'NONE', #65390, 1000.000000000000000 ) ;
#26500 = CARTESIAN_POINT ( 'NONE',  ( 14.57812500061451644, -4.541064518000419881, 2.621784821874995952 ) ) ;
#26501 = CARTESIAN_POINT ( 'NONE',  ( 18.81562500061452070, 3.027376345333613106, -5.243569643749998122 ) ) ;
#26502 = CARTESIAN_POINT ( 'NONE',  ( 28.91250000122903074, -4.330127018922190985, -2.500000000000001332 ) ) ;
#26503 = VECTOR ( 'NONE', #37711, 1000.000000000000000 ) ;
#26504 = CARTESIAN_POINT ( 'NONE',  ( 29.51250000122903216, 4.330127018922192761, -2.499999999999997780 ) ) ;
#26505 = CARTESIAN_POINT ( 'NONE',  ( 24.03750000000000142, 5.773502691896255534, 3.535250795749688894E-16 ) ) ;
#26506 = CARTESIAN_POINT ( 'NONE',  ( -3.756430356250001434, 13.35312499938548392, 32.16877607737301048 ) ) ;
#26507 = AXIS2_PLACEMENT_3D ( 'NONE', #64746, #35938, #58461 ) ;
#26508 = CARTESIAN_POINT ( 'NONE',  ( 26.28749999999999432, 5.773502691896255534, 3.535250795749688894E-16 ) ) ;
#26509 = CARTESIAN_POINT ( 'NONE',  ( 24.90937500061451715, 0.000000000000000000, 5.243569643749999010 ) ) ;
#26510 = FACE_OUTER_BOUND ( 'NONE', #34959, .T. ) ;
#26511 = CARTESIAN_POINT ( 'NONE',  ( 13.08750000122903323, -4.330127018922194537, 2.499999999999995559 ) ) ;
#26512 = CARTESIAN_POINT ( 'NONE',  ( 29.52187500061451431, -6.054752690667223547, -1.112240025338166033E-15 ) ) ;
#26513 = EDGE_CURVE ( 'NONE', #29218, #71220, #68662, .T. ) ;
#26514 = CARTESIAN_POINT ( 'NONE',  ( 12.48750000000000249, -2.886751345948074920, 5.000000000000092371 ) ) ;
#26515 = CARTESIAN_POINT ( 'NONE',  ( 6.346875000614517148, 6.054752690667223547, 3.707466751127219781E-16 ) ) ;
#26516 = B_SPLINE_CURVE_WITH_KNOTS ( 'NONE', 3,
 ( #2201, #47259, #71991, #60891, #66819, #9924, #45010, #16192, #54997, #21365 ),
 .UNSPECIFIED., .F., .F.,
 ( 4, 3, 3, 4 ),
 ( 1.914080865847744861E-16, 2.812508936123897185E-05, 5.625017725354377072E-05, 0.0001049420589380106804 ),
 .UNSPECIFIED. ) ;
#26517 = CARTESIAN_POINT ( 'NONE',  ( 26.39062500061451644, -3.027376345333610441, -5.243569643749999898 ) ) ;
#26518 = CARTESIAN_POINT ( 'NONE',  ( -6.275039685470489619E-15, 17.97500000122903074, -26.00000000000000355 ) ) ;
#26519 = CARTESIAN_POINT ( 'NONE',  ( -1.585543809737899990, 9.875380255848552835, -24.20988672647330731 ) ) ;
#26520 = CARTESIAN_POINT ( 'NONE',  ( -4.000000000000000000, 16.77499999999999858, 30.00000000000000000 ) ) ;
#26521 = CARTESIAN_POINT ( 'NONE',  ( 6.421875000614519102, 3.027376345333611329, 5.243569643749999010 ) ) ;
#26522 = CARTESIAN_POINT ( 'NONE',  ( 9.984375000614518214, 4.541064518000418104, 2.621784821874999949 ) ) ;
#26523 = CARTESIAN_POINT ( 'NONE',  ( 29.40937500061451715, 0.000000000000000000, 5.243569643749999010 ) ) ;
#26524 = CARTESIAN_POINT ( 'NONE',  ( 4.243569643749999010, 11.96562500061459389, 27.54997392385601174 ) ) ;
#26525 = CARTESIAN_POINT ( 'NONE',  ( 22.01249999999999574, -5.773502691896255534, -1.060575238724906372E-15 ) ) ;
#26526 = CARTESIAN_POINT ( 'NONE',  ( 29.85937500061451644, 0.000000000000000000, 5.243569643749999010 ) ) ;
#26527 = VERTEX_POINT ( 'NONE', #53068 ) ;
#26528 = CARTESIAN_POINT ( 'NONE',  ( 18.10312500061451502, 0.000000000000000000, 5.243569643749999010 ) ) ;
#26529 = CARTESIAN_POINT ( 'NONE',  ( 11.09062500061451573, -3.027376345333610441, -5.243569643749999898 ) ) ;
#26530 = CARTESIAN_POINT ( 'NONE',  ( 21.60937500061451644, 2.746126346562643317, 4.756430356249998326 ) ) ;
#26531 = CARTESIAN_POINT ( 'NONE',  ( 8.109375000614518214, 4.541064518000418104, -2.621784821874998173 ) ) ;
#26532 = CARTESIAN_POINT ( 'NONE',  ( 24.71250000000000213, -5.773502691896255534, -1.060575238724906372E-15 ) ) ;
#26533 = CARTESIAN_POINT ( 'NONE',  ( 20.66250000122903074, 0.000000000000000000, 4.999999999999998224 ) ) ;
#26534 = CIRCLE ( 'NONE', #45370, 1.500000000000000222 ) ;
#26535 = CARTESIAN_POINT ( 'NONE',  ( 15.95625000122903181, 4.330127018922192761, -2.499999999999997780 ) ) ;
#26536 = CARTESIAN_POINT ( 'NONE',  ( 8.521875000614516082, 3.027376345333613106, -5.243569643749998122 ) ) ;
#26537 = CARTESIAN_POINT ( 'NONE',  ( 14.10937500061451644, 0.000000000000000000, 5.243569643749999010 ) ) ;
#26538 = CARTESIAN_POINT ( 'NONE',  ( 25.28437500061451715, 4.541064518000418104, 2.621784821874999949 ) ) ;
#26539 = FACE_OUTER_BOUND ( 'NONE', #28983, .T. ) ;
#26540 = CARTESIAN_POINT ( 'NONE',  ( 13.91249999999999964, -5.773502691896255534, -1.060575238724906372E-15 ) ) ;
#26541 = CARTESIAN_POINT ( 'NONE',  ( 18.49687500061452283, 6.054752690667223547, 3.707466751127219781E-16 ) ) ;
#26542 = VECTOR ( 'NONE', #13869, 1000.000000000000000 ) ;
#26543 = CARTESIAN_POINT ( 'NONE',  ( 8.296875000614516438, -3.027376345333614438, 5.243569643749998122 ) ) ;
#26544 = CARTESIAN_POINT ( 'NONE',  ( 0.6522972858965978560, 20.75364861271052419, 33.69936173848522998 ) ) ;
#26545 = CARTESIAN_POINT ( 'NONE',  ( 20.02500000000000213, 4.330127018922191873, 2.499999999999999556 ) ) ;
#26546 = CARTESIAN_POINT ( 'NONE',  ( 2.828200636599751609E-16, 15.76249999999999751, 25.38119784648299415 ) ) ;
#26547 = CARTESIAN_POINT ( 'NONE',  ( 29.88749999999999929, 5.773502691896255534, 3.535250795749688401E-16 ) ) ;
#26548 = CARTESIAN_POINT ( 'NONE',  ( 25.50937500061451502, -4.119189519843965641, -2.378215178125001383 ) ) ;
#26549 = CARTESIAN_POINT ( 'NONE',  ( 13.00312500061451537, 4.541064518000418104, -2.621784821874998173 ) ) ;
#26550 = CARTESIAN_POINT ( 'NONE',  ( 28.62187500061451573, -6.054752690667223547, -1.112240025338166033E-15 ) ) ;
#26551 = DIRECTION ( 'NONE',  ( 0.000000000000000000, 0.000000000000000000, -1.000000000000000000 ) ) ;
#26552 = CARTESIAN_POINT ( 'NONE',  ( 45.00000000000000000, 7.332543590861092753, -5.218601775200125914 ) ) ;
#26553 = CARTESIAN_POINT ( 'NONE',  ( 11.62500000000000000, -4.330127018922194537, 2.499999999999995559 ) ) ;
#26554 = CARTESIAN_POINT ( 'NONE',  ( -2.000000000000000000, 18.23750000122903359, 26.53589838486224650 ) ) ;
#26555 = CARTESIAN_POINT ( 'NONE',  ( 12.60000000122903430, -2.886751345948129988, 4.999999999999997335 ) ) ;
#26556 = CARTESIAN_POINT ( 'NONE',  ( 21.94687500061451857, -3.027376345333610441, -5.243569643749999898 ) ) ;
#26557 = CARTESIAN_POINT ( 'NONE',  ( 17.33437500061451431, -4.541064518000419881, 2.621784821874995952 ) ) ;
#26558 = CARTESIAN_POINT ( 'NONE',  ( 0.000000000000000000, -4.999999999999999112, 0.000000000000000000 ) ) ;
#26559 = VERTEX_POINT ( 'NONE', #2463 ) ;
#26560 = CARTESIAN_POINT ( 'NONE',  ( 17.09062500061451573, 6.054752690667223547, 3.707466751127219781E-16 ) ) ;
#26561 = CARTESIAN_POINT ( 'NONE',  ( 27.86250000122903359, 0.000000000000000000, 4.999999999999998224 ) ) ;
#26562 = CARTESIAN_POINT ( 'NONE',  ( 17.63437500061451502, 4.541064518000418104, 2.621784821874999949 ) ) ;
#26563 = CARTESIAN_POINT ( 'NONE',  ( 5.840625000614516615, 6.054752690667223547, 3.707466751127219781E-16 ) ) ;
#26564 = CARTESIAN_POINT ( 'NONE',  ( 20.12812500061451715, 6.421520780324663323E-16, -5.243569643749999010 ) ) ;
#26565 = CARTESIAN_POINT ( 'NONE',  ( -1.071796769724496556, 16.94240381056766509, -26.00000000000000355 ) ) ;
#26566 = CARTESIAN_POINT ( 'NONE',  ( 28.09687500061451360, -3.027376345333614438, 5.243569643749998122 ) ) ;
#26567 = CARTESIAN_POINT ( 'NONE',  ( -2.121784821874999949, 13.42812500061451786, 26.32496088578401938 ) ) ;
#26568 = CARTESIAN_POINT ( 'NONE',  ( 15.90000000122903501, -2.886751345948125991, -5.000000000000000000 ) ) ;
#26569 = CARTESIAN_POINT ( 'NONE',  ( 10.58437500061451964, -4.119189519843968306, 2.378215178124996054 ) ) ;
#26570 = CARTESIAN_POINT ( 'NONE',  ( 27.17812500061451786, -4.541064518000419881, 2.621784821874995952 ) ) ;
#26571 = CARTESIAN_POINT ( 'NONE',  ( -3.999999999999999112, 9.762500001229033941, 30.00000000000000000 ) ) ;
#26572 = ADVANCED_FACE ( 'NONE', ( #35 ), #58960, .F. ) ;
#26573 = CARTESIAN_POINT ( 'NONE',  ( 20.74687500061451573, 6.054752690667223547, 3.707466751127219781E-16 ) ) ;
#26574 = CARTESIAN_POINT ( 'NONE',  ( 21.90000000122903145, 5.773502691896255534, 3.535250795749688894E-16 ) ) ;
#26575 = CARTESIAN_POINT ( 'NONE',  ( 23.50312500061451360, 0.000000000000000000, 5.243569643749999010 ) ) ;
#26576 = CARTESIAN_POINT ( 'NONE',  ( 17.70937500061451431, 0.000000000000000000, 5.243569643749999010 ) ) ;
#26577 = CARTESIAN_POINT ( 'NONE',  ( 11.35312500061451679, 0.000000000000000000, 5.243569643749999010 ) ) ;
#26578 = CARTESIAN_POINT ( 'NONE',  ( 4.243569643749999898, 14.68437500061451750, 30.00000000000000000 ) ) ;
#26579 = CARTESIAN_POINT ( 'NONE',  ( 17.46562500061451217, 3.027376345333613106, -5.243569643749998122 ) ) ;
#26580 = CARTESIAN_POINT ( 'NONE',  ( 29.12812500061451715, 6.421520780324663323E-16, -5.243569643749999010 ) ) ;
#26581 = ORIENTED_EDGE ( 'NONE', *, *, #13122, .F. ) ;
#26582 = CARTESIAN_POINT ( 'NONE',  ( 22.34999999999999787, 0.000000000000000000, 4.999999999999998224 ) ) ;
#26583 = CARTESIAN_POINT ( 'NONE',  ( 9.001249775931846008E-16, 18.62187500061451928, -25.09994784771203058 ) ) ;
#26584 = CARTESIAN_POINT ( 'NONE',  ( 3.999999999999999112, 18.08750000122903501, 30.00000000000000000 ) ) ;
#26585 = CARTESIAN_POINT ( 'NONE',  ( 25.56562500061452070, 3.027376345333613106, -5.243569643749998122 ) ) ;
#26586 = CARTESIAN_POINT ( 'NONE',  ( 6.553125000614518747, -4.541064518000417216, -2.621784821875001281 ) ) ;
#26587 = CARTESIAN_POINT ( 'NONE',  ( 18.00000000122903288, -2.886751345948129988, 4.999999999999997335 ) ) ;
#26588 = CARTESIAN_POINT ( 'NONE',  ( 22.22812500061451502, -4.541064518000419881, 2.621784821874995952 ) ) ;
#26589 = CARTESIAN_POINT ( 'NONE',  ( 22.23750000000000071, 5.773502691896255534, 3.535250795749688894E-16 ) ) ;
#26590 = CARTESIAN_POINT ( 'NONE',  ( 28.15312500061451573, -4.541064518000417216, -2.621784821875001281 ) ) ;
#26591 = CARTESIAN_POINT ( 'NONE',  ( 7.978125000614517681, 6.421520780324663323E-16, -5.243569643749999010 ) ) ;
#26592 = VERTEX_POINT ( 'NONE', #54537 ) ;
#26593 = CARTESIAN_POINT ( 'NONE',  ( 23.99062500061451786, -3.027376345333614438, 5.243569643749998122 ) ) ;
#26594 = CARTESIAN_POINT ( 'NONE',  ( 3.478125000614517237, 6.421520780324663323E-16, -5.243569643749999010 ) ) ;
#26595 = AXIS2_PLACEMENT_3D ( 'NONE', #21560, #48922, #44114 ) ;
#26596 = CARTESIAN_POINT ( 'NONE',  ( 12.45937500061451786, -4.119189519843965641, -2.378215178125001383 ) ) ;
#26597 = DIRECTION ( 'NONE',  ( -0.000000000000000000, -1.000000000000000000, -0.000000000000000000 ) ) ;
#26598 = CARTESIAN_POINT ( 'NONE',  ( 2.000000000000001332, 14.41250000122903430, -26.53589838486224650 ) ) ;
#26599 = AXIS2_PLACEMENT_3D ( 'NONE', #45173, #11908, #51073 ) ;
#26600 = EDGE_CURVE ( 'NONE', #53550, #42330, #63102, .T. ) ;
#26601 = CARTESIAN_POINT ( 'NONE',  ( 10.42500000000000071, 6.123233995736764310E-16, -4.999999999999998224 ) ) ;
#26603 = CARTESIAN_POINT ( 'NONE',  ( 10.54687500061451644, -3.027376345333614438, 5.243569643749998122 ) ) ;
#26602 = CIRCLE ( 'NONE', #65506, 9.000000000000000000 ) ;
#26604 = CARTESIAN_POINT ( 'NONE',  ( 5.475000001229035185, -5.773502691896255534, -1.060575238724906372E-15 ) ) ;
#26605 = CARTESIAN_POINT ( 'NONE',  ( 14.22187500061451537, -6.054752690667223547, -1.112240025338166033E-15 ) ) ;
#26606 = CARTESIAN_POINT ( 'NONE',  ( 4.996875000614516615, 6.054752690667223547, 3.707466751127219781E-16 ) ) ;
#26607 = CARTESIAN_POINT ( 'NONE',  ( 16.87500000000000000, 4.330127018922191873, 2.499999999999999556 ) ) ;
#26608 = CIRCLE ( 'NONE', #43165, 1.500000000000000444 ) ;
#26609 = CARTESIAN_POINT ( 'NONE',  ( 30.00000000000000000, 0.000000000000000000, 4.999999999999998224 ) ) ;
#26610 = CARTESIAN_POINT ( 'NONE',  ( 13.24687500061451750, -3.027376345333614438, 5.243569643749998122 ) ) ;
#26611 = CARTESIAN_POINT ( 'NONE',  ( 6.262500001229034829, 0.000000000000000000, 4.999999999999998224 ) ) ;
#26612 = EDGE_CURVE ( 'NONE', #37421, #9597, #65923, .T. ) ;
#26613 = CARTESIAN_POINT ( 'NONE',  ( 22.94062500061451715, 6.054752690667223547, 3.707466751127219781E-16 ) ) ;
#26614 = CARTESIAN_POINT ( 'NONE',  ( -4.243569643749999898, 10.37187500061451750, 27.54997392385601529 ) ) ;
#26615 = CARTESIAN_POINT ( 'NONE',  ( 4.243569643749999010, 19.61562500061459602, 27.54997392385601174 ) ) ;
#26616 = CARTESIAN_POINT ( 'NONE',  ( 23.74687500061451573, -3.027376345333610441, -5.243569643749999898 ) ) ;
#26617 = CARTESIAN_POINT ( 'NONE',  ( -1.071796769724491005, 13.72009619066136921, -34.00000000000000000 ) ) ;
#26618 = CARTESIAN_POINT ( 'NONE',  ( 5.540625000614515905, -3.027376345333614438, 5.243569643749998122 ) ) ;
#26619 = CARTESIAN_POINT ( 'NONE',  ( 19.39687500061451786, 0.000000000000000000, 4.756430356249998326 ) ) ;
#26620 = CARTESIAN_POINT ( 'NONE',  ( 23.91562500061451502, 3.027376345333611329, 5.243569643749999010 ) ) ;
#26621 = CARTESIAN_POINT ( 'NONE',  ( 18.32812500061451644, 6.421520780324663323E-16, -5.243569643749999010 ) ) ;
#26622 = CARTESIAN_POINT ( 'NONE',  ( 14.19375000122903074, 5.773502691896255534, 3.535250795749688894E-16 ) ) ;
#26623 = CARTESIAN_POINT ( 'NONE',  ( 15.23437500061451644, 6.421520780324663323E-16, -5.243569643749999010 ) ) ;
#26624 = CARTESIAN_POINT ( 'NONE',  ( -1.071796769724496334, 15.78259618943233455, 26.00000000000000355 ) ) ;
#26625 = CARTESIAN_POINT ( 'NONE',  ( 27.90000000122903145, -2.886751345948129988, 4.999999999999997335 ) ) ;
#26626 = CARTESIAN_POINT ( 'NONE',  ( 7.134375000614516793, 6.421520780324663323E-16, -5.243569643749999010 ) ) ;
#26627 = CARTESIAN_POINT ( 'NONE',  ( 17.55937500061451573, 4.541064518000418104, -2.621784821874998173 ) ) ;
#26628 = CARTESIAN_POINT ( 'NONE',  ( -1.626862140677534273E-15, 17.73124999877096641, 34.00000000000000000 ) ) ;
#26629 = CARTESIAN_POINT ( 'NONE',  ( 23.58749999999999858, 5.773502691896255534, 3.535250795749688894E-16 ) ) ;
#26630 = CARTESIAN_POINT ( 'NONE',  ( 3.037500001229032964, 4.330127018922191873, 2.499999999999999556 ) ) ;
#26631 = CARTESIAN_POINT ( 'NONE',  ( 24.19687500061451857, -3.027376345333610441, -5.243569643749999898 ) ) ;
#26632 = CARTESIAN_POINT ( 'NONE',  ( 16.02187500061451786, -6.054752690667223547, -1.112240025338166033E-15 ) ) ;
#26633 = CARTESIAN_POINT ( 'NONE',  ( -1.878215178124999163, 13.35312499938548392, 26.74683588394047007 ) ) ;
#26634 = CARTESIAN_POINT ( 'NONE',  ( 27.00000000000000000, -4.330127018922190985, -2.500000000000001332 ) ) ;
#26635 = ADVANCED_FACE ( 'NONE', ( #25730 ), #54901, .T. ) ;
#26636 = CARTESIAN_POINT ( 'NONE',  ( 7.500000000000000000, 0.000000000000000000, 4.999999999999998224 ) ) ;
#26637 = CARTESIAN_POINT ( 'NONE',  ( 8.934375000614515727, 5.492252693125287522, 3.363034840372157021E-16 ) ) ;
#26638 = CARTESIAN_POINT ( 'NONE',  ( 20.09062500061451573, -3.027376345333610441, -5.243569643749999898 ) ) ;
#26639 = CARTESIAN_POINT ( 'NONE',  ( 9.937500000000001776, -2.886751345948125991, -5.000000000000000000 ) ) ;
#26640 = CARTESIAN_POINT ( 'NONE',  ( 3.140625000614516882, 6.054752690667223547, 3.707466751127219781E-16 ) ) ;
#26641 = CARTESIAN_POINT ( 'NONE',  ( 20.32499999999999929, 6.123233995736764310E-16, -4.999999999999998224 ) ) ;
#26642 = CARTESIAN_POINT ( 'NONE',  ( 1.138803498474273873E-14, 16.38124999877096499, 34.00000000000000000 ) ) ;
#26643 = CARTESIAN_POINT ( 'NONE',  ( 22.01250000122903216, 0.000000000000000000, 4.999999999999998224 ) ) ;
#26644 = CARTESIAN_POINT ( 'NONE',  ( 50.00000000000000000, -8.875000000000000000, -1.494782592887675232 ) ) ;
#26645 = CARTESIAN_POINT ( 'NONE',  ( 28.92187500061451644, 3.027376345333611329, 5.243569643749999010 ) ) ;
#26646 = AXIS2_PLACEMENT_3D ( 'NONE', #8755, #51563, #62636 ) ;
#26647 = ORIENTED_EDGE ( 'NONE', *, *, #43096, .F. ) ;
#26648 = CARTESIAN_POINT ( 'NONE',  ( 16.60312500061451857, 4.541064518000418104, -2.621784821874998173 ) ) ;
#26649 = CARTESIAN_POINT ( 'NONE',  ( 23.95312500061451289, 0.000000000000000000, 5.243569643749999010 ) ) ;
#26650 = CARTESIAN_POINT ( 'NONE',  ( 24.19687500061451857, -3.027376345333610441, -5.243569643749999898 ) ) ;
#26651 = CARTESIAN_POINT ( 'NONE',  ( 9.825000000000001066, -4.330127018922194537, 2.499999999999995559 ) ) ;
#26652 = CARTESIAN_POINT ( 'NONE',  ( 11.91562500061451857, -6.054752690667223547, -1.112240025338166033E-15 ) ) ;
#26653 = CARTESIAN_POINT ( 'NONE',  ( 27.66562500061451146, -6.054752690667223547, -1.112240025338166033E-15 ) ) ;
#26654 = CARTESIAN_POINT ( 'NONE',  ( 15.08437500061451786, -4.541064518000419881, 2.621784821874995952 ) ) ;
#26655 = CARTESIAN_POINT ( 'NONE',  ( 19.88437500061451857, 4.541064518000418104, 2.621784821874999949 ) ) ;
#26656 = CARTESIAN_POINT ( 'NONE',  ( 4.648177544792955741E-15, 14.58124999877096606, 33.99999999999999289 ) ) ;
#26657 = CARTESIAN_POINT ( 'NONE',  ( -3.000416591977282496E-16, 10.74687500061451928, 25.09994784771203058 ) ) ;
#26658 = EDGE_CURVE ( 'NONE', #54979, #8125, #9104, .T. ) ;
#26659 = CARTESIAN_POINT ( 'NONE',  ( 22.72500000122903430, 2.886751345948129099, -4.999999999999998224 ) ) ;
#26660 = CARTESIAN_POINT ( 'NONE',  ( 16.77187500061451786, 2.746126346562643317, 4.756430356249998326 ) ) ;
#26661 = CARTESIAN_POINT ( 'NONE',  ( 13.97812500061451679, 4.541064518000418104, 2.621784821874999949 ) ) ;
#26662 = CARTESIAN_POINT ( 'NONE',  ( 7.059375000614518392, -4.541064518000417216, -2.621784821875001281 ) ) ;
#26663 = CARTESIAN_POINT ( 'NONE',  ( 8.371875000614515727, -6.054752690667223547, -1.112240025338166033E-15 ) ) ;
#26664 = ORIENTED_EDGE ( 'NONE', *, *, #48794, .F. ) ;
#26665 = CARTESIAN_POINT ( 'NONE',  ( 26.74687500061451573, -3.027376345333614438, 5.243569643749998122 ) ) ;
#26666 = CARTESIAN_POINT ( 'NONE',  ( 20.35312500061451502, 0.000000000000000000, 5.243569643749999010 ) ) ;
#26667 =( BOUNDED_SURFACE ( )  B_SPLINE_SURFACE ( 1, 2, ( 
 ( #42956, #42592, #13396, #30414, #8243, #41497, #59937, #31876, #64385, #8606, #2339, #9344, #31135, #2703, #52941, #65117, #35943, #25599, #54411, #70661, #53303, #26333, #53676, #3446, #47765, #20036, #37041, #65485, #24856, #20408, #14875, #31511, #25965, #59565, #14508, #54052, #47402, #71033, #58465, #19303, #37414, #3811, #30773, #25219, #48872, #13776, #19673, #36317, #64751, #58833, #70301, #42227, #7877, #14142, #36677, #18938, #3070, #43333, #27800, #27435, #72860, #37774, #66588, #71774, #56233, #66218, #33689, #16330, #55144, #44435, #65855, #61039, #5627, #38138, #22244, #60293, #38885, #71402, #15965, #4542, #26706, #21875, #27071, #21143, #50337, #43697, #44798, #10797, #28163, #20776, #9704, #32238, #15595, #15237, #60661, #10075, #44061, #10437, #49602, #4177, #55870, #38516, #32606, #5257, #39248, #72129, #21508, #32967, #55507, #72489, #61402, #4900, #49966, #54772, #49240, #66965, #33332, #67331, #16691, #61761, #11165, #51774, #57663, #93, #58018, #56937, #29241, #51050, #63210, #45151, #22956, #45516, #56585, #447, #5982, #7069, #67683, #17054, #1174, #46230, #29598, #34409, #7427, #39612, #12961, #34046, #40325, #46594, #28512, #23682, #68047, #17416, #68769, #52134, #40692, #1537, #6342, #17766, #39974, #62487, #62132, #28873, #18126, #12606, #11524, #35139, #24045, #11884, #51412, #69136, #12240, #18495, #814, #23322, #45871, #41060, #63574, #62847, #50691, #35498, #22599, #68404, #34772, #57304, #6709, #71956, #43885, #52858, #71216, #13317, #21332, #20593, #13687, #41416, #54596, #52494, #37599, #66411, #9530, #64299, #38329, #43150, #15420, #59756, #32063, #49063, #54963, #63932, #30328, #20965, #3999, #69495, #1905, #26525, #35856, #43519, #37963, #48693, #71591, #7790, #58379, #66042, #36231, #65673, #15062, #3630, #60485, #2258, #18854, #4368, #9891, #26898, #9163, #32427, #60120, #24772, #15788, #49423, #60858, #29954, #24410, #46959, #47316, #69849, #19216, #41770, #31698, #54233, #26152, #61229, #61951, #10261, #16515, #10623, #33153, #73045, #32793, #68235, #72685, #72316, #11713, #67155, #40158, #22783, #27987, #39068, #28697, #61582, #11355, #33506, #56055, #4724, #39430, #10985, #34230, #27621, #33873, #55330, #49791, #27258, #5447, #21697, #50517, #22427, #50155, #56764, #56416, #44254, #66785, #22067, #16158, #51236, #23148, #55690, #44974, #38710, #639, #67512, #16876, #5086, #5807, #44626, #28338, #45702, #50875, #273, #17599, #45335, #67870, #17242, #39802, #62318, #6168, #23510, #63032, #52678, #63754, #29067, #12073, #13143, #46059, #2086, #47143, #7255, #35683, #40517, #68593, #41242, #46419, #1722, #29783, #35323, #69674, #12431, #51603, #13502, #58205, #36049, #68957, #19040, #46784, #34965, #24957, #58570, #30513, #41598, #7977, #53040, #7609, #17955, #57492, #24595, #64117, #18679, #6896, #29427, #30146, #62678, #18314, #51963, #1362, #52319, #34595, #47501, #23871, #1003, #2435, #40885, #19405, #70032, #24234, #63401, #57123, #12786, #6534, #57845, #69319, #36417, #71129, #48237, #65955, #59294, #43059, #13878, #8340, #58933, #65214, #71871, #42692, #70762, #8704, #9076, #31237, #19777, #30869, #20137, #60033, #37512, #53408, #31972, #65584, #47873, #42327, #15335, #3542, #54508, #3174, #14604, #37140, #60395, #9803, #31612, #41963, #25327, #54148, #37875, #70401, #14974, #64852, #53778, #9444, #71503, #3911, #20879, #25701, #43433, #32336, #26433, #48974, #54874, #4279, #48604, #14240, #26805, #2800, #36778, #49339, #64485, #59668, #26065, #20502, #32709, #21979, #66696, #67069, #44166, #50066, #21611, #10174, #16068, #15699, #33791, #61863, #66322, #50790, #50435, #22698, #60767, #16427, #38618, #6082, #61142, #56683, #39349, #5000, #67430, #38238, #10897, #28614, #10537, #45250, #55246, #11269, #21243, #38985, #27533, #49705, #44894, #72596, #33065, #193, #55604, #67783, #56334, #51151, #43796, #4641, #27171, #44538, #72233, #61500, #33425, #55967, #5362, #27900, #72960, #5724, #22342, #16792, #28259, #62234, #17157, #39716, #11630, #34146, #1638, #41159, #6807, #7168, #62590, #17514, #45617, #35959, #28979, #18595, #47056, #23781, #24144, #7524, #23062, #7891, #29341, #52234, #916, #13058, #68151, #45971, #68505, #6444, #23425, #51517, #30057, #40075, #11986, #46697, #69233, #52595, #57402, #30427, #34509, #58480, #18223, #51873, #18952, #1272, #63668, #46333, #68867, #57038, #29696, #40797, #24512, #17868, #35597, #40427, #62944, #12338, #63310, #552, #12701, #35238, #34873, #57759, #58116, #2002, #69590, #41512, #64031, #13410, #69946, #42967, #54062, #58846, #30786, #3823, #14519, #65497, #14154, #3082, #8618, #71413, #20789, #42603, #52955, #26344, #3458, #47416, #64399, #42240, #2352, #43345, #65867, #2716, #20048, #36332, #15249, #65129, #36688, #13791, #25978, #24869, #59577, #37786, #31522, #59210, #60306, #37052, #37425, #31147, #48517, #71044, #48883, #8256, #53317, #14886, #20419, #19316, #41870, #59948, #25232, #9355, #31888, #70673, #54423, #47778, #70313, #9717, #53688, #8990, #19686, #25610, #64764, #48148, #71786, #56247, #55881, #5638, #15977, #61772, #16341, #4553, #67693, #28175, #105, #11176, #50702, #22610, #50348, #38150, #27082, #22255, #33700, #61415, #55156, #10087, #10808, #32250, #38527, #32617, #49613, #21890, #54783, #17065, #21519, #21154, #45162, #61049, #62143, #44809, #39625, #10449, #4189, #38896, #72140, #26718, #49251, #43708, #66229, #15608, #60673, #72872, #44074, #66603, #67342, #32978, #33343, #55518, #4911, #5269, #27447, #49977, #72501, #44447, #66976, #27814, #16703, #39260, #459, #12972, #68415, #41427, #24058, #29253, #17777, #29965, #40336, #12617, #34783, #57316, #5993, #40704, #62858, #35510, #28885, #35151, #56597, #51062, #28523, #6720, #11537, #12252 ),
 ( #22967, #51785, #56949, #1185, #34421, #23693, #11896, #45528, #6353, #68059, #46604, #52145, #17426, #41071, #63222, #58029, #39986, #46241, #51424, #69506, #825, #46970, #29609, #68781, #57674, #62498, #18137, #18866, #23333, #7439, #45883, #1548, #34057, #7080, #69147, #18506, #63585, #52506, #1917, #24421, #36242, #37340, #3372, #71324, #13328, #30340, #24782, #58756, #58390, #64309, #13699, #36602, #2991, #47685, #69859, #42151, #25519, #65043, #31434, #70221, #70589, #52868, #7803, #35867, #26259, #19226, #8902, #59863, #14063, #14433, #70958, #2267, #20699, #19595, #42517, #8166, #25893, #47326, #30695, #53226, #41780, #2623, #25144, #20331, #64678, #59123, #36968, #59490, #42884, #8530, #63943, #31059, #48796, #53596, #48064, #9267, #19964, #53974, #48433, #65407, #14797, #31802, #54340, #3734, #26999, #44722, #39170, #33257, #50261, #61327, #16257, #49890, #49168, #27723, #9632, #71699, #10725, #38812, #55068, #49529, #72415, #54699, #43989, #15522, #15891, #66144, #72053, #43622, #32166, #38064, #37697, #55795, #5185, #15160, #72786, #21797, #67257, #4104, #38437, #60588, #28089, #9997, #5551, #22169, #21432, #16615, #60219, #32893, #50617, #32532, #61686, #26631, #11085, #43257, #60963, #66510, #21071, #66889, #10362, #4469, #33613, #55433, #56157, #22, #65778, #4825, #27359, #44362, #17344, #16977, #22880, #45438, #68336, #34698, #6270, #28440, #6997, #17696, #39903, #29528, #63504, #23250, #62416, #39534, #12534, #23613, #50975, #372, #46521, #57227, #35068, #56865, #45800, #51339, #40988, #12891, #12170, #22528, #69062, #46159, #62059, #33974, #11815, #45075, #35424, #57948, #67971, #62778, #5906, #7356, #6642, #28798, #56513, #68699, #67611, #29169, #29885, #1106, #741, #52423, #51703, #52063, #40257, #18059, #40619, #18422, #34332, #63139, #57594, #1467, #11453, #23973, #25437, #58307, #14350, #59403, #19513, #47980, #52785, #7718, #53512, #58674, #13980, #42071, #47605, #8812, #24700, #41346, #25809, #70508, #48347, #8084, #31349, #59039, #47244, #37253, #70872, #42798, #53890, #20246, #65320, #19884, #30252, #69776, #64959, #3281, #30979, #19144, #2186, #2906, #1829, #30614, #41698, #64222, #64592, #24338, #59775, #13611, #63856, #14710, #53144, #31716, #36885, #36519, #2543, #9181, #25062, #42437, #70135, #8443, #69424, #46886, #18781, #13246, #36156, #35784, #3648, #71234, #26171, #37980, #5103, #60502, #43537, #26541, #54981, #49082, #60137, #20613, #66058, #60875, #10279, #4742, #9908, #4017, #27276, #38726, #15436, #54611, #32445, #49441, #66428, #32810, #4386, #21348, #43172, #48712, #65691, #10641, #37615, #55348, #44272, #26916, #43904, #49809, #15078, #55709, #71975, #15806, #9546, #72334, #32080, #71611, #20984, #38347, #21714, #66804, #16175, #61247, #33171, #54251, #36324, #23774, #58472, #35591, #53310, #46690, #30420, #1267, #68861, #46326, #52588, #59204, #30048, #58110, #69227, #69583, #18588, #7161, #18217, #7517, #47409, #24862, #40791, #19309, #52948, #35232, #29690, #2709, #64024, #41862, #63661, #1994, #24505, #47771, #70307, #18945, #29335, #25225, #2345, #63303, #12695, #41153, #51865, #19680, #42233, #52227, #41504, #57753, #64758, #13403, #13052, #1631, #69939, #24138, #35951, #14148, #7884, #47049, #36683, #64392, #13782, #58839, #8249, #30779, #32612, #42598, #8985, #71781, #9711, #48143, #31141, #32245, #65124, #21149, #66224, #26339, #54778, #59572, #14514, #60300, #65491, #20783, #48878, #54417, #15603, #31517, #70667, #55150, #4184, #38144, #43703, #60668, #14881, #10082, #4548, #27077, #49608, #26712, #49246, #15243, #37047, #72135, #20043, #54058, #21515, #44069, #20414, #37420, #37780, #3453, #9350, #25971, #3818, #48512, #59943, #71039, #42962, #31883, #3077, #66596, #15972, #53682, #38522, #8612, #25605, #71408, #43339, #65861, #45878, #55876, #23328, #5988, #44804, #34052, #55513, #50697, #68410, #27809, #62493, #49972, #28518, #61045, #5633, #67337, #16336, #11532, #16697, #61409, #39981, #33338, #34416, #453, #17772, #10443, #27442, #21882, #5263, #4906, #10803, #50343, #33695, #99, #39255, #66971, #45523, #56242, #72867, #68053, #28879, #61767, #22250, #11171, #11891, #56944, #51419, #51058, #38891, #28170, #22962, #17422, #17060, #22605, #45157, #39620, #32973, #67689, #62138, #56592, #6348, #72497, #44442, #820, #29248, #41776, #24053, #70217, #52864, #58024, #46600, #58752, #19222, #63580, #7434, #47322, #34778, #69501, #69142, #64305, #57669, #41422, #12247, #6715, #57311, #12967, #40332, #41066, #18501, #40699, #13695, #12612, #36238, #2264, #47681, #62853, #51780, #1180, #35146, #23688, #63217, #7075, #35505, #52501, #29960, #46236, #24778, #1912, #29604, #69855, #8162, #68776, #18132, #1543, #52140, #63938, #7798, #24416, #46965, #18861, #13323, #35862, #2619, #58385, #30336, #30691, #53222, #25140, #26626, #42147, #26995, #25888, #71318, #19961, #32161, #14059, #65037, #14428, #25515, #42513, #48060, #49163, #36598, #64674, #49524, #20694, #20325, #3367, #19591, #59119, #55064, #2987, #9262, #15517, #70585, #43253, #36963, #59485, #37692, #71694, #9628, #21066, #48428, #43617, #38059, #54694, #66139, #60215, #65773, #26254, #8897, #4097, #8526, #31429, #60584, #15155, #53969, #70954, #48791, #31055, #42879, #65402, #14793, #37335, #59858, #31797, #53592, #54335, #3729, #9992, #32527, #4465, #28434, #28084, #367, #38432, #67252, #72410, #56859, #66884, #34327, #16972, #55790, #45070, #66505, #61681, #6265, #38807, #22875, #60956, #39528, #72049, #16610, #5180, #27354, #22523, #28793, #55428, #11080, #67966, #49885, #16, #4820, #61322, #62054, #50971, #11449, #45432, #27717, #17339, #39898, #33969, #5901, #56508, #67607, #5546, #21792, #62411, #10358, #44358, #11810, #21427, #10720 ) ),
 .UNSPECIFIED., .F., .F., .F. ) 
 B_SPLINE_SURFACE_WITH_KNOTS ( ( 2, 2 ),
 ( 3, 2, 2, 2, 2, 2, 2, 2, 2, 2, 2, 2, 2, 2, 2, 2, 2, 2, 2, 2, 2, 2, 2, 2, 2, 2, 2, 2, 2, 2, 2, 2, 2, 2, 2, 2, 2, 2, 2, 2, 2, 2, 2, 2, 2, 2, 2, 2, 2, 2, 2, 2, 2, 2, 2, 2, 2, 2, 2, 2, 2, 2, 2, 2, 2, 2, 2, 2, 2, 2, 2, 2, 2, 2, 2, 2, 2, 2, 2, 2, 2, 2, 2, 2, 2, 2, 2, 2, 2, 2, 2, 2, 2, 2, 2, 2, 2, 2, 2, 2, 2, 2, 2, 2, 2, 2, 2, 2, 2, 2, 2, 2, 2, 2, 2, 2, 2, 2, 2, 2, 2, 2, 2, 2, 2, 2, 2, 2, 2, 2, 2, 2, 2, 2, 2, 2, 2, 2, 2, 2, 2, 2, 2, 2, 2, 2, 2, 2, 2, 2, 2, 2, 2, 2, 2, 2, 2, 2, 2, 2, 2, 2, 2, 2, 2, 2, 2, 2, 2, 2, 2, 2, 2, 2, 2, 2, 2, 2, 2, 2, 2, 2, 2, 2, 2, 2, 2, 2, 2, 2, 2, 2, 2, 2, 2, 2, 2, 2, 2, 2, 2, 2, 2, 2, 2, 2, 2, 2, 2, 2, 2, 2, 2, 2, 2, 2, 2, 2, 2, 2, 2, 2, 2, 2, 2, 2, 2, 2, 2, 2, 2, 2, 2, 2, 2, 2, 2, 2, 2, 2, 2, 2, 2, 2, 2, 2, 2, 2, 2, 2, 2, 2, 2, 2, 2, 2, 2, 2, 2, 2, 2, 2, 2, 2, 2, 2, 2, 2, 2, 2, 2, 2, 2, 2, 2, 2, 2, 2, 2, 2, 2, 2, 2, 2, 2, 2, 2, 2, 2, 2, 2, 2, 2, 2, 2, 2, 2, 2, 2, 2, 2, 2, 2, 2, 2, 2, 2, 2, 2, 2, 2, 2, 2, 2, 2, 2, 2, 2, 2, 2, 2, 2, 2, 2, 2, 2, 2, 2, 2, 2, 2, 2, 2, 2, 2, 2, 2, 2, 2, 2, 2, 2, 2, 2, 2, 2, 2, 2, 2, 2, 2, 2, 2, 2, 2, 2, 2, 2, 2, 2, 3 ),
 ( 0.000000000000000000, 1.000000000000000000 ),
 ( 0.000000000000000000, 0.002777777777777777884, 0.005555555555555555768, 0.008333333333333333218, 0.01111111111111111154, 0.01388888888888888812, 0.01666666666666666644, 0.01944444444444444475, 0.02222222222222222307, 0.02500000000000000139, 0.02777777777777777624, 0.03055555555555555455, 0.03333333333333333287, 0.03611111111111110772, 0.03888888888888888951, 0.04166666666666666435, 0.04444444444444444614, 0.04722222222222222099, 0.05000000000000000278, 0.05277777777777777762, 0.05555555555555555247, 0.05833333333333333426, 0.06111111111111110911, 0.06388888888888888395, 0.06666666666666666574, 0.06944444444444444753, 0.07222222222222221544, 0.07499999999999999722, 0.07777777777777777901, 0.08055555555555556080, 0.08333333333333332871, 0.08611111111111111049, 0.08888888888888889228, 0.09166666666666666019, 0.09444444444444444198, 0.09722222222222222376, 0.1000000000000000056, 0.1027777777777777735, 0.1055555555555555552, 0.1083333333333333370, 0.1111111111111111049, 0.1138888888888888867, 0.1166666666666666685, 0.1194444444444444503, 0.1222222222222222182, 0.1250000000000000000, 0.1277777777777777679, 0.1305555555555555636, 0.1333333333333333315, 0.1361111111111110994, 0.1388888888888888951, 0.1416666666666666630, 0.1444444444444444309, 0.1472222222222222265, 0.1499999999999999944, 0.1527777777777777901, 0.1555555555555555580, 0.1583333333333333259, 0.1611111111111111216, 0.1638888888888888895, 0.1666666666666666574, 0.1694444444444444531, 0.1722222222222222210, 0.1749999999999999889, 0.1777777777777777846, 0.1805555555555555525, 0.1833333333333333204, 0.1861111111111111160, 0.1888888888888888840, 0.1916666666666666796, 0.1944444444444444475, 0.1972222222222222154, 0.2000000000000000111, 0.2027777777777777790, 0.2055555555555555469, 0.2083333333333333426, 0.2111111111111111105, 0.2138888888888888784, 0.2166666666666666741, 0.2194444444444444420, 0.2222222222222222099, 0.2250000000000000056, 0.2277777777777777735, 0.2305555555555555691, 0.2333333333333333370, 0.2361111111111111049, 0.2388888888888889006, 0.2416666666666666685, 0.2444444444444444364, 0.2472222222222222321, 0.2500000000000000000, 0.2527777777777777679, 0.2555555555555555358, 0.2583333333333333592, 0.2611111111111111271, 0.2638888888888888951, 0.2666666666666666630, 0.2694444444444444309, 0.2722222222222221988, 0.2750000000000000222, 0.2777777777777777901, 0.2805555555555555580, 0.2833333333333333259, 0.2861111111111110938, 0.2888888888888888618, 0.2916666666666666852, 0.2944444444444444531, 0.2972222222222222210, 0.2999999999999999889, 0.3027777777777777568, 0.3055555555555555802, 0.3083333333333333481, 0.3111111111111111160, 0.3138888888888888840, 0.3166666666666666519, 0.3194444444444444198, 0.3222222222222222432, 0.3250000000000000111, 0.3277777777777777790, 0.3305555555555555469, 0.3333333333333333148, 0.3361111111111111382, 0.3388888888888889062, 0.3416666666666666741, 0.3444444444444444420, 0.3472222222222222099, 0.3499999999999999778, 0.3527777777777778012, 0.3555555555555555691, 0.3583333333333333370, 0.3611111111111111049, 0.3638888888888888729, 0.3666666666666666408, 0.3694444444444444642, 0.3722222222222222321, 0.3750000000000000000, 0.3777777777777777679, 0.3805555555555555358, 0.3833333333333333592, 0.3861111111111111271, 0.3888888888888888951, 0.3916666666666666630, 0.3944444444444444309, 0.3972222222222221988, 0.4000000000000000222, 0.4027777777777777901, 0.4055555555555555580, 0.4083333333333333259, 0.4111111111111110938, 0.4138888888888888618, 0.4166666666666666852, 0.4194444444444444531, 0.4222222222222222210, 0.4249999999999999889, 0.4277777777777777568, 0.4305555555555555802, 0.4333333333333333481, 0.4361111111111111160, 0.4388888888888888840, 0.4416666666666666519, 0.4444444444444444198, 0.4472222222222222432, 0.4500000000000000111, 0.4527777777777777790, 0.4555555555555555469, 0.4583333333333333148, 0.4611111111111111382, 0.4638888888888889062, 0.4666666666666666741, 0.4694444444444444420, 0.4722222222222222099, 0.4749999999999999778, 0.4777777777777778012, 0.4805555555555555691, 0.4833333333333333370, 0.4861111111111111049, 0.4888888888888888729, 0.4916666666666666408, 0.4944444444444444642, 0.4972222222222222321, 0.5000000000000000000, 0.5027777777777777679, 0.5055555555555555358, 0.5083333333333333037, 0.5111111111111110716, 0.5138888888888888395, 0.5166666666666667185, 0.5194444444444444864, 0.5222222222222222543, 0.5250000000000000222, 0.5277777777777777901, 0.5305555555555555580, 0.5333333333333333259, 0.5361111111111110938, 0.5388888888888888618, 0.5416666666666666297, 0.5444444444444443976, 0.5472222222222222765, 0.5500000000000000444, 0.5527777777777778123, 0.5555555555555555802, 0.5583333333333333481, 0.5611111111111111160, 0.5638888888888888840, 0.5666666666666666519, 0.5694444444444444198, 0.5722222222222221877, 0.5749999999999999556, 0.5777777777777777235, 0.5805555555555556024, 0.5833333333333333703, 0.5861111111111111382, 0.5888888888888889062, 0.5916666666666666741, 0.5944444444444444420, 0.5972222222222222099, 0.5999999999999999778, 0.6027777777777777457, 0.6055555555555555136, 0.6083333333333332815, 0.6111111111111111605, 0.6138888888888889284, 0.6166666666666666963, 0.6194444444444444642, 0.6222222222222222321, 0.6250000000000000000, 0.6277777777777777679, 0.6305555555555555358, 0.6333333333333333037, 0.6361111111111110716, 0.6388888888888888395, 0.6416666666666667185, 0.6444444444444444864, 0.6472222222222222543, 0.6500000000000000222, 0.6527777777777777901, 0.6555555555555555580, 0.6583333333333333259, 0.6611111111111110938, 0.6638888888888888618, 0.6666666666666666297, 0.6694444444444443976, 0.6722222222222222765, 0.6750000000000000444, 0.6777777777777778123, 0.6805555555555555802, 0.6833333333333333481, 0.6861111111111111160, 0.6888888888888888840, 0.6916666666666666519, 0.6944444444444444198, 0.6972222222222221877, 0.6999999999999999556, 0.7027777777777777235, 0.7055555555555556024, 0.7083333333333333703, 0.7111111111111111382, 0.7138888888888889062, 0.7166666666666666741, 0.7194444444444444420, 0.7222222222222222099, 0.7249999999999999778, 0.7277777777777777457, 0.7305555555555555136, 0.7333333333333332815, 0.7361111111111111605, 0.7388888888888889284, 0.7416666666666666963, 0.7444444444444444642, 0.7472222222222222321, 0.7500000000000000000, 0.7527777777777777679, 0.7555555555555555358, 0.7583333333333333037, 0.7611111111111110716, 0.7638888888888888395, 0.7666666666666667185, 0.7694444444444444864, 0.7722222222222222543, 0.7750000000000000222, 0.7777777777777777901, 0.7805555555555555580, 0.7833333333333333259, 0.7861111111111110938, 0.7888888888888888618, 0.7916666666666666297, 0.7944444444444443976, 0.7972222222222222765, 0.8000000000000000444, 0.8027777777777778123, 0.8055555555555555802, 0.8083333333333333481, 0.8111111111111111160, 0.8138888888888888840, 0.8166666666666666519, 0.8194444444444444198, 0.8222222222222221877, 0.8249999999999999556, 0.8277777777777777235, 0.8305555555555556024, 0.8333333333333333703, 0.8361111111111111382, 0.8388888888888889062, 0.8416666666666666741, 0.8444444444444444420, 0.8472222222222222099, 0.8499999999999999778, 0.8527777777777777457, 0.8555555555555555136, 0.8583333333333332815, 0.8611111111111111605, 0.8638888888888889284, 0.8666666666666666963, 0.8694444444444444642, 0.8722222222222222321, 0.8750000000000000000, 0.8777777777777777679, 0.8805555555555555358, 0.8833333333333333037, 0.8861111111111110716, 0.8888888888888888395, 0.8916666666666667185, 0.8944444444444444864, 0.8972222222222222543, 0.9000000000000000222, 0.9027777777777777901, 0.9055555555555555580, 0.9083333333333333259, 0.9111111111111110938, 0.9138888888888888618, 0.9166666666666666297, 0.9194444444444443976, 0.9222222222222222765, 0.9250000000000000444, 0.9277777777777778123, 0.9305555555555555802, 0.9333333333333333481, 0.9361111111111111160, 0.9388888888888888840, 0.9416666666666666519, 0.9444444444444444198, 0.9472222222222221877, 0.9499999999999999556, 0.9527777777777777235, 0.9555555555555556024, 0.9583333333333333703, 0.9611111111111111382, 0.9638888888888889062, 0.9666666666666666741, 0.9694444444444444420, 0.9722222222222222099, 0.9749999999999999778, 0.9777777777777777457, 0.9805555555555555136, 0.9833333333333332815, 0.9861111111111111605, 0.9888888888888889284, 0.9916666666666666963, 0.9944444444444444642, 0.9972222222222222321, 1.000000000000000000 ),
 .UNSPECIFIED. ) 
 GEOMETRIC_REPRESENTATION_ITEM ( )  RATIONAL_B_SPLINE_SURFACE ( (
 ( 1.000000000000000000, 0.8660254037844387076, 1.000000000000000000, 0.8660254037844387076, 1.000000000000000000, 0.8660254037844387076, 1.000000000000000000, 0.8660254037844387076, 1.000000000000000000, 0.8660254037844387076, 1.000000000000000000, 0.8660254037844387076, 1.000000000000000000, 0.8660254037844387076, 1.000000000000000000, 0.8660254037844387076, 1.000000000000000000, 0.8660254037844387076, 1.000000000000000000, 0.8660254037844387076, 1.000000000000000000, 0.8660254037844387076, 1.000000000000000000, 0.8660254037844387076, 1.000000000000000000, 0.8660254037844387076, 1.000000000000000000, 0.8660254037844387076, 1.000000000000000000, 0.8660254037844387076, 1.000000000000000000, 0.8660254037844387076, 1.000000000000000000, 0.8660254037844387076, 1.000000000000000000, 0.8660254037844387076, 1.000000000000000000, 0.8660254037844387076, 1.000000000000000000, 0.8660254037844387076, 1.000000000000000000, 0.8660254037844387076, 1.000000000000000000, 0.8660254037844387076, 1.000000000000000000, 0.8660254037844387076, 1.000000000000000000, 0.8660254037844387076, 1.000000000000000000, 0.8660254037844387076, 1.000000000000000000, 0.8660254037844387076, 1.000000000000000000, 0.8660254037844387076, 1.000000000000000000, 0.8660254037844387076, 1.000000000000000000, 0.8660254037844387076, 1.000000000000000000, 0.8660254037844387076, 1.000000000000000000, 0.8660254037844387076, 1.000000000000000000, 0.8660254037844387076, 1.000000000000000000, 0.8660254037844387076, 1.000000000000000000, 0.8660254037844387076, 1.000000000000000000, 0.8660254037844387076, 1.000000000000000000, 0.8660254037844387076, 1.000000000000000000, 0.8660254037844387076, 1.000000000000000000, 0.8660254037844387076, 1.000000000000000000, 0.8660254037844387076, 1.000000000000000000, 0.8660254037844387076, 1.000000000000000000, 0.8660254037844387076, 1.000000000000000000, 0.8660254037844387076, 1.000000000000000000, 0.8660254037844387076, 1.000000000000000000, 0.8660254037844387076, 1.000000000000000000, 0.8660254037844387076, 1.000000000000000000, 0.8660254037844387076, 1.000000000000000000, 0.8660254037844387076, 1.000000000000000000, 0.8660254037844387076, 1.000000000000000000, 0.8660254037844387076, 1.000000000000000000, 0.8660254037844387076, 1.000000000000000000, 0.8660254037844387076, 1.000000000000000000, 0.8660254037844387076, 1.000000000000000000, 0.8660254037844387076, 1.000000000000000000, 0.8660254037844387076, 1.000000000000000000, 0.8660254037844387076, 1.000000000000000000, 0.8660254037844387076, 1.000000000000000000, 0.8660254037844387076, 1.000000000000000000, 0.8660254037844387076, 1.000000000000000000, 0.8660254037844387076, 1.000000000000000000, 0.8660254037844387076, 1.000000000000000000, 0.8660254037844387076, 1.000000000000000000, 0.8660254037844387076, 1.000000000000000000, 0.8660254037844387076, 1.000000000000000000, 0.8660254037844387076, 1.000000000000000000, 0.8660254037844387076, 1.000000000000000000, 0.8660254037844387076, 1.000000000000000000, 0.8660254037844387076, 1.000000000000000000, 0.8660254037844387076, 1.000000000000000000, 0.8660254037844387076, 1.000000000000000000, 0.8660254037844387076, 1.000000000000000000, 0.8660254037844387076, 1.000000000000000000, 0.8660254037844387076, 1.000000000000000000, 0.8660254037844387076, 1.000000000000000000, 0.8660254037844387076, 1.000000000000000000, 0.8660254037844387076, 1.000000000000000000, 0.8660254037844387076, 1.000000000000000000, 0.8660254037844387076, 1.000000000000000000, 0.8660254037844387076, 1.000000000000000000, 0.8660254037844387076, 1.000000000000000000, 0.8660254037844387076, 1.000000000000000000, 0.8660254037844387076, 1.000000000000000000, 0.8660254037844387076, 1.000000000000000000, 0.8660254037844387076, 1.000000000000000000, 0.8660254037844387076, 1.000000000000000000, 0.8660254037844387076, 1.000000000000000000, 0.8660254037844387076, 1.000000000000000000, 0.8660254037844387076, 1.000000000000000000, 0.8660254037844387076, 1.000000000000000000, 0.8660254037844387076, 1.000000000000000000, 0.8660254037844387076, 1.000000000000000000, 0.8660254037844387076, 1.000000000000000000, 0.8660254037844387076, 1.000000000000000000, 0.8660254037844387076, 1.000000000000000000, 0.8660254037844387076, 1.000000000000000000, 0.8660254037844387076, 1.000000000000000000, 0.8660254037844387076, 1.000000000000000000, 0.8660254037844387076, 1.000000000000000000, 0.8660254037844387076, 1.000000000000000000, 0.8660254037844387076, 1.000000000000000000, 0.8660254037844387076, 1.000000000000000000, 0.8660254037844387076, 1.000000000000000000, 0.8660254037844387076, 1.000000000000000000, 0.8660254037844387076, 1.000000000000000000, 0.8660254037844387076, 1.000000000000000000, 0.8660254037844387076, 1.000000000000000000, 0.8660254037844387076, 1.000000000000000000, 0.8660254037844387076, 1.000000000000000000, 0.8660254037844387076, 1.000000000000000000, 0.8660254037844387076, 1.000000000000000000, 0.8660254037844387076, 1.000000000000000000, 0.8660254037844387076, 1.000000000000000000, 0.8660254037844387076, 1.000000000000000000, 0.8660254037844387076, 1.000000000000000000, 0.8660254037844387076, 1.000000000000000000, 0.8660254037844387076, 1.000000000000000000, 0.8660254037844387076, 1.000000000000000000, 0.8660254037844387076, 1.000000000000000000, 0.8660254037844387076, 1.000000000000000000, 0.8660254037844387076, 1.000000000000000000, 0.8660254037844387076, 1.000000000000000000, 0.8660254037844387076, 1.000000000000000000, 0.8660254037844387076, 1.000000000000000000, 0.8660254037844387076, 1.000000000000000000, 0.8660254037844387076, 1.000000000000000000, 0.8660254037844387076, 1.000000000000000000, 0.8660254037844387076, 1.000000000000000000, 0.8660254037844387076, 1.000000000000000000, 0.8660254037844387076, 1.000000000000000000, 0.8660254037844387076, 1.000000000000000000, 0.8660254037844387076, 1.000000000000000000, 0.8660254037844387076, 1.000000000000000000, 0.8660254037844387076, 1.000000000000000000, 0.8660254037844387076, 1.000000000000000000, 0.8660254037844387076, 1.000000000000000000, 0.8660254037844387076, 1.000000000000000000, 0.8660254037844387076, 1.000000000000000000, 0.8660254037844387076, 1.000000000000000000, 0.8660254037844387076, 1.000000000000000000, 0.8660254037844387076, 1.000000000000000000, 0.8660254037844387076, 1.000000000000000000, 0.8660254037844387076, 1.000000000000000000, 0.8660254037844387076, 1.000000000000000000, 0.8660254037844387076, 1.000000000000000000, 0.8660254037844387076, 1.000000000000000000, 0.8660254037844387076, 1.000000000000000000, 0.8660254037844387076, 1.000000000000000000, 0.8660254037844387076, 1.000000000000000000, 0.8660254037844387076, 1.000000000000000000, 0.8660254037844387076, 1.000000000000000000, 0.8660254037844387076, 1.000000000000000000, 0.8660254037844387076, 1.000000000000000000, 0.8660254037844387076, 1.000000000000000000, 0.8660254037844387076, 1.000000000000000000, 0.8660254037844387076, 1.000000000000000000, 0.8660254037844387076, 1.000000000000000000, 0.8660254037844387076, 1.000000000000000000, 0.8660254037844387076, 1.000000000000000000, 0.8660254037844387076, 1.000000000000000000, 0.8660254037844387076, 1.000000000000000000, 0.8660254037844387076, 1.000000000000000000, 0.8660254037844387076, 1.000000000000000000, 0.8660254037844387076, 1.000000000000000000, 0.8660254037844387076, 1.000000000000000000, 0.8660254037844387076, 1.000000000000000000, 0.8660254037844387076, 1.000000000000000000, 0.8660254037844387076, 1.000000000000000000, 0.8660254037844387076, 1.000000000000000000, 0.8660254037844387076, 1.000000000000000000, 0.8660254037844387076, 1.000000000000000000, 0.8660254037844387076, 1.000000000000000000, 0.8660254037844387076, 1.000000000000000000, 0.8660254037844387076, 1.000000000000000000, 0.8660254037844387076, 1.000000000000000000, 0.8660254037844387076, 1.000000000000000000, 0.8660254037844387076, 1.000000000000000000, 0.8660254037844387076, 1.000000000000000000, 0.8660254037844387076, 1.000000000000000000, 0.8660254037844387076, 1.000000000000000000, 0.8660254037844387076, 1.000000000000000000, 0.8660254037844387076, 1.000000000000000000, 0.8660254037844387076, 1.000000000000000000, 0.8660254037844387076, 1.000000000000000000, 0.8660254037844387076, 1.000000000000000000, 0.8660254037844387076, 1.000000000000000000, 0.8660254037844387076, 1.000000000000000000, 0.8660254037844387076, 1.000000000000000000, 0.8660254037844387076, 1.000000000000000000, 0.8660254037844387076, 1.000000000000000000, 0.8660254037844387076, 1.000000000000000000, 0.8660254037844387076, 1.000000000000000000, 0.8660254037844387076, 1.000000000000000000, 0.8660254037844387076, 1.000000000000000000, 0.8660254037844387076, 1.000000000000000000, 0.8660254037844387076, 1.000000000000000000, 0.8660254037844387076, 1.000000000000000000, 0.8660254037844387076, 1.000000000000000000, 0.8660254037844387076, 1.000000000000000000, 0.8660254037844387076, 1.000000000000000000, 0.8660254037844387076, 1.000000000000000000, 0.8660254037844387076, 1.000000000000000000, 0.8660254037844387076, 1.000000000000000000, 0.8660254037844387076, 1.000000000000000000, 0.8660254037844387076, 1.000000000000000000, 0.8660254037844387076, 1.000000000000000000, 0.8660254037844387076, 1.000000000000000000, 0.8660254037844387076, 1.000000000000000000, 0.8660254037844387076, 1.000000000000000000, 0.8660254037844387076, 1.000000000000000000, 0.8660254037844387076, 1.000000000000000000, 0.8660254037844387076, 1.000000000000000000, 0.8660254037844387076, 1.000000000000000000, 0.8660254037844387076, 1.000000000000000000, 0.8660254037844387076, 1.000000000000000000, 0.8660254037844387076, 1.000000000000000000, 0.8660254037844387076, 1.000000000000000000, 0.8660254037844387076, 1.000000000000000000, 0.8660254037844387076, 1.000000000000000000, 0.8660254037844387076, 1.000000000000000000, 0.8660254037844387076, 1.000000000000000000, 0.8660254037844387076, 1.000000000000000000, 0.8660254037844387076, 1.000000000000000000, 0.8660254037844387076, 1.000000000000000000, 0.8660254037844387076, 1.000000000000000000, 0.8660254037844387076, 1.000000000000000000, 0.8660254037844387076, 1.000000000000000000, 0.8660254037844387076, 1.000000000000000000, 0.8660254037844387076, 1.000000000000000000, 0.8660254037844387076, 1.000000000000000000, 0.8660254037844387076, 1.000000000000000000, 0.8660254037844387076, 1.000000000000000000, 0.8660254037844387076, 1.000000000000000000, 0.8660254037844387076, 1.000000000000000000, 0.8660254037844387076, 1.000000000000000000, 0.8660254037844387076, 1.000000000000000000, 0.8660254037844387076, 1.000000000000000000, 0.8660254037844387076, 1.000000000000000000, 0.8660254037844387076, 1.000000000000000000, 0.8660254037844387076, 1.000000000000000000, 0.8660254037844387076, 1.000000000000000000, 0.8660254037844387076, 1.000000000000000000, 0.8660254037844387076, 1.000000000000000000, 0.8660254037844387076, 1.000000000000000000, 0.8660254037844387076, 1.000000000000000000, 0.8660254037844387076, 1.000000000000000000, 0.8660254037844387076, 1.000000000000000000, 0.8660254037844387076, 1.000000000000000000, 0.8660254037844387076, 1.000000000000000000, 0.8660254037844387076, 1.000000000000000000, 0.8660254037844387076, 1.000000000000000000, 0.8660254037844387076, 1.000000000000000000, 0.8660254037844387076, 1.000000000000000000, 0.8660254037844387076, 1.000000000000000000, 0.8660254037844387076, 1.000000000000000000, 0.8660254037844387076, 1.000000000000000000, 0.8660254037844387076, 1.000000000000000000, 0.8660254037844387076, 1.000000000000000000, 0.8660254037844387076, 1.000000000000000000, 0.8660254037844387076, 1.000000000000000000, 0.8660254037844387076, 1.000000000000000000, 0.8660254037844387076, 1.000000000000000000, 0.8660254037844387076, 1.000000000000000000, 0.8660254037844387076, 1.000000000000000000, 0.8660254037844387076, 1.000000000000000000, 0.8660254037844387076, 1.000000000000000000, 0.8660254037844387076, 1.000000000000000000, 0.8660254037844387076, 1.000000000000000000, 0.8660254037844387076, 1.000000000000000000, 0.8660254037844387076, 1.000000000000000000, 0.8660254037844387076, 1.000000000000000000, 0.8660254037844387076, 1.000000000000000000, 0.8660254037844387076, 1.000000000000000000, 0.8660254037844387076, 1.000000000000000000, 0.8660254037844387076, 1.000000000000000000, 0.8660254037844387076, 1.000000000000000000, 0.8660254037844387076, 1.000000000000000000, 0.8660254037844387076, 1.000000000000000000, 0.8660254037844387076, 1.000000000000000000, 0.8660254037844387076, 1.000000000000000000, 0.8660254037844387076, 1.000000000000000000, 0.8660254037844387076, 1.000000000000000000, 0.8660254037844387076, 1.000000000000000000, 0.8660254037844387076, 1.000000000000000000, 0.8660254037844387076, 1.000000000000000000, 0.8660254037844387076, 1.000000000000000000, 0.8660254037844387076, 1.000000000000000000, 0.8660254037844387076, 1.000000000000000000, 0.8660254037844387076, 1.000000000000000000, 0.8660254037844387076, 1.000000000000000000, 0.8660254037844387076, 1.000000000000000000, 0.8660254037844387076, 1.000000000000000000, 0.8660254037844387076, 1.000000000000000000, 0.8660254037844387076, 1.000000000000000000, 0.8660254037844387076, 1.000000000000000000, 0.8660254037844387076, 1.000000000000000000, 0.8660254037844387076, 1.000000000000000000, 0.8660254037844387076, 1.000000000000000000, 0.8660254037844387076, 1.000000000000000000, 0.8660254037844387076, 1.000000000000000000, 0.8660254037844387076, 1.000000000000000000, 0.8660254037844387076, 1.000000000000000000, 0.8660254037844387076, 1.000000000000000000, 0.8660254037844387076, 1.000000000000000000, 0.8660254037844387076, 1.000000000000000000, 0.8660254037844387076, 1.000000000000000000, 0.8660254037844387076, 1.000000000000000000, 0.8660254037844387076, 1.000000000000000000, 0.8660254037844387076, 1.000000000000000000, 0.8660254037844387076, 1.000000000000000000, 0.8660254037844387076, 1.000000000000000000, 0.8660254037844387076, 1.000000000000000000, 0.8660254037844387076, 1.000000000000000000, 0.8660254037844387076, 1.000000000000000000, 0.8660254037844387076, 1.000000000000000000, 0.8660254037844387076, 1.000000000000000000, 0.8660254037844387076, 1.000000000000000000, 0.8660254037844387076, 1.000000000000000000, 0.8660254037844387076, 1.000000000000000000, 0.8660254037844387076, 1.000000000000000000, 0.8660254037844387076, 1.000000000000000000, 0.8660254037844387076, 1.000000000000000000, 0.8660254037844387076, 1.000000000000000000, 0.8660254037844387076, 1.000000000000000000, 0.8660254037844387076, 1.000000000000000000, 0.8660254037844387076, 1.000000000000000000, 0.8660254037844387076, 1.000000000000000000, 0.8660254037844387076, 1.000000000000000000, 0.8660254037844387076, 1.000000000000000000, 0.8660254037844387076, 1.000000000000000000, 0.8660254037844387076, 1.000000000000000000, 0.8660254037844387076, 1.000000000000000000, 0.8660254037844387076, 1.000000000000000000, 0.8660254037844387076, 1.000000000000000000, 0.8660254037844387076, 1.000000000000000000, 0.8660254037844387076, 1.000000000000000000, 0.8660254037844387076, 1.000000000000000000, 0.8660254037844387076, 1.000000000000000000, 0.8660254037844387076, 1.000000000000000000, 0.8660254037844387076, 1.000000000000000000, 0.8660254037844387076, 1.000000000000000000, 0.8660254037844387076, 1.000000000000000000, 0.8660254037844387076, 1.000000000000000000, 0.8660254037844387076, 1.000000000000000000, 0.8660254037844387076, 1.000000000000000000, 0.8660254037844387076, 1.000000000000000000, 0.8660254037844387076, 1.000000000000000000, 0.8660254037844387076, 1.000000000000000000, 0.8660254037844387076, 1.000000000000000000, 0.8660254037844387076, 1.000000000000000000, 0.8660254037844387076, 1.000000000000000000, 0.8660254037844387076, 1.000000000000000000, 0.8660254037844387076, 1.000000000000000000, 0.8660254037844387076, 1.000000000000000000, 0.8660254037844387076, 1.000000000000000000, 0.8660254037844387076, 1.000000000000000000, 0.8660254037844387076, 1.000000000000000000, 0.8660254037844387076, 1.000000000000000000, 0.8660254037844387076, 1.000000000000000000, 0.8660254037844387076, 1.000000000000000000, 0.8660254037844387076, 1.000000000000000000, 0.8660254037844387076, 1.000000000000000000),
 ( 1.000000000000000000, 0.8660254037844387076, 1.000000000000000000, 0.8660254037844387076, 1.000000000000000000, 0.8660254037844387076, 1.000000000000000000, 0.8660254037844387076, 1.000000000000000000, 0.8660254037844387076, 1.000000000000000000, 0.8660254037844387076, 1.000000000000000000, 0.8660254037844387076, 1.000000000000000000, 0.8660254037844387076, 1.000000000000000000, 0.8660254037844387076, 1.000000000000000000, 0.8660254037844387076, 1.000000000000000000, 0.8660254037844387076, 1.000000000000000000, 0.8660254037844387076, 1.000000000000000000, 0.8660254037844387076, 1.000000000000000000, 0.8660254037844387076, 1.000000000000000000, 0.8660254037844387076, 1.000000000000000000, 0.8660254037844387076, 1.000000000000000000, 0.8660254037844387076, 1.000000000000000000, 0.8660254037844387076, 1.000000000000000000, 0.8660254037844387076, 1.000000000000000000, 0.8660254037844387076, 1.000000000000000000, 0.8660254037844387076, 1.000000000000000000, 0.8660254037844387076, 1.000000000000000000, 0.8660254037844387076, 1.000000000000000000, 0.8660254037844387076, 1.000000000000000000, 0.8660254037844387076, 1.000000000000000000, 0.8660254037844387076, 1.000000000000000000, 0.8660254037844387076, 1.000000000000000000, 0.8660254037844387076, 1.000000000000000000, 0.8660254037844387076, 1.000000000000000000, 0.8660254037844387076, 1.000000000000000000, 0.8660254037844387076, 1.000000000000000000, 0.8660254037844387076, 1.000000000000000000, 0.8660254037844387076, 1.000000000000000000, 0.8660254037844387076, 1.000000000000000000, 0.8660254037844387076, 1.000000000000000000, 0.8660254037844387076, 1.000000000000000000, 0.8660254037844387076, 1.000000000000000000, 0.8660254037844387076, 1.000000000000000000, 0.8660254037844387076, 1.000000000000000000, 0.8660254037844387076, 1.000000000000000000, 0.8660254037844387076, 1.000000000000000000, 0.8660254037844387076, 1.000000000000000000, 0.8660254037844387076, 1.000000000000000000, 0.8660254037844387076, 1.000000000000000000, 0.8660254037844387076, 1.000000000000000000, 0.8660254037844387076, 1.000000000000000000, 0.8660254037844387076, 1.000000000000000000, 0.8660254037844387076, 1.000000000000000000, 0.8660254037844387076, 1.000000000000000000, 0.8660254037844387076, 1.000000000000000000, 0.8660254037844387076, 1.000000000000000000, 0.8660254037844387076, 1.000000000000000000, 0.8660254037844387076, 1.000000000000000000, 0.8660254037844387076, 1.000000000000000000, 0.8660254037844387076, 1.000000000000000000, 0.8660254037844387076, 1.000000000000000000, 0.8660254037844387076, 1.000000000000000000, 0.8660254037844387076, 1.000000000000000000, 0.8660254037844387076, 1.000000000000000000, 0.8660254037844387076, 1.000000000000000000, 0.8660254037844387076, 1.000000000000000000, 0.8660254037844387076, 1.000000000000000000, 0.8660254037844387076, 1.000000000000000000, 0.8660254037844387076, 1.000000000000000000, 0.8660254037844387076, 1.000000000000000000, 0.8660254037844387076, 1.000000000000000000, 0.8660254037844387076, 1.000000000000000000, 0.8660254037844387076, 1.000000000000000000, 0.8660254037844387076, 1.000000000000000000, 0.8660254037844387076, 1.000000000000000000, 0.8660254037844387076, 1.000000000000000000, 0.8660254037844387076, 1.000000000000000000, 0.8660254037844387076, 1.000000000000000000, 0.8660254037844387076, 1.000000000000000000, 0.8660254037844387076, 1.000000000000000000, 0.8660254037844387076, 1.000000000000000000, 0.8660254037844387076, 1.000000000000000000, 0.8660254037844387076, 1.000000000000000000, 0.8660254037844387076, 1.000000000000000000, 0.8660254037844387076, 1.000000000000000000, 0.8660254037844387076, 1.000000000000000000, 0.8660254037844387076, 1.000000000000000000, 0.8660254037844387076, 1.000000000000000000, 0.8660254037844387076, 1.000000000000000000, 0.8660254037844387076, 1.000000000000000000, 0.8660254037844387076, 1.000000000000000000, 0.8660254037844387076, 1.000000000000000000, 0.8660254037844387076, 1.000000000000000000, 0.8660254037844387076, 1.000000000000000000, 0.8660254037844387076, 1.000000000000000000, 0.8660254037844387076, 1.000000000000000000, 0.8660254037844387076, 1.000000000000000000, 0.8660254037844387076, 1.000000000000000000, 0.8660254037844387076, 1.000000000000000000, 0.8660254037844387076, 1.000000000000000000, 0.8660254037844387076, 1.000000000000000000, 0.8660254037844387076, 1.000000000000000000, 0.8660254037844387076, 1.000000000000000000, 0.8660254037844387076, 1.000000000000000000, 0.8660254037844387076, 1.000000000000000000, 0.8660254037844387076, 1.000000000000000000, 0.8660254037844387076, 1.000000000000000000, 0.8660254037844387076, 1.000000000000000000, 0.8660254037844387076, 1.000000000000000000, 0.8660254037844387076, 1.000000000000000000, 0.8660254037844387076, 1.000000000000000000, 0.8660254037844387076, 1.000000000000000000, 0.8660254037844387076, 1.000000000000000000, 0.8660254037844387076, 1.000000000000000000, 0.8660254037844387076, 1.000000000000000000, 0.8660254037844387076, 1.000000000000000000, 0.8660254037844387076, 1.000000000000000000, 0.8660254037844387076, 1.000000000000000000, 0.8660254037844387076, 1.000000000000000000, 0.8660254037844387076, 1.000000000000000000, 0.8660254037844387076, 1.000000000000000000, 0.8660254037844387076, 1.000000000000000000, 0.8660254037844387076, 1.000000000000000000, 0.8660254037844387076, 1.000000000000000000, 0.8660254037844387076, 1.000000000000000000, 0.8660254037844387076, 1.000000000000000000, 0.8660254037844387076, 1.000000000000000000, 0.8660254037844387076, 1.000000000000000000, 0.8660254037844387076, 1.000000000000000000, 0.8660254037844387076, 1.000000000000000000, 0.8660254037844387076, 1.000000000000000000, 0.8660254037844387076, 1.000000000000000000, 0.8660254037844387076, 1.000000000000000000, 0.8660254037844387076, 1.000000000000000000, 0.8660254037844387076, 1.000000000000000000, 0.8660254037844387076, 1.000000000000000000, 0.8660254037844387076, 1.000000000000000000, 0.8660254037844387076, 1.000000000000000000, 0.8660254037844387076, 1.000000000000000000, 0.8660254037844387076, 1.000000000000000000, 0.8660254037844387076, 1.000000000000000000, 0.8660254037844387076, 1.000000000000000000, 0.8660254037844387076, 1.000000000000000000, 0.8660254037844387076, 1.000000000000000000, 0.8660254037844387076, 1.000000000000000000, 0.8660254037844387076, 1.000000000000000000, 0.8660254037844387076, 1.000000000000000000, 0.8660254037844387076, 1.000000000000000000, 0.8660254037844387076, 1.000000000000000000, 0.8660254037844387076, 1.000000000000000000, 0.8660254037844387076, 1.000000000000000000, 0.8660254037844387076, 1.000000000000000000, 0.8660254037844387076, 1.000000000000000000, 0.8660254037844387076, 1.000000000000000000, 0.8660254037844387076, 1.000000000000000000, 0.8660254037844387076, 1.000000000000000000, 0.8660254037844387076, 1.000000000000000000, 0.8660254037844387076, 1.000000000000000000, 0.8660254037844387076, 1.000000000000000000, 0.8660254037844387076, 1.000000000000000000, 0.8660254037844387076, 1.000000000000000000, 0.8660254037844387076, 1.000000000000000000, 0.8660254037844387076, 1.000000000000000000, 0.8660254037844387076, 1.000000000000000000, 0.8660254037844387076, 1.000000000000000000, 0.8660254037844387076, 1.000000000000000000, 0.8660254037844387076, 1.000000000000000000, 0.8660254037844387076, 1.000000000000000000, 0.8660254037844387076, 1.000000000000000000, 0.8660254037844387076, 1.000000000000000000, 0.8660254037844387076, 1.000000000000000000, 0.8660254037844387076, 1.000000000000000000, 0.8660254037844387076, 1.000000000000000000, 0.8660254037844387076, 1.000000000000000000, 0.8660254037844387076, 1.000000000000000000, 0.8660254037844387076, 1.000000000000000000, 0.8660254037844387076, 1.000000000000000000, 0.8660254037844387076, 1.000000000000000000, 0.8660254037844387076, 1.000000000000000000, 0.8660254037844387076, 1.000000000000000000, 0.8660254037844387076, 1.000000000000000000, 0.8660254037844387076, 1.000000000000000000, 0.8660254037844387076, 1.000000000000000000, 0.8660254037844387076, 1.000000000000000000, 0.8660254037844387076, 1.000000000000000000, 0.8660254037844387076, 1.000000000000000000, 0.8660254037844387076, 1.000000000000000000, 0.8660254037844387076, 1.000000000000000000, 0.8660254037844387076, 1.000000000000000000, 0.8660254037844387076, 1.000000000000000000, 0.8660254037844387076, 1.000000000000000000, 0.8660254037844387076, 1.000000000000000000, 0.8660254037844387076, 1.000000000000000000, 0.8660254037844387076, 1.000000000000000000, 0.8660254037844387076, 1.000000000000000000, 0.8660254037844387076, 1.000000000000000000, 0.8660254037844387076, 1.000000000000000000, 0.8660254037844387076, 1.000000000000000000, 0.8660254037844387076, 1.000000000000000000, 0.8660254037844387076, 1.000000000000000000, 0.8660254037844387076, 1.000000000000000000, 0.8660254037844387076, 1.000000000000000000, 0.8660254037844387076, 1.000000000000000000, 0.8660254037844387076, 1.000000000000000000, 0.8660254037844387076, 1.000000000000000000, 0.8660254037844387076, 1.000000000000000000, 0.8660254037844387076, 1.000000000000000000, 0.8660254037844387076, 1.000000000000000000, 0.8660254037844387076, 1.000000000000000000, 0.8660254037844387076, 1.000000000000000000, 0.8660254037844387076, 1.000000000000000000, 0.8660254037844387076, 1.000000000000000000, 0.8660254037844387076, 1.000000000000000000, 0.8660254037844387076, 1.000000000000000000, 0.8660254037844387076, 1.000000000000000000, 0.8660254037844387076, 1.000000000000000000, 0.8660254037844387076, 1.000000000000000000, 0.8660254037844387076, 1.000000000000000000, 0.8660254037844387076, 1.000000000000000000, 0.8660254037844387076, 1.000000000000000000, 0.8660254037844387076, 1.000000000000000000, 0.8660254037844387076, 1.000000000000000000, 0.8660254037844387076, 1.000000000000000000, 0.8660254037844387076, 1.000000000000000000, 0.8660254037844387076, 1.000000000000000000, 0.8660254037844387076, 1.000000000000000000, 0.8660254037844387076, 1.000000000000000000, 0.8660254037844387076, 1.000000000000000000, 0.8660254037844387076, 1.000000000000000000, 0.8660254037844387076, 1.000000000000000000, 0.8660254037844387076, 1.000000000000000000, 0.8660254037844387076, 1.000000000000000000, 0.8660254037844387076, 1.000000000000000000, 0.8660254037844387076, 1.000000000000000000, 0.8660254037844387076, 1.000000000000000000, 0.8660254037844387076, 1.000000000000000000, 0.8660254037844387076, 1.000000000000000000, 0.8660254037844387076, 1.000000000000000000, 0.8660254037844387076, 1.000000000000000000, 0.8660254037844387076, 1.000000000000000000, 0.8660254037844387076, 1.000000000000000000, 0.8660254037844387076, 1.000000000000000000, 0.8660254037844387076, 1.000000000000000000, 0.8660254037844387076, 1.000000000000000000, 0.8660254037844387076, 1.000000000000000000, 0.8660254037844387076, 1.000000000000000000, 0.8660254037844387076, 1.000000000000000000, 0.8660254037844387076, 1.000000000000000000, 0.8660254037844387076, 1.000000000000000000, 0.8660254037844387076, 1.000000000000000000, 0.8660254037844387076, 1.000000000000000000, 0.8660254037844387076, 1.000000000000000000, 0.8660254037844387076, 1.000000000000000000, 0.8660254037844387076, 1.000000000000000000, 0.8660254037844387076, 1.000000000000000000, 0.8660254037844387076, 1.000000000000000000, 0.8660254037844387076, 1.000000000000000000, 0.8660254037844387076, 1.000000000000000000, 0.8660254037844387076, 1.000000000000000000, 0.8660254037844387076, 1.000000000000000000, 0.8660254037844387076, 1.000000000000000000, 0.8660254037844387076, 1.000000000000000000, 0.8660254037844387076, 1.000000000000000000, 0.8660254037844387076, 1.000000000000000000, 0.8660254037844387076, 1.000000000000000000, 0.8660254037844387076, 1.000000000000000000, 0.8660254037844387076, 1.000000000000000000, 0.8660254037844387076, 1.000000000000000000, 0.8660254037844387076, 1.000000000000000000, 0.8660254037844387076, 1.000000000000000000, 0.8660254037844387076, 1.000000000000000000, 0.8660254037844387076, 1.000000000000000000, 0.8660254037844387076, 1.000000000000000000, 0.8660254037844387076, 1.000000000000000000, 0.8660254037844387076, 1.000000000000000000, 0.8660254037844387076, 1.000000000000000000, 0.8660254037844387076, 1.000000000000000000, 0.8660254037844387076, 1.000000000000000000, 0.8660254037844387076, 1.000000000000000000, 0.8660254037844387076, 1.000000000000000000, 0.8660254037844387076, 1.000000000000000000, 0.8660254037844387076, 1.000000000000000000, 0.8660254037844387076, 1.000000000000000000, 0.8660254037844387076, 1.000000000000000000, 0.8660254037844387076, 1.000000000000000000, 0.8660254037844387076, 1.000000000000000000, 0.8660254037844387076, 1.000000000000000000, 0.8660254037844387076, 1.000000000000000000, 0.8660254037844387076, 1.000000000000000000, 0.8660254037844387076, 1.000000000000000000, 0.8660254037844387076, 1.000000000000000000, 0.8660254037844387076, 1.000000000000000000, 0.8660254037844387076, 1.000000000000000000, 0.8660254037844387076, 1.000000000000000000, 0.8660254037844387076, 1.000000000000000000, 0.8660254037844387076, 1.000000000000000000, 0.8660254037844387076, 1.000000000000000000, 0.8660254037844387076, 1.000000000000000000, 0.8660254037844387076, 1.000000000000000000, 0.8660254037844387076, 1.000000000000000000, 0.8660254037844387076, 1.000000000000000000, 0.8660254037844387076, 1.000000000000000000, 0.8660254037844387076, 1.000000000000000000, 0.8660254037844387076, 1.000000000000000000, 0.8660254037844387076, 1.000000000000000000, 0.8660254037844387076, 1.000000000000000000, 0.8660254037844387076, 1.000000000000000000, 0.8660254037844387076, 1.000000000000000000, 0.8660254037844387076, 1.000000000000000000, 0.8660254037844387076, 1.000000000000000000, 0.8660254037844387076, 1.000000000000000000, 0.8660254037844387076, 1.000000000000000000, 0.8660254037844387076, 1.000000000000000000, 0.8660254037844387076, 1.000000000000000000, 0.8660254037844387076, 1.000000000000000000, 0.8660254037844387076, 1.000000000000000000, 0.8660254037844387076, 1.000000000000000000, 0.8660254037844387076, 1.000000000000000000, 0.8660254037844387076, 1.000000000000000000, 0.8660254037844387076, 1.000000000000000000, 0.8660254037844387076, 1.000000000000000000, 0.8660254037844387076, 1.000000000000000000, 0.8660254037844387076, 1.000000000000000000, 0.8660254037844387076, 1.000000000000000000, 0.8660254037844387076, 1.000000000000000000, 0.8660254037844387076, 1.000000000000000000, 0.8660254037844387076, 1.000000000000000000, 0.8660254037844387076, 1.000000000000000000, 0.8660254037844387076, 1.000000000000000000, 0.8660254037844387076, 1.000000000000000000, 0.8660254037844387076, 1.000000000000000000, 0.8660254037844387076, 1.000000000000000000, 0.8660254037844387076, 1.000000000000000000, 0.8660254037844387076, 1.000000000000000000, 0.8660254037844387076, 1.000000000000000000, 0.8660254037844387076, 1.000000000000000000, 0.8660254037844387076, 1.000000000000000000, 0.8660254037844387076, 1.000000000000000000, 0.8660254037844387076, 1.000000000000000000, 0.8660254037844387076, 1.000000000000000000, 0.8660254037844387076, 1.000000000000000000, 0.8660254037844387076, 1.000000000000000000, 0.8660254037844387076, 1.000000000000000000, 0.8660254037844387076, 1.000000000000000000, 0.8660254037844387076, 1.000000000000000000, 0.8660254037844387076, 1.000000000000000000, 0.8660254037844387076, 1.000000000000000000, 0.8660254037844387076, 1.000000000000000000, 0.8660254037844387076, 1.000000000000000000, 0.8660254037844387076, 1.000000000000000000, 0.8660254037844387076, 1.000000000000000000, 0.8660254037844387076, 1.000000000000000000, 0.8660254037844387076, 1.000000000000000000, 0.8660254037844387076, 1.000000000000000000, 0.8660254037844387076, 1.000000000000000000, 0.8660254037844387076, 1.000000000000000000, 0.8660254037844387076, 1.000000000000000000, 0.8660254037844387076, 1.000000000000000000, 0.8660254037844387076, 1.000000000000000000, 0.8660254037844387076, 1.000000000000000000, 0.8660254037844387076, 1.000000000000000000, 0.8660254037844387076, 1.000000000000000000, 0.8660254037844387076, 1.000000000000000000, 0.8660254037844387076, 1.000000000000000000, 0.8660254037844387076, 1.000000000000000000) ) ) 
 REPRESENTATION_ITEM ( '' )  SURFACE ( )  );
#26668 = CARTESIAN_POINT ( 'NONE',  ( 23.25937500061451857, -4.541064518000417216, -2.621784821875001281 ) ) ;
#26669 = CARTESIAN_POINT ( 'NONE',  ( 20.76562500061451644, 3.027376345333611329, 5.243569643749999010 ) ) ;
#26670 = CARTESIAN_POINT ( 'NONE',  ( 4.000000000000000000, 12.53749999999999964, 32.30940107675849049 ) ) ;
#26671 = CARTESIAN_POINT ( 'NONE',  ( 25.82812500061451644, -4.541064518000419881, 2.621784821874995952 ) ) ;
#26672 = CARTESIAN_POINT ( 'NONE',  ( 6.600000001229032520, 5.773502691896255534, 3.535250795749688894E-16 ) ) ;
#26673 = VECTOR ( 'NONE', #39067, 1000.000000000000000 ) ;
#26674 = ORIENTED_EDGE ( 'NONE', *, *, #13592, .F. ) ;
#26675 = CARTESIAN_POINT ( 'NONE',  ( 22.46250000122903501, 0.000000000000000000, 4.999999999999998224 ) ) ;
#26676 = CARTESIAN_POINT ( 'NONE',  ( 4.000000000000000000, 14.33750000000000213, -27.69059892324149530 ) ) ;
#26677 = CARTESIAN_POINT ( 'NONE',  ( 22.80000000122903359, 5.773502691896255534, 3.535250795749688894E-16 ) ) ;
#26678 = CARTESIAN_POINT ( 'NONE',  ( 3.756430356250000102, 15.45312499938548356, 30.00000000000000000 ) ) ;
#26679 = CARTESIAN_POINT ( 'NONE',  ( 4.509375000614518569, 4.541064518000418104, -2.621784821874998173 ) ) ;
#26680 = CARTESIAN_POINT ( 'NONE',  ( 23.36250000000000071, -5.773502691896255534, -1.060575238724906372E-15 ) ) ;
#26681 = CARTESIAN_POINT ( 'NONE',  ( 12.51562500061451821, 3.027376345333613106, -5.243569643749998122 ) ) ;
#26682 = CARTESIAN_POINT ( 'NONE',  ( 8.334375000614516082, -4.541064518000419881, 2.621784821874995952 ) ) ;
#26683 = CARTESIAN_POINT ( 'NONE',  ( 23.81250000122903288, 0.000000000000000000, 4.999999999999998224 ) ) ;
#26684 = CARTESIAN_POINT ( 'NONE',  ( 14.33437500061451786, 6.421520780324663323E-16, -5.243569643749999010 ) ) ;
#26685 = CARTESIAN_POINT ( 'NONE',  ( 2.859375000614519546, 0.000000000000000000, 5.243569643749999010 ) ) ;
#26686 = CARTESIAN_POINT ( 'NONE',  ( 8.025000001229035007, 2.886751345948126879, 4.999999999999998224 ) ) ;
#26687 = CARTESIAN_POINT ( 'NONE',  ( 4.303125000614516971, -4.541064518000417216, -2.621784821875001281 ) ) ;
#26688 = CARTESIAN_POINT ( 'NONE',  ( 14.27812500061451573, 6.421520780324663323E-16, -5.243569643749999010 ) ) ;
#26689 = ORIENTED_EDGE ( 'NONE', *, *, #35579, .F. ) ;
#26690 = CARTESIAN_POINT ( 'NONE',  ( 11.95312500061451644, -4.541064518000417216, -2.621784821875001281 ) ) ;
#26691 = CARTESIAN_POINT ( 'NONE',  ( 9.103125000614515017, 0.000000000000000000, 5.243569643749999010 ) ) ;
#26692 = CARTESIAN_POINT ( 'NONE',  ( 20.44687500061451857, -2.746126346562646425, 4.756430356249996549 ) ) ;
#26693 = CARTESIAN_POINT ( 'NONE',  ( 8.175000000000002487, 6.123233995736764310E-16, -4.999999999999998224 ) ) ;
#26694 = CARTESIAN_POINT ( 'NONE',  ( 4.237500001229036251, 6.123233995736764310E-16, -4.999999999999998224 ) ) ;
#26695 = CARTESIAN_POINT ( 'NONE',  ( 18.59999999999999787, 4.330127018922192761, -2.499999999999997780 ) ) ;
#26696 = CARTESIAN_POINT ( 'NONE',  ( 19.35937500061451644, 4.541064518000418104, -2.621784821874998173 ) ) ;
#26697 = CARTESIAN_POINT ( 'NONE',  ( 13.20000000122903394, -2.886751345948125991, -5.000000000000000000 ) ) ;
#26698 = CARTESIAN_POINT ( 'NONE',  ( 23.02499999999999858, 6.123233995736764310E-16, -4.999999999999998224 ) ) ;
#26699 = AXIS2_PLACEMENT_3D ( 'NONE', #35581, #39057, #58102 ) ;
#26700 = CARTESIAN_POINT ( 'NONE',  ( -3.000416591977282496E-16, 16.99062500061451786, -34.90005215228797653 ) ) ;
#26701 = CARTESIAN_POINT ( 'NONE',  ( 21.48750000000000071, -2.886751345948130876, 4.999999999999996447 ) ) ;
#26702 = FACE_OUTER_BOUND ( 'NONE', #20520, .T. ) ;
#26703 = CARTESIAN_POINT ( 'NONE',  ( 28.67812500061451431, 6.421520780324663323E-16, -5.243569643749999010 ) ) ;
#26704 = FACE_OUTER_BOUND ( 'NONE', #13431, .T. ) ;
#26705 = CARTESIAN_POINT ( 'NONE',  ( 13.47187500061451537, 3.027376345333613106, -5.243569643749998122 ) ) ;
#26706 = CARTESIAN_POINT ( 'NONE',  ( 27.00000000000000000, -4.330127018922190985, -2.500000000000001332 ) ) ;
#26707 = CARTESIAN_POINT ( 'NONE',  ( 10.75312500061451715, 4.541064518000418104, -2.621784821874998173 ) ) ;
#26708 = CARTESIAN_POINT ( 'NONE',  ( 26.70937500061451431, -5.492252693125287522, -1.008910452111647106E-15 ) ) ;
#26709 = CARTESIAN_POINT ( 'NONE',  ( 20.29687500061451644, 6.054752690667223547, 3.707466751127219781E-16 ) ) ;
#26710 = CARTESIAN_POINT ( 'NONE',  ( 14.07187500061451679, -4.119189519843968306, 2.378215178124996054 ) ) ;
#26711 = CARTESIAN_POINT ( 'NONE',  ( 7.978125000614517681, 6.421520780324663323E-16, -5.243569643749999010 ) ) ;
#26712 = CARTESIAN_POINT ( 'NONE',  ( 13.09687500061451892, 6.054752690667223547, 3.707466751127219781E-16 ) ) ;
#26713 = ORIENTED_EDGE ( 'NONE', *, *, #25401, .F. ) ;
#26714 = CARTESIAN_POINT ( 'NONE',  ( 23.70937500061451786, -4.541064518000417216, -2.621784821875001281 ) ) ;
#26715 = CARTESIAN_POINT ( 'NONE',  ( 3.943546631589882168, 3.074146327801218881, -29.31700319132604093 ) ) ;
#26716 = CARTESIAN_POINT ( 'NONE',  ( 8.849999999999999645, 0.000000000000000000, 4.999999999999998224 ) ) ;
#26717 = EDGE_CURVE ( 'NONE', #40294, #47010, #3202, .T. ) ;
#26718 = CARTESIAN_POINT ( 'NONE',  ( 4.724999999999999645, 4.330127018922191873, 2.499999999999999556 ) ) ;
#26719 = CARTESIAN_POINT ( 'NONE',  ( 18.03750000122903430, -4.330127018922194537, 2.499999999999995559 ) ) ;
#26720 = DIRECTION ( 'NONE',  ( 0.000000000000000000, 1.000000000000000000, -6.195440985631456550E-17 ) ) ;
#26721 = CARTESIAN_POINT ( 'NONE',  ( 8.671875000614518214, -4.119189519843968306, 2.378215178124996054 ) ) ;
#26722 = ORIENTED_EDGE ( 'NONE', *, *, #24962, .T. ) ;
#26723 = CARTESIAN_POINT ( 'NONE',  ( 16.12500000000000000, -4.330127018922194537, 2.499999999999995559 ) ) ;
#26724 = CARTESIAN_POINT ( 'NONE',  ( 16.23750000000000071, -2.886751345948125991, -5.000000000000000000 ) ) ;
#26725 = CARTESIAN_POINT ( 'NONE',  ( 12.44062500061451537, -3.027376345333610441, -5.243569643749999898 ) ) ;
#26726 = ORIENTED_EDGE ( 'NONE', *, *, #4619, .F. ) ;
#26727 = CARTESIAN_POINT ( 'NONE',  ( 24.60000000000000142, 0.000000000000000000, 4.999999999999998224 ) ) ;
#26728 = CARTESIAN_POINT ( 'NONE',  ( -2.121784821874996840, 18.13437500061451502, -26.32496088578401583 ) ) ;
#26729 = CARTESIAN_POINT ( 'NONE',  ( 29.32500000122903216, -5.773502691896255534, -1.060575238724906372E-15 ) ) ;
#26730 = CARTESIAN_POINT ( 'NONE',  ( 3.756430356250000546, 15.37812499938548427, 27.83122392262697886 ) ) ;
#26731 = CARTESIAN_POINT ( 'NONE',  ( 10.87500000000000000, 6.123233995736764310E-16, -4.999999999999998224 ) ) ;
#26732 = CARTESIAN_POINT ( 'NONE',  ( 3.765213524098920406, 3.290336489363023365, -3.765213524098920406 ) ) ;
#26733 = EDGE_LOOP ( 'NONE', ( #44456, #67314, #8613, #14622 ) ) ;
#26734 = CARTESIAN_POINT ( 'NONE',  ( 9.001249775931846008E-16, 11.81562500061451715, 34.90005215228797653 ) ) ;
#26735 = CARTESIAN_POINT ( 'NONE',  ( 24.06562500061451715, -6.054752690667223547, -1.112240025338166033E-15 ) ) ;
#26736 = CARTESIAN_POINT ( 'NONE',  ( 3.593020343235445058, 3.477097182003509257, 3.793492915512545416 ) ) ;
#26737 = CARTESIAN_POINT ( 'NONE',  ( -3.756430356250000102, 19.61562499938548143, 30.00000000000000000 ) ) ;
#26738 = CARTESIAN_POINT ( 'NONE',  ( 21.72187500061451715, 3.027376345333611329, 5.243569643749999010 ) ) ;
#26739 = CARTESIAN_POINT ( 'NONE',  ( 19.90312500061451573, 0.000000000000000000, 5.243569643749999010 ) ) ;
#26740 = EDGE_CURVE ( 'NONE', #59952, #62607, #43825, .T. ) ;
#26741 = CARTESIAN_POINT ( 'NONE',  ( 4.243569643749999898, 15.07812500061459460, -30.00000000000000000 ) ) ;
#26742 = CARTESIAN_POINT ( 'NONE',  ( 23.13750000122903216, 6.123233995736764310E-16, -4.999999999999998224 ) ) ;
#26743 = CARTESIAN_POINT ( 'NONE',  ( 4.790625000614518569, -3.027376345333610441, -5.243569643749999898 ) ) ;
#26744 = CARTESIAN_POINT ( 'NONE',  ( 23.25937500061451857, -4.119189519843965641, -2.378215178125001383 ) ) ;
#26745 = CARTESIAN_POINT ( 'NONE',  ( 20.91562500061451502, -6.054752690667223547, -1.112240025338166033E-15 ) ) ;
#26746 = CARTESIAN_POINT ( 'NONE',  ( 7.809375000614519280, 0.000000000000000000, 4.756430356249998326 ) ) ;
#26747 = CARTESIAN_POINT ( 'NONE',  ( -1.878215178124999163, 19.54062499938548214, 26.74683588394047007 ) ) ;
#26748 = CARTESIAN_POINT ( 'NONE',  ( 15.72187500061451892, 3.027376345333613106, -5.243569643749998122 ) ) ;
#26749 = CARTESIAN_POINT ( 'NONE',  ( 15.38437500061451679, 4.541064518000418104, 2.621784821874999949 ) ) ;
#26750 = CARTESIAN_POINT ( 'NONE',  ( 23.48437500061451644, 4.541064518000418104, 2.621784821874999949 ) ) ;
#26751 = CARTESIAN_POINT ( 'NONE',  ( -4.243569643749998122, 11.79687500061451999, 32.45002607614398471 ) ) ;
#26752 = CARTESIAN_POINT ( 'NONE',  ( 6.140625000614516438, -3.027376345333610441, -5.243569643749999898 ) ) ;
#26753 = CARTESIAN_POINT ( 'NONE',  ( 25.37812500061451715, -4.541064518000419881, 2.621784821874995952 ) ) ;
#26754 = EDGE_CURVE ( 'NONE', #8302, #56819, #60731, .T. ) ;
#26755 = CARTESIAN_POINT ( 'NONE',  ( 27.10312500061451502, 0.000000000000000000, 5.243569643749999010 ) ) ;
#26756 = CARTESIAN_POINT ( 'NONE',  ( 8.475000001229034297, 2.886751345948193936, 4.999999999999883649 ) ) ;
#26757 = CARTESIAN_POINT ( 'NONE',  ( 8.484601909799253346E-16, 19.21250000000000213, 34.61880215351700230 ) ) ;
#26758 = CARTESIAN_POINT ( 'NONE',  ( 6.121875000614517504, -6.054752690667223547, -1.112240025338166033E-15 ) ) ;
#26759 = DIRECTION ( 'NONE',  ( 0.000000000000000000, 0.000000000000000000, 1.000000000000000000 ) ) ;
#26760 = CARTESIAN_POINT ( 'NONE',  ( 14.58750000122903323, 6.123233995736764310E-16, -4.999999999999998224 ) ) ;
#26761 = CARTESIAN_POINT ( 'NONE',  ( 9.600000001229034297, -2.886751345948125991, -5.000000000000000000 ) ) ;
#26762 = CARTESIAN_POINT ( 'NONE',  ( 3.065625000614517592, 3.027376345333613106, -5.243569643749998122 ) ) ;
#26763 = CARTESIAN_POINT ( 'NONE',  ( -4.000000000000000000, 15.36874999877096570, 30.00000000000000000 ) ) ;
#26764 = CARTESIAN_POINT ( 'NONE',  ( 19.63125000122903430, 4.330127018922191873, 2.499999999999999556 ) ) ;
#26765 = CARTESIAN_POINT ( 'NONE',  ( 14.82187500061451679, 3.027376345333613106, -5.243569643749998122 ) ) ;
#26766 = CARTESIAN_POINT ( 'NONE',  ( 7.575000000000001954, -4.330127018922194537, 2.499999999999995559 ) ) ;
#26767 = VERTEX_POINT ( 'NONE', #42721 ) ;
#26768 = CARTESIAN_POINT ( 'NONE',  ( 20.20312500061451644, 4.541064518000418104, -2.621784821874998173 ) ) ;
#26769 = CARTESIAN_POINT ( 'NONE',  ( 7.040625000614517681, -3.027376345333610441, -5.243569643749999898 ) ) ;
#26770 = CARTESIAN_POINT ( 'NONE',  ( 22.47187500061452070, 3.027376345333612662, -5.243569643749998122 ) ) ;
#26771 = CARTESIAN_POINT ( 'NONE',  ( 5.090625000614516615, -3.027376345333614438, 5.243569643749998122 ) ) ;
#26772 = CARTESIAN_POINT ( 'NONE',  ( -1.999999999999999112, 16.19374999877096499, 26.53589838486224650 ) ) ;
#26773 = CARTESIAN_POINT ( 'NONE',  ( 7.612500001229035362, 0.000000000000000000, 4.999999999999998224 ) ) ;
#26774 = CARTESIAN_POINT ( 'NONE',  ( 21.92812500061451431, 6.421520780324663323E-16, -5.243569643749999010 ) ) ;
#26775 = CARTESIAN_POINT ( 'NONE',  ( 1.999999999999998668, 17.26250000122903572, -33.46410161513775705 ) ) ;
#26776 = CARTESIAN_POINT ( 'NONE',  ( 11.55000000122903181, 5.773502691896255534, 3.535250795749688894E-16 ) ) ;
#26777 = CARTESIAN_POINT ( 'NONE',  ( 20.12812500061451715, 6.421520780324663323E-16, -5.243569643749999010 ) ) ;
#26778 = CARTESIAN_POINT ( 'NONE',  ( 14.99062500061451786, -3.027376345333614438, 5.243569643749998122 ) ) ;
#26779 = CARTESIAN_POINT ( 'NONE',  ( 28.32187500061451502, 2.746126346562645981, -4.756430356249997438 ) ) ;
#26780 = CARTESIAN_POINT ( 'NONE',  ( 16.19999999999999929, -4.330127018922190985, -2.500000000000001332 ) ) ;
#26781 = CARTESIAN_POINT ( 'NONE',  ( 12.11250000122903181, 0.000000000000000000, 4.999999999999998224 ) ) ;
#26782 = CARTESIAN_POINT ( 'NONE',  ( 8.915625000614515017, 3.027376345333613106, -5.243569643749998122 ) ) ;
#26783 = CARTESIAN_POINT ( 'NONE',  ( 11.84062500061451750, -3.027376345333614438, 5.243569643749998122 ) ) ;
#26784 = CARTESIAN_POINT ( 'NONE',  ( 21.18750000122903288, -4.330127018922194537, 2.499999999999995559 ) ) ;
#26785 = CARTESIAN_POINT ( 'NONE',  ( 20.10937500061451289, -4.541064518000417216, -2.621784821875001281 ) ) ;
#26786 = CARTESIAN_POINT ( 'NONE',  ( 24.93750000000000000, 5.773502691896255534, 3.535250795749688401E-16 ) ) ;
#26787 = CARTESIAN_POINT ( 'NONE',  ( 6.525000001229033231, 2.886751345948129099, -4.999999999999998224 ) ) ;
#26788 = AXIS2_PLACEMENT_3D ( 'NONE', #72725, #26939, #21737 ) ;
#26789 = CARTESIAN_POINT ( 'NONE',  ( 4.884375000614518569, 6.421520780324663323E-16, -5.243569643749999010 ) ) ;
#26790 = CARTESIAN_POINT ( 'NONE',  ( 23.93437500061451573, 4.541064518000418104, 2.621784821874999949 ) ) ;
#26791 = CARTESIAN_POINT ( 'NONE',  ( -1.487416814333745711E-14, 15.16250000000000142, 34.00000000000000000 ) ) ;
#26792 = CARTESIAN_POINT ( 'NONE',  ( 18.21562500061451573, -6.054752690667223547, -1.112240025338166033E-15 ) ) ;
#26793 = CARTESIAN_POINT ( 'NONE',  ( 24.04687500061451644, -3.027376345333614438, 5.243569643749998122 ) ) ;
#26794 = CARTESIAN_POINT ( 'NONE',  ( 1.878215178125000495, 19.12812499938548427, 26.74683588394047007 ) ) ;
#26795 = CARTESIAN_POINT ( 'NONE',  ( 29.73281250092177430, 0.000000000000000000, 5.121784821874998173 ) ) ;
#26796 = CARTESIAN_POINT ( 'NONE',  ( 27.98437500061451289, 4.541064518000418104, 2.621784821874999949 ) ) ;
#26797 = CARTESIAN_POINT ( 'NONE',  ( 20.67187500061451289, 4.119189519843966529, 2.378215178124999607 ) ) ;
#26798 = CARTESIAN_POINT ( 'NONE',  ( 15.85312500061451857, 0.000000000000000000, 5.243569643749999010 ) ) ;
#26799 = CARTESIAN_POINT ( 'NONE',  ( 14.33437500061451786, 6.421520780324663323E-16, -5.243569643749999010 ) ) ;
#26800 = VERTEX_POINT ( 'NONE', #25357 ) ;
#26801 = CARTESIAN_POINT ( 'NONE',  ( 22.42500000122903003, 2.886751345948093572, 5.000000000000056843 ) ) ;
#26802 = CARTESIAN_POINT ( 'NONE',  ( 22.11562500061451786, 3.027376345333611329, 5.243569643749999010 ) ) ;
#26803 = CARTESIAN_POINT ( 'NONE',  ( 3.999999999999999112, 13.02500000000000213, -30.00000000000000000 ) ) ;
#26804 = CARTESIAN_POINT ( 'NONE',  ( 0.000000000000000000, 27.50000000000000000, 26.00000000000000000 ) ) ;
#26805 = CARTESIAN_POINT ( 'NONE',  ( 13.76250000000000107, 2.886751345948126879, 4.999999999999999112 ) ) ;
#26806 = CARTESIAN_POINT ( 'NONE',  ( 23.17500000122903359, 2.886751345948129099, -4.999999999999998224 ) ) ;
#26807 = CARTESIAN_POINT ( 'NONE',  ( 19.26562500061451644, 3.027376345333613106, -5.243569643749998122 ) ) ;
#26808 = VERTEX_POINT ( 'NONE', #65242 ) ;
#26809 = CARTESIAN_POINT ( 'NONE',  ( 21.63749999999999929, -2.886751345948125991, -5.000000000000000000 ) ) ;
#26810 =( BOUNDED_CURVE ( )  B_SPLINE_CURVE ( 2, ( #33757, #56653, #45583, #11951, #17831, #34476, #57004, #40392, #1241 ),
 .UNSPECIFIED., .F., .F. ) 
 B_SPLINE_CURVE_WITH_KNOTS ( ( 3, 2, 2, 2, 3 ),
 ( 0.4305555555555555802, 0.4351851851851851749, 0.4444444444444444198, 0.4537037037037037202, 0.4583333333333333703 ),
 .UNSPECIFIED. ) 
 CURVE ( )  GEOMETRIC_REPRESENTATION_ITEM ( )  RATIONAL_B_SPLINE_CURVE ( ( 0.9330127018922194093, 0.9330127018922197424, 1.000000000000000000, 0.8660254037844387076, 1.000000000000000000, 0.8660254037844387076, 1.000000000000000000, 0.9330127018922189652, 0.9330127018922194093 ) ) 
 REPRESENTATION_ITEM ( '' )  );
#26811 = CARTESIAN_POINT ( 'NONE',  ( 22.92187500061451644, 3.027376345333613106, -5.243569643749998122 ) ) ;
#26812 = EDGE_LOOP ( 'NONE', ( #47655, #12826, #5214, #65209 ) ) ;
#26813 = DIRECTION ( 'NONE',  ( -0.000000000000000000, -1.000000000000000000, -0.000000000000000000 ) ) ;
#26814 = CARTESIAN_POINT ( 'NONE',  ( 9.928125000614517859, 4.541064518000418104, 2.621784821874999949 ) ) ;
#26815 = DIRECTION ( 'NONE',  ( -1.000000000000000000, -0.000000000000000000, -0.000000000000000000 ) ) ;
#26816 = CARTESIAN_POINT ( 'NONE',  ( 13.73437500061451644, -2.746126346562642428, -4.756430356249999214 ) ) ;
#26817 = CARTESIAN_POINT ( 'NONE',  ( 26.24062500061451431, -3.027376345333614438, 5.243569643749998122 ) ) ;
#26818 = CARTESIAN_POINT ( 'NONE',  ( 18.22499999999999787, 4.330127018922191873, 2.499999999999999556 ) ) ;
#26819 = CARTESIAN_POINT ( 'NONE',  ( 24.63749999999999574, -2.886751345948129988, 4.999999999999997335 ) ) ;
#26820 = CARTESIAN_POINT ( 'NONE',  ( 2.121784821874999061, 19.20312500061451644, 26.32496088578401583 ) ) ;
#26821 = CARTESIAN_POINT ( 'NONE',  ( 5.821875000614519458, 3.027376345333613106, -5.243569643749998122 ) ) ;
#26822 = CARTESIAN_POINT ( 'NONE',  ( 17.10937500061451999, 4.541064518000418104, -2.621784821874998173 ) ) ;
#26823 = CARTESIAN_POINT ( 'NONE',  ( 29.29687500061451644, 6.054752690667223547, 3.707466751127219781E-16 ) ) ;
#26824 = VERTEX_POINT ( 'NONE', #3571 ) ;
#26825 = CARTESIAN_POINT ( 'NONE',  ( 25.75312500061451715, 0.000000000000000000, 5.243569643749999010 ) ) ;
#26826 = CARTESIAN_POINT ( 'NONE',  ( 28.77187500061451431, 3.027376345333613106, -5.243569643749998122 ) ) ;
#26827 = CARTESIAN_POINT ( 'NONE',  ( -1.999999999999999112, 14.84374999877096712, 26.53589838486224650 ) ) ;
#26828 = CARTESIAN_POINT ( 'NONE',  ( 12.90000000000000213, 0.000000000000000000, 4.999999999999998224 ) ) ;
#26829 = CARTESIAN_POINT ( 'NONE',  ( 11.31562500061451892, 3.027376345333611329, 5.243569643749999010 ) ) ;
#26830 = LINE ( 'NONE', #72983, #25418 ) ;
#26831 = CARTESIAN_POINT ( 'NONE',  ( 19.50000000000000000, 4.330127018922192761, -2.499999999999997780 ) ) ;
#26832 = CARTESIAN_POINT ( 'NONE',  ( 29.39062500061451644, -3.027376345333614438, 5.243569643749998122 ) ) ;
#26833 = CARTESIAN_POINT ( 'NONE',  ( 16.16250000122903430, 0.000000000000000000, 4.999999999999998224 ) ) ;
#26834 = CARTESIAN_POINT ( 'NONE',  ( 26.98125000122903216, -4.330127018922194537, 2.499999999999995559 ) ) ;
#26835 = CARTESIAN_POINT ( 'NONE',  ( 15.72187500061451892, 2.746126346562645981, -4.756430356249997438 ) ) ;
#26836 = CARTESIAN_POINT ( 'NONE',  ( 4.903125000614516615, 4.541064518000418104, -2.621784821874998173 ) ) ;
#26837 = CARTESIAN_POINT ( 'NONE',  ( 20.70937500061451786, 4.541064518000418104, -2.621784821874998173 ) ) ;
#26838 = CARTESIAN_POINT ( 'NONE',  ( 2.121784821875001281, 15.95937500061451608, 33.67503911421598417 ) ) ;
#26839 = CARTESIAN_POINT ( 'NONE',  ( 20.55937500061451573, -4.541064518000417216, -2.621784821875001281 ) ) ;
#26840 = CARTESIAN_POINT ( 'NONE',  ( 28.77187500061451431, 3.027376345333613106, -5.243569643749998122 ) ) ;
#26841 = CARTESIAN_POINT ( 'NONE',  ( -3.000416591977282496E-16, 19.29687500061451644, 25.09994784771203058 ) ) ;
#26842 = CARTESIAN_POINT ( 'NONE',  ( 12.36562500061451608, -6.054752690667223547, -1.112240025338166033E-15 ) ) ;
#26843 = CARTESIAN_POINT ( 'NONE',  ( 4.312500001229034652, 4.330127018922192761, -2.499999999999997780 ) ) ;
#26844 = EDGE_CURVE ( 'NONE', #13883, #35438, #68301, .T. ) ;
#26845 = CARTESIAN_POINT ( 'NONE',  ( 7.096875000614517148, -3.027376345333610441, -5.243569643749999898 ) ) ;
#26846 = CARTESIAN_POINT ( 'NONE',  ( 3.882866153107933371, 3.150134987115559060, -3.987202789055975582 ) ) ;
#26847 = CARTESIAN_POINT ( 'NONE',  ( 8.953125000614518214, 4.541064518000418104, -2.621784821874998173 ) ) ;
#26848 = CARTESIAN_POINT ( 'NONE',  ( 13.65937500061451715, 0.000000000000000000, 5.243569643749999010 ) ) ;
#26849 = CARTESIAN_POINT ( 'NONE',  ( 24.58125000122903003, 4.330127018922191873, 2.499999999999999556 ) ) ;
#26850 = CARTESIAN_POINT ( 'NONE',  ( 22.01250000122903216, 0.000000000000000000, 4.999999999999998224 ) ) ;
#26851 = CARTESIAN_POINT ( 'NONE',  ( 8.484375000614518214, 6.421520780324663323E-16, -5.243569643749999010 ) ) ;
#26852 = CARTESIAN_POINT ( 'NONE',  ( 12.59062500061451573, 6.054752690667223547, 3.707466751127219781E-16 ) ) ;
#26853 = CARTESIAN_POINT ( 'NONE',  ( 25.14375000122903003, -2.886751345948129988, 4.999999999999997335 ) ) ;
#26854 = CARTESIAN_POINT ( 'NONE',  ( 22.54687500061451999, 6.054752690667223547, 3.707466751127219781E-16 ) ) ;
#26855 = CARTESIAN_POINT ( 'NONE',  ( 26.79375000122903216, 5.773502691896255534, 3.535250795749688401E-16 ) ) ;
#26856 = CARTESIAN_POINT ( 'NONE',  ( -3.964499721297434665, 3.046849790701494420, 29.45062293401495879 ) ) ;
#26857 = VECTOR ( 'NONE', #10161, 1000.000000000000000 ) ;
#26858 = CARTESIAN_POINT ( 'NONE',  ( 8.287499999999999645, 5.773502691896255534, 3.535250795749688401E-16 ) ) ;
#26859 = CARTESIAN_POINT ( 'NONE',  ( 4.243569643749999010, 11.57187500061451679, -32.45002607614398471 ) ) ;
#26860 = CARTESIAN_POINT ( 'NONE',  ( 14.43750000122903288, -4.330127018922194537, 2.499999999999995559 ) ) ;
#26861 = CARTESIAN_POINT ( 'NONE',  ( 9.001249775931846008E-16, 15.86562500061451608, -25.09994784771203058 ) ) ;
#26862 = CARTESIAN_POINT ( 'NONE',  ( 16.53750000122903430, 4.330127018922191873, 2.499999999999999556 ) ) ;
#26863 = CARTESIAN_POINT ( 'NONE',  ( 10.00312500061451715, 0.000000000000000000, 5.243569643749999010 ) ) ;
#26864 = ORIENTED_EDGE ( 'NONE', *, *, #48137, .T. ) ;
#26865 = CARTESIAN_POINT ( 'NONE',  ( 13.87500000000000178, -4.330127018922194537, 2.499999999999995559 ) ) ;
#26866 = CARTESIAN_POINT ( 'NONE',  ( 23.75625000122903074, 0.000000000000000000, 4.999999999999998224 ) ) ;
#26867 = CARTESIAN_POINT ( 'NONE',  ( 23.27812500061451573, 6.421520780324663323E-16, -5.243569643749999010 ) ) ;
#26868 = CARTESIAN_POINT ( 'NONE',  ( 11.07187500061451679, -6.054752690667223547, -1.112240025338166033E-15 ) ) ;
#26869 = CARTESIAN_POINT ( 'NONE',  ( 4.390052511545366798, -2.393233949706693675, -4.665573943098876519 ) ) ;
#26870 = CARTESIAN_POINT ( 'NONE',  ( 11.28750000122903252, -4.330127018922194537, 2.499999999999995559 ) ) ;
#26871 = CARTESIAN_POINT ( 'NONE',  ( 18.93750000122903288, -4.330127018922194537, 2.499999999999995559 ) ) ;
#26872 =( BOUNDED_CURVE ( )  B_SPLINE_CURVE ( 2, ( #34676, #29147, #51682, #1086, #59019, #13961, #64572 ),
 .UNSPECIFIED., .F., .F. ) 
 B_SPLINE_CURVE_WITH_KNOTS ( ( 3, 2, 2, 3 ),
 ( 0.4666666666666667296, 0.4694444444444444975, 0.4722222222222222654, 0.4750000000000000333 ),
 .UNSPECIFIED. ) 
 CURVE ( )  GEOMETRIC_REPRESENTATION_ITEM ( )  RATIONAL_B_SPLINE_CURVE ( ( 0.9999999999999973355, 0.8660254037844413721, 1.000000000000000000, 0.8660254037844387076, 1.000000000000000000, 0.8660254037844360431, 1.000000000000002665 ) ) 
 REPRESENTATION_ITEM ( '' )  );
#26873 = CARTESIAN_POINT ( 'NONE',  ( 15.62812500061451537, 6.421520780324663323E-16, -5.243569643749999010 ) ) ;
#26874 = CARTESIAN_POINT ( 'NONE',  ( 18.17812500061451786, -4.541064518000419881, 2.621784821874995952 ) ) ;
#26875 = CARTESIAN_POINT ( 'NONE',  ( 25.23750000122903359, -4.330127018922194537, 2.499999999999995559 ) ) ;
#26876 =( BOUNDED_CURVE ( )  B_SPLINE_CURVE ( 2, ( #12838, #35372, #46106, #58254, #57895, #7303, #29834 ),
 .UNSPECIFIED., .F., .F. ) 
 B_SPLINE_CURVE_WITH_KNOTS ( ( 3, 2, 2, 3 ),
 ( 0.2999999999999999889, 0.3033333333333333437, 0.3066666666666666430, 0.3099999999999999978 ),
 .UNSPECIFIED. ) 
 CURVE ( )  GEOMETRIC_REPRESENTATION_ITEM ( )  RATIONAL_B_SPLINE_CURVE ( ( 1.000000000000000000, 0.8660254037844387076, 1.000000000000000000, 0.8660254037844387076, 1.000000000000000000, 0.8660254037844387076, 1.000000000000000000 ) ) 
 REPRESENTATION_ITEM ( '' )  );
#26877 = CARTESIAN_POINT ( 'NONE',  ( 28.83750000122903145, -4.330127018922194537, 2.499999999999995559 ) ) ;
#26878 = CARTESIAN_POINT ( 'NONE',  ( 25.57499999999999929, -4.330127018922194537, 2.499999999999995559 ) ) ;
#26879 = CARTESIAN_POINT ( 'NONE',  ( -7.967954043666661671E-16, 13.42812499938548321, 34.33755215474603517 ) ) ;
#26880 = CARTESIAN_POINT ( 'NONE',  ( 26.55937500061451573, 4.541064518000418104, -2.621784821874998173 ) ) ;
#26881 = LINE ( 'NONE', #42405, #72473 ) ;
#26882 = CARTESIAN_POINT ( 'NONE',  ( 13.20000000122903394, -2.886751345948125991, -5.000000000000000000 ) ) ;
#26883 = CARTESIAN_POINT ( 'NONE',  ( 4.237500000000001599, 5.773502691896255534, 3.535250795749688894E-16 ) ) ;
#26884 = EDGE_CURVE ( 'NONE', #100, #32704, #61933, .T. ) ;
#26885 = CARTESIAN_POINT ( 'NONE',  ( -2.498395430326213790E-14, 20.26249999999999929, 26.00000000000000000 ) ) ;
#26886 =( BOUNDED_CURVE ( )  B_SPLINE_CURVE ( 2, ( #36254, #7451, #13712, #52519, #25904, #63956, #18519 ),
 .UNSPECIFIED., .F., .F. ) 
 B_SPLINE_CURVE_WITH_KNOTS ( ( 3, 2, 2, 3 ),
 ( 0.2800000000000000266, 0.2833333333333333259, 0.2866666666666667362, 0.2900000000000000355 ),
 .UNSPECIFIED. ) 
 CURVE ( )  GEOMETRIC_REPRESENTATION_ITEM ( )  RATIONAL_B_SPLINE_CURVE ( ( 1.000000000000000000, 0.8660254037844387076, 1.000000000000000000, 0.8660254037844387076, 1.000000000000000000, 0.8660254037844364872, 1.000000000000002220 ) ) 
 REPRESENTATION_ITEM ( '' )  );
#26887 = CARTESIAN_POINT ( 'NONE',  ( 8.334375000614516082, -4.541064518000419881, 2.621784821874995952 ) ) ;
#26888 = CARTESIAN_POINT ( 'NONE',  ( 25.82812500061451644, -4.541064518000419881, 2.621784821874995952 ) ) ;
#26889 = LINE ( 'NONE', #43512, #71972 ) ;
#26890 = CARTESIAN_POINT ( 'NONE',  ( 22.50000000000000000, -4.330127018922190985, -2.500000000000001332 ) ) ;
#26891 = CARTESIAN_POINT ( 'NONE',  ( 9.834375000614517859, 6.421520780324663323E-16, -5.243569643749999010 ) ) ;
#26892 = DIRECTION ( 'NONE',  ( 0.000000000000000000, 0.000000000000000000, 1.000000000000000000 ) ) ;
#26893 = CARTESIAN_POINT ( 'NONE',  ( 28.94062500061452070, -3.027376345333614438, 5.243569643749998122 ) ) ;
#26894 = CARTESIAN_POINT ( 'NONE',  ( 8.521875000614516082, 3.027376345333613106, -5.243569643749998122 ) ) ;
#26895 = CARTESIAN_POINT ( 'NONE',  ( 29.55937500061451573, -4.541064518000417216, -2.621784821875001281 ) ) ;
#26896 = VECTOR ( 'NONE', #24187, 1000.000000000000000 ) ;
#26897 = CARTESIAN_POINT ( 'NONE',  ( -4.243569643749999898, 12.15312500061459211, 30.00000000000000000 ) ) ;
#26898 = CARTESIAN_POINT ( 'NONE',  ( 21.33749999999999858, 5.773502691896255534, 3.535250795749688894E-16 ) ) ;
#26899 = EDGE_LOOP ( 'NONE', ( #9688, #40175, #15552, #56565 ) ) ;
#26900 = CARTESIAN_POINT ( 'NONE',  ( 20.66250000122903074, 0.000000000000000000, 4.999999999999998224 ) ) ;
#26901 = CARTESIAN_POINT ( 'NONE',  ( 3.712499999999999911, 2.886751345948129099, -4.999999999999998224 ) ) ;
#26902 = VERTEX_POINT ( 'NONE', #54174 ) ;
#26903 = CARTESIAN_POINT ( 'NONE',  ( 17.95312500061451644, 4.541064518000418104, -2.621784821874998173 ) ) ;
#26904 = CARTESIAN_POINT ( 'NONE',  ( 11.61562500061451608, 3.027376345333613106, -5.243569643749998122 ) ) ;
#26905 = CARTESIAN_POINT ( 'NONE',  ( 22.54687500061451644, 0.000000000000000000, 4.756430356249998326 ) ) ;
#26906 = CARTESIAN_POINT ( 'NONE',  ( 6.946875000614517681, -3.027376345333614438, 5.243569643749998122 ) ) ;
#26907 = CARTESIAN_POINT ( 'NONE',  ( 19.46250000122903145, -4.330127018922190985, -2.500000000000001332 ) ) ;
#26908 = CARTESIAN_POINT ( 'NONE',  ( 15.71250000000000036, -5.773502691896255534, -1.060575238724906372E-15 ) ) ;
#26909 = CARTESIAN_POINT ( 'NONE',  ( 5.896875000614518747, 6.054752690667223547, 3.707466751127219781E-16 ) ) ;
#26910 = CARTESIAN_POINT ( 'NONE',  ( 14.37187500061451928, 3.027376345333613106, -5.243569643749998122 ) ) ;
#26911 = CARTESIAN_POINT ( 'NONE',  ( 24.72187500061451360, 3.027376345333613106, -5.243569643749998122 ) ) ;
#26912 = EDGE_CURVE ( 'NONE', #4778, #71509, #38266, .T. ) ;
#26913 = CYLINDRICAL_SURFACE ( 'NONE', #60753, 4.000000000000000000 ) ;
#26914 = ORIENTED_EDGE ( 'NONE', *, *, #40712, .T. ) ;
#26915 = CARTESIAN_POINT ( 'NONE',  ( 13.72500000000000142, 4.330127018922191873, 2.499999999999999556 ) ) ;
#26916 = CARTESIAN_POINT ( 'NONE',  ( 17.44687500061451857, -3.027376345333610441, -5.243569643749999898 ) ) ;
#26917 = CARTESIAN_POINT ( 'NONE',  ( 10.39687500061451786, 6.054752690667223547, 3.707466751127219781E-16 ) ) ;
#26918 = CARTESIAN_POINT ( 'NONE',  ( -7.967954043666661671E-16, 15.22812499938548214, 34.33755215474603517 ) ) ;
#26919 = CARTESIAN_POINT ( 'NONE',  ( 20.10000000000000142, 0.000000000000000000, 4.999999999999998224 ) ) ;
#26920 = CARTESIAN_POINT ( 'NONE',  ( 1.999999999999997335, 16.92500000000000071, 33.46410161513775705 ) ) ;
#26921 = CARTESIAN_POINT ( 'NONE',  ( -4.243569643749997233, 9.996875000614517504, -27.54997392385601174 ) ) ;
#26922 = CARTESIAN_POINT ( 'NONE',  ( 21.27187500061451786, 2.746126346562643317, 4.756430356249998326 ) ) ;
#26923 = CARTESIAN_POINT ( 'NONE',  ( 12.62812500061451537, 4.541064518000418104, 2.621784821874999949 ) ) ;
#26924 = CARTESIAN_POINT ( 'NONE',  ( 28.92187500061451644, 3.027376345333611329, 5.243569643749999010 ) ) ;
#26925 = CARTESIAN_POINT ( 'NONE',  ( 13.29375000122903394, 5.773502691896255534, 3.535250795749688401E-16 ) ) ;
#26926 = CARTESIAN_POINT ( 'NONE',  ( 29.07187500061451502, -6.054752690667223547, -1.112240025338166033E-15 ) ) ;
#26927 = CARTESIAN_POINT ( 'NONE',  ( 13.08750000000000036, -2.886751345948125991, -5.000000000000000000 ) ) ;
#26928 = CARTESIAN_POINT ( 'NONE',  ( 8.484601909799253346E-16, 17.97500000122903785, 34.61880215351700230 ) ) ;
#26929 = CARTESIAN_POINT ( 'NONE',  ( 11.28750000122903252, -4.330127018922194537, 2.499999999999995559 ) ) ;
#26930 = CARTESIAN_POINT ( 'NONE',  ( 23.29687500061451644, -3.027376345333610441, -5.243569643749999898 ) ) ;
#26931 = CARTESIAN_POINT ( 'NONE',  ( 17.63437500061451502, 4.541064518000418104, 2.621784821874999949 ) ) ;
#26932 = LINE ( 'NONE', #60519, #15929 ) ;
#26933 = EDGE_LOOP ( 'NONE', ( #35340, #3929, #54271, #31366 ) ) ;
#26934 = CARTESIAN_POINT ( 'NONE',  ( 17.46562500061451217, 3.027376345333613106, -5.243569643749998122 ) ) ;
#26935 = CARTESIAN_POINT ( 'NONE',  ( 28.35000000122903430, -2.886751345948129988, 4.999999999999997335 ) ) ;
#26936 = CARTESIAN_POINT ( 'NONE',  ( 15.19687500061451857, -3.027376345333610441, -5.243569643749999898 ) ) ;
#26937 = CARTESIAN_POINT ( 'NONE',  ( 5.948646956027292099, 8.038298999021534996, -29.19102198739167875 ) ) ;
#26938 = CARTESIAN_POINT ( 'NONE',  ( 20.27812500061451573, 4.541064518000418104, 2.621784821874999949 ) ) ;
#26939 = DIRECTION ( 'NONE',  ( -0.000000000000000000, -0.000000000000000000, -1.000000000000000000 ) ) ;
#26940 = CARTESIAN_POINT ( 'NONE',  ( 28.73437500061451644, 6.421520780324663323E-16, -5.243569643749999010 ) ) ;
#26941 = CARTESIAN_POINT ( 'NONE',  ( -3.000416591977282496E-16, 12.94062500061451537, 25.09994784771203058 ) ) ;
#26942 = CARTESIAN_POINT ( 'NONE',  ( 16.77187500061451786, 3.027376345333611329, 5.243569643749999010 ) ) ;
#26943 = CARTESIAN_POINT ( 'NONE',  ( 13.68750000122903288, 6.123233995736764310E-16, -4.999999999999998224 ) ) ;
#26944 = CARTESIAN_POINT ( 'NONE',  ( 9.721875000614517148, -5.492252693125287522, -1.008910452111647106E-15 ) ) ;
#26945 = CARTESIAN_POINT ( 'NONE',  ( 4.243569643749999898, 19.14687500061451431, -27.54997392385601529 ) ) ;
#26946 = CARTESIAN_POINT ( 'NONE',  ( 20.07187500061451857, -6.054752690667223547, -1.112240025338166033E-15 ) ) ;
#26947 = CARTESIAN_POINT ( 'NONE',  ( 21.37500000122902932, 2.886751345948129099, -4.999999999999998224 ) ) ;
#26948 = CARTESIAN_POINT ( 'NONE',  ( 17.37187500061451573, -6.054752690667223547, -1.112240025338166033E-15 ) ) ;
#26949 = CARTESIAN_POINT ( 'NONE',  ( 12.10312500061451857, 4.541064518000418104, -2.621784821874998173 ) ) ;
#26950 = CARTESIAN_POINT ( 'NONE',  ( -4.243569643749999898, 15.32187500061451679, 27.54997392385601529 ) ) ;
#26951 = CARTESIAN_POINT ( 'NONE',  ( 18.44062500061451715, 6.054752690667223547, 3.707466751127219781E-16 ) ) ;
#26952 = VERTEX_POINT ( 'NONE', #70431 ) ;
#26953 = CARTESIAN_POINT ( 'NONE',  ( 23.17500000000000071, 4.330127018922191873, 2.499999999999999556 ) ) ;
#26954 = CARTESIAN_POINT ( 'NONE',  ( 4.243569643749999010, 18.77187500061451786, -32.45002607614398471 ) ) ;
#26955 = CARTESIAN_POINT ( 'NONE',  ( 3.843527511662434559, -3.198147656327572808, -4.075615451639215792 ) ) ;
#26956 = CARTESIAN_POINT ( 'NONE',  ( 23.54062500061451146, -3.027376345333614438, 5.243569643749998122 ) ) ;
#26957 = CARTESIAN_POINT ( 'NONE',  ( 6.403125000614517504, 0.000000000000000000, 5.243569643749999010 ) ) ;
#26958 = CARTESIAN_POINT ( 'NONE',  ( 18.45000000122903216, -2.886751345948129988, 4.999999999999997335 ) ) ;
#26959 = CARTESIAN_POINT ( 'NONE',  ( 23.50312500061451360, 0.000000000000000000, 5.243569643749999010 ) ) ;
#26960 = CARTESIAN_POINT ( 'NONE',  ( 23.09999999999999787, 4.330127018922192761, -2.499999999999997780 ) ) ;
#26961 = CARTESIAN_POINT ( 'NONE',  ( 25.82812500061451644, -4.541064518000419881, 2.621784821874995952 ) ) ;
#26962 = CARTESIAN_POINT ( 'NONE',  ( 4.565625000614516260, 3.027376345333611329, 5.243569643749999010 ) ) ;
#26963 = ORIENTED_EDGE ( 'NONE', *, *, #63735, .F. ) ;
#26964 = CARTESIAN_POINT ( 'NONE',  ( 24.06562500061451715, -6.054752690667223547, -1.112240025338166033E-15 ) ) ;
#26965 = CARTESIAN_POINT ( 'NONE',  ( 3.328125000614516438, -4.541064518000419881, 2.621784821874995952 ) ) ;
#26966 = CARTESIAN_POINT ( 'NONE',  ( 10.77187500061451786, 2.746126346562645981, -4.756430356249997438 ) ) ;
#26967 = CARTESIAN_POINT ( 'NONE',  ( 1.071796769724489895, 18.96740381056766722, 26.00000000000000355 ) ) ;
#26968 = CARTESIAN_POINT ( 'NONE',  ( 4.000000000000000000, 14.00000000122903288, -27.69059892324149530 ) ) ;
#26969 = CARTESIAN_POINT ( 'NONE',  ( -4.243569643749999898, 19.82187500061451857, -32.45002607614398471 ) ) ;
#26970 = CARTESIAN_POINT ( 'NONE',  ( 10.87500000000000000, 6.123233995736764310E-16, -4.999999999999998224 ) ) ;
#26971 = EDGE_CURVE ( 'NONE', #49631, #9585, #60794, .T. ) ;
#26972 = CARTESIAN_POINT ( 'NONE',  ( 10.65937500061451715, -4.541064518000417216, -2.621784821875001281 ) ) ;
#26973 = CARTESIAN_POINT ( 'NONE',  ( 7.425000001229034474, 2.886751345948129099, -4.999999999999998224 ) ) ;
#26974 = CARTESIAN_POINT ( 'NONE',  ( 13.92187500061451644, 3.027376345333613106, -5.243569643749998122 ) ) ;
#26975 = CARTESIAN_POINT ( 'NONE',  ( 5.071875000614519458, 3.027376345333611329, 5.243569643749999010 ) ) ;
#26976 = CARTESIAN_POINT ( 'NONE',  ( 25.72499999999999787, 6.123233995736764310E-16, -4.999999999999998224 ) ) ;
#26977 = CARTESIAN_POINT ( 'NONE',  ( 0.000000000000000000, 20.00000000000000000, -30.00000000000000000 ) ) ;
#26979 = EDGE_CURVE ( 'NONE', #29126, #27766, #70650, .T. ) ;
#26978 = CARTESIAN_POINT ( 'NONE',  ( 11.82187500061451679, 3.027376345333611329, 5.243569643749999010 ) ) ;
#26980 = CYLINDRICAL_SURFACE ( 'NONE', #1771, 4.999999999999998224 ) ;
#26981 = CARTESIAN_POINT ( 'NONE',  ( 20.95312500061451999, -4.541064518000417216, -2.621784821875001281 ) ) ;
#26982 = CARTESIAN_POINT ( 'NONE',  ( 16.61250000000000071, -5.773502691896255534, -1.060575238724906372E-15 ) ) ;
#26983 = CARTESIAN_POINT ( 'NONE',  ( 9.001249775931846008E-16, 19.01562500061459104, 34.90005215228797653 ) ) ;
#26984 = CARTESIAN_POINT ( 'NONE',  ( 22.80937500061451573, -4.541064518000417216, -2.621784821875001281 ) ) ;
#26985 = EDGE_CURVE ( 'NONE', #21477, #62607, #45653, .T. ) ;
#26986 = FACE_OUTER_BOUND ( 'NONE', #35744, .T. ) ;
#26987 = CARTESIAN_POINT ( 'NONE',  ( 29.47500000122903430, 2.886751345948129099, -4.999999999999998224 ) ) ;
#26988 = CARTESIAN_POINT ( 'NONE',  ( 20.82187500061451502, -4.119189519843968306, 2.378215178124996054 ) ) ;
#26989 = CARTESIAN_POINT ( 'NONE',  ( 24.36562500061451786, 3.027376345333611329, 5.243569643749999010 ) ) ;
#26990 = CARTESIAN_POINT ( 'NONE',  ( 17.01562500061451644, 3.027376345333613106, -5.243569643749998122 ) ) ;
#26991 = CARTESIAN_POINT ( 'NONE',  ( 13.85625000122903216, 0.000000000000000000, 4.999999999999998224 ) ) ;
#26992 = CARTESIAN_POINT ( 'NONE',  ( 15.15937500061451715, -4.541064518000417216, -2.621784821875001281 ) ) ;
#26993 = CARTESIAN_POINT ( 'NONE',  ( -1.999999999999999112, 15.80000000000000071, 26.53589838486224650 ) ) ;
#26994 = CARTESIAN_POINT ( 'NONE',  ( 28.42500000122904069, -5.773502691896255534, -1.060575238724906372E-15 ) ) ;
#26995 = CARTESIAN_POINT ( 'NONE',  ( 7.059375000614518392, -4.541064518000417216, -2.621784821875001281 ) ) ;
#26996 = CARTESIAN_POINT ( 'NONE',  ( 14.07187500061451679, 3.027376345333611329, 5.243569643749999010 ) ) ;
#26997 = CARTESIAN_POINT ( 'NONE',  ( 4.849242802210273595, -1.218730718756773967, -5.100017238597982505 ) ) ;
#26998 = CARTESIAN_POINT ( 'NONE',  ( 4.462500001229035007, 0.000000000000000000, 4.999999999999998224 ) ) ;
#26999 = CARTESIAN_POINT ( 'NONE',  ( 25.95937500061451431, -4.541064518000417216, -2.621784821875001281 ) ) ;
#27000 = CARTESIAN_POINT ( 'NONE',  ( 17.82187500061451502, -6.054752690667223547, -1.112240025338166033E-15 ) ) ;
#27001 = CARTESIAN_POINT ( 'NONE',  ( -3.756430356250001434, 14.81562499938548250, 32.16877607737301048 ) ) ;
#27002 = CARTESIAN_POINT ( 'NONE',  ( 28.53749999999999787, 5.773502691896255534, 3.535250795749688894E-16 ) ) ;
#27003 = CARTESIAN_POINT ( 'NONE',  ( 5.850000000000001421, -4.330127018922190985, -2.500000000000001332 ) ) ;
#27004 = CARTESIAN_POINT ( 'NONE',  ( 28.58437500061451786, -4.119189519843968306, 2.378215178124996054 ) ) ;
#27005 = CARTESIAN_POINT ( 'NONE',  ( 18.96562500061451573, 3.027376345333611329, 5.243569643749999010 ) ) ;
#27006 = CARTESIAN_POINT ( 'NONE',  ( 8.737500000000002487, 5.773502691896255534, 3.535250795749688894E-16 ) ) ;
#27007 = CARTESIAN_POINT ( 'NONE',  ( 4.865625000614517859, 3.027376345333613106, -5.243569643749998122 ) ) ;
#27008 = CARTESIAN_POINT ( 'NONE',  ( 20.54999999999999716, 0.000000000000000000, 4.999999999999998224 ) ) ;
#27009 = CARTESIAN_POINT ( 'NONE',  ( 3.807538167735159185, -3.240779705755961526, 4.122180188640082399 ) ) ;
#27010 = CARTESIAN_POINT ( 'NONE',  ( 22.12500000122903288, -5.773502691896255534, -1.060575238724906372E-15 ) ) ;
#27011 = CARTESIAN_POINT ( 'NONE',  ( 0.8036833610285047946, 9.975469519845873378, 35.95937231738776063 ) ) ;
#27012 = CARTESIAN_POINT ( 'NONE',  ( 3.000000000000002665, 0.000000000000000000, 4.999999999999998224 ) ) ;
#27013 = VERTEX_POINT ( 'NONE', #22368 ) ;
#27014 = CARTESIAN_POINT ( 'NONE',  ( 16.82812500061451644, -4.541064518000419881, 2.621784821874995952 ) ) ;
#27015 = CARTESIAN_POINT ( 'NONE',  ( 23.20312500061451644, -4.541064518000417216, -2.621784821875001281 ) ) ;
#27016 = CARTESIAN_POINT ( 'NONE',  ( 24.42187500061451999, 3.027376345333611329, 5.243569643749999010 ) ) ;
#27017 = CARTESIAN_POINT ( 'NONE',  ( 6.899999999999999467, 4.330127018922192761, -2.499999999999997780 ) ) ;
#27018 = CARTESIAN_POINT ( 'NONE',  ( 10.71562500061451928, 3.027376345333613106, -5.243569643749998122 ) ) ;
#27019 = CARTESIAN_POINT ( 'NONE',  ( 26.46562500061451573, 3.027376345333613106, -5.243569643749998122 ) ) ;
#27020 = CARTESIAN_POINT ( 'NONE',  ( 15.00937500061451679, 0.000000000000000000, 5.243569643749999010 ) ) ;
#27021 = CARTESIAN_POINT ( 'NONE',  ( 19.32187500061451857, 3.027376345333613106, -5.243569643749998122 ) ) ;
#27022 = LINE ( 'NONE', #22194, #62701 ) ;
#27023 = CARTESIAN_POINT ( 'NONE',  ( -3.000416591977282496E-16, 19.69062500061451360, 25.09994784771203058 ) ) ;
#27024 = EDGE_CURVE ( 'NONE', #58126, #56216, #7866, .T. ) ;
#27025 = CARTESIAN_POINT ( 'NONE',  ( 24.93750000122903288, 6.123233995736764310E-16, -4.999999999999998224 ) ) ;
#27026 = CARTESIAN_POINT ( 'NONE',  ( 17.93437500061451928, 5.824947211148865298E-16, -4.756430356249998326 ) ) ;
#27027 = CARTESIAN_POINT ( 'NONE',  ( 11.84062500061451573, -3.027376345333614438, 5.243569643749998122 ) ) ;
#27028 = CARTESIAN_POINT ( 'NONE',  ( 9.084375000614517859, 4.541064518000418104, 2.621784821874999949 ) ) ;
#27029 = CARTESIAN_POINT ( 'NONE',  ( 7.209375000614519635, 4.541064518000418104, -2.621784821874998173 ) ) ;
#27030 = VERTEX_POINT ( 'NONE', #33817 ) ;
#27031 = CARTESIAN_POINT ( 'NONE',  ( 27.98437500061451289, 4.541064518000418104, 2.621784821874999949 ) ) ;
#27032 = CARTESIAN_POINT ( 'NONE',  ( 19.07812500061451644, -4.541064518000419881, 2.621784821874995952 ) ) ;
#27033 = CARTESIAN_POINT ( 'NONE',  ( 3.178125000614515638, 4.541064518000418104, 2.621784821874999949 ) ) ;
#27034 = CARTESIAN_POINT ( 'NONE',  ( 3.196875000614516793, 6.054752690667223547, 3.707466751127219781E-16 ) ) ;
#27035 = CARTESIAN_POINT ( 'NONE',  ( 24.08437500061451786, -4.541064518000419881, 2.621784821874995952 ) ) ;
#27036 = CARTESIAN_POINT ( 'NONE',  ( 19.75312500061451360, 4.541064518000418104, -2.621784821874998173 ) ) ;
#27037 = CARTESIAN_POINT ( 'NONE',  ( 3.999999999999999112, 11.22500000000000142, 30.00000000000000000 ) ) ;
#27038 = CARTESIAN_POINT ( 'NONE',  ( 25.41562500061451146, -6.054752690667223547, -1.112240025338166033E-15 ) ) ;
#27039 = CARTESIAN_POINT ( 'NONE',  ( 4.650000001229035895, -2.886751345948125991, -5.000000000000000000 ) ) ;
#27040 = ORIENTED_EDGE ( 'NONE', *, *, #34911, .F. ) ;
#27041 = CARTESIAN_POINT ( 'NONE',  ( 3.075000001229035718, 2.886751345948126879, 4.999999999999999112 ) ) ;
#27042 = CARTESIAN_POINT ( 'NONE',  ( -1.999999999999997113, 16.47500000000000142, -26.53589838486224295 ) ) ;
#27043 = CARTESIAN_POINT ( 'NONE',  ( -1.878215178124999163, 16.05312499938548143, 26.74683588394047007 ) ) ;
#27044 = CARTESIAN_POINT ( 'NONE',  ( 5.071875000614519458, 3.027376345333611329, 5.243569643749999010 ) ) ;
#27045 = CARTESIAN_POINT ( 'NONE',  ( 25.27499999999999858, 6.123233995736764310E-16, -4.999999999999998224 ) ) ;
#27046 = CARTESIAN_POINT ( 'NONE',  ( 13.37812500061451715, 6.421520780324663323E-16, -5.243569643749999010 ) ) ;
#27047 = CARTESIAN_POINT ( 'NONE',  ( 6.534375000614517148, -4.541064518000419881, 2.621784821874995952 ) ) ;
#27048 = CARTESIAN_POINT ( 'NONE',  ( 23.92500000122903359, -5.773502691896255534, -1.060575238724906372E-15 ) ) ;
#27049 = CARTESIAN_POINT ( 'NONE',  ( 13.99687500061451928, 6.054752690667223547, 3.707466751127219781E-16 ) ) ;
#27050 = CARTESIAN_POINT ( 'NONE',  ( 3.571875000614517237, 3.027376345333613106, -5.243569643749998122 ) ) ;
#27051 = CARTESIAN_POINT ( 'NONE',  ( 1.626862140677534273E-15, 18.76250000000000284, 34.00000000000000000 ) ) ;
#27052 = CARTESIAN_POINT ( 'NONE',  ( 2.953125000614516438, -4.541064518000417216, -2.621784821875001281 ) ) ;
#27053 = CARTESIAN_POINT ( 'NONE',  ( 14.95312500061451644, 0.000000000000000000, 5.243569643749999010 ) ) ;
#27054 = ORIENTED_EDGE ( 'NONE', *, *, #69433, .T. ) ;
#27055 = CARTESIAN_POINT ( 'NONE',  ( 10.64062500061451644, -3.027376345333610441, -5.243569643749999898 ) ) ;
#27056 = CARTESIAN_POINT ( 'NONE',  ( 7.715625000614515727, 3.027376345333611329, 5.243569643749999010 ) ) ;
#27057 = CARTESIAN_POINT ( 'NONE',  ( 19.77187500061451786, 2.746126346562645981, -4.756430356249997438 ) ) ;
#27058 = CARTESIAN_POINT ( 'NONE',  ( 9.525000000000002132, 6.123233995736764310E-16, -4.999999999999998224 ) ) ;
#27059 = CARTESIAN_POINT ( 'NONE',  ( 3.375000001229033320, 2.886751345948129099, -4.999999999999998224 ) ) ;
#27060 = CARTESIAN_POINT ( 'NONE',  ( 17.51249999999999929, -5.773502691896255534, -1.060575238724906372E-15 ) ) ;
#27061 = CARTESIAN_POINT ( 'NONE',  ( 18.45937500061451431, 4.541064518000418104, -2.621784821874998173 ) ) ;
#27062 = CARTESIAN_POINT ( 'NONE',  ( 14.10000000122903252, -2.886751345948125991, -5.000000000000000000 ) ) ;
#27063 = CARTESIAN_POINT ( 'NONE',  ( 19.87500000000000000, 6.123233995736764310E-16, -4.999999999999998224 ) ) ;
#27064 = CARTESIAN_POINT ( 'NONE',  ( 9.001249775931846008E-16, 16.31562500061451715, -25.09994784771203058 ) ) ;
#27065 = CARTESIAN_POINT ( 'NONE',  ( 20.69999999999999929, -4.330127018922190985, -2.500000000000001332 ) ) ;
#27066 = CARTESIAN_POINT ( 'NONE',  ( 28.86562500061451786, 3.027376345333611329, 5.243569643749999010 ) ) ;
#27067 =( NAMED_UNIT ( * ) SI_UNIT ( $, .STERADIAN. ) SOLID_ANGLE_UNIT ( ) );
#27068 = DIRECTION ( 'NONE',  ( -1.000000000000000000, -0.000000000000000000, -0.000000000000000000 ) ) ;
#27069 = CARTESIAN_POINT ( 'NONE',  ( 13.02187500061451608, 3.027376345333613106, -5.243569643749998122 ) ) ;
#27070 = ADVANCED_FACE ( 'NONE', ( #16819 ), #72625, .F. ) ;
#27071 = CARTESIAN_POINT ( 'NONE',  ( 26.92499999999999716, -4.330127018922194537, 2.499999999999995559 ) ) ;
#27072 = CARTESIAN_POINT ( 'NONE',  ( 10.30312500061451431, 4.541064518000418104, -2.621784821874998173 ) ) ;
#27073 = CARTESIAN_POINT ( 'NONE',  ( 27.23437500061450933, -2.746126346562642428, -4.756430356249999214 ) ) ;
#27074 = CARTESIAN_POINT ( 'NONE',  ( 21.87187500061451573, -6.054752690667223547, -1.112240025338166033E-15 ) ) ;
#27075 = CARTESIAN_POINT ( 'NONE',  ( 12.79687500061451466, -4.119189519843965641, -2.378215178125001383 ) ) ;
#27076 = CARTESIAN_POINT ( 'NONE',  ( 8.653125000614515727, 0.000000000000000000, 5.243569643749999010 ) ) ;
#27077 = CARTESIAN_POINT ( 'NONE',  ( 13.17187500061451999, 3.027376345333611329, 5.243569643749999010 ) ) ;
#27078 = VERTEX_POINT ( 'NONE', #33451 ) ;
#27079 = CARTESIAN_POINT ( 'NONE',  ( 22.65937500061451715, 0.000000000000000000, 5.243569643749999010 ) ) ;
#27080 = CARTESIAN_POINT ( 'NONE',  ( 0.2755985575760799833, 4.994312242614637576, -26.00710267647355778 ) ) ;
#27081 = DIRECTION ( 'NONE',  ( -1.000000000000000000, -0.000000000000000000, -0.000000000000000000 ) ) ;
#27082 = CARTESIAN_POINT ( 'NONE',  ( 5.662500000000000533, 2.886751345948126879, 4.999999999999999112 ) ) ;
#27083 = CARTESIAN_POINT ( 'NONE',  ( 16.42500000122903359, 2.886751345948129099, -4.999999999999998224 ) ) ;
#27084 = CARTESIAN_POINT ( 'NONE',  ( 16.78125000122903288, 6.123233995736764310E-16, -4.999999999999998224 ) ) ;
#27085 = CARTESIAN_POINT ( 'NONE',  ( -2.556497649636125342E-15, 19.21250000000000213, -26.00000000000000000 ) ) ;
#27086 = ORIENTED_EDGE ( 'NONE', *, *, #38503, .T. ) ;
#27087 = CARTESIAN_POINT ( 'NONE',  ( 13.04999999999999893, -4.330127018922190985, -2.500000000000001332 ) ) ;
#27088 = CARTESIAN_POINT ( 'NONE',  ( 15.75000000000000000, -4.330127018922190985, -2.500000000000001332 ) ) ;
#27089 = CARTESIAN_POINT ( 'NONE',  ( 13.46250000122903323, 0.000000000000000000, 4.999999999999998224 ) ) ;
#27090 = CARTESIAN_POINT ( 'NONE',  ( 10.64062500061451644, -3.027376345333610441, -5.243569643749999898 ) ) ;
#27091 =( BOUNDED_CURVE ( )  B_SPLINE_CURVE ( 2, ( #28245, #55591, #179, #54858, #22684, #45235, #67768, #4267, #71857 ),
 .UNSPECIFIED., .F., .F. ) 
 B_SPLINE_CURVE_WITH_KNOTS ( ( 3, 2, 2, 2, 3 ),
 ( 0.09782608695652174335, 0.1014492753623188470, 0.1086956521739130405, 0.1159420289855072478, 0.1195652173913043514 ),
 .UNSPECIFIED. ) 
 CURVE ( )  GEOMETRIC_REPRESENTATION_ITEM ( )  RATIONAL_B_SPLINE_CURVE ( ( 0.9330127018922194093, 0.9330127018922194093, 1.000000000000000000, 0.8660254037844387076, 1.000000000000000000, 0.8660254037844387076, 1.000000000000000000, 0.9330127018922194093, 0.9330127018922194093 ) ) 
 REPRESENTATION_ITEM ( '' )  );
#27092 = ORIENTED_EDGE ( 'NONE', *, *, #6241, .F. ) ;
#27093 = CYLINDRICAL_SURFACE ( 'NONE', #48956, 4.999999999999998224 ) ;
#27094 = CARTESIAN_POINT ( 'NONE',  ( -4.243569643749997233, 15.39687500061451786, -27.54997392385601174 ) ) ;
#27095 = CARTESIAN_POINT ( 'NONE',  ( 3.665625000614517681, 3.027376345333611329, 5.243569643749999010 ) ) ;
#27096 = CARTESIAN_POINT ( 'NONE',  ( 3.756430356249998770, 15.75312499938548427, 32.16877607737301759 ) ) ;
#27097 = CARTESIAN_POINT ( 'NONE',  ( 10.91250000000000320, 2.886751345948129099, -4.999999999999998224 ) ) ;
#27098 = CARTESIAN_POINT ( 'NONE',  ( 3.100832673336169520, 3.922389953441107302, 3.244276004801022850 ) ) ;
#27099 = ORIENTED_EDGE ( 'NONE', *, *, #57008, .T. ) ;
#27100 = CARTESIAN_POINT ( 'NONE',  ( 23.12812500061451360, -4.541064518000419881, 2.621784821874995952 ) ) ;
#27101 = CARTESIAN_POINT ( 'NONE',  ( 29.36250000000000782, 2.886751345948158409, -4.999999999999947597 ) ) ;
#27102 = CARTESIAN_POINT ( 'NONE',  ( 1.878215178124997609, 19.76562499938548356, 33.25316411605952993 ) ) ;
#27103 = CARTESIAN_POINT ( 'NONE',  ( 21.64687500061451786, 6.054752690667223547, 3.707466751127219781E-16 ) ) ;
#27104 = CARTESIAN_POINT ( 'NONE',  ( 18.29062500061451502, -3.027376345333610441, -5.243569643749999898 ) ) ;
#27105 = CARTESIAN_POINT ( 'NONE',  ( 4.243569643749999898, 13.72812500061459318, -30.00000000000000000 ) ) ;
#27106 = CARTESIAN_POINT ( 'NONE',  ( 6.178125000614518747, 6.421520780324663323E-16, -5.243569643749999010 ) ) ;
#27107 = CARTESIAN_POINT ( 'NONE',  ( 4.603125000614518569, 0.000000000000000000, 5.243569643749999010 ) ) ;
#27108 = CARTESIAN_POINT ( 'NONE',  ( 24.38437500061451502, 4.119189519843966529, 2.378215178124999607 ) ) ;
#27109 = CARTESIAN_POINT ( 'NONE',  ( 21.02812500061451573, 6.421520780324663323E-16, -5.243569643749999010 ) ) ;
#27110 = CARTESIAN_POINT ( 'NONE',  ( 8.859375000614518214, -4.119189519843965641, -2.378215178125001383 ) ) ;
#27111 = CARTESIAN_POINT ( 'NONE',  ( 1.878215178124997609, 17.51562499938548356, 33.25316411605952993 ) ) ;
#27112 = CARTESIAN_POINT ( 'NONE',  ( 14.59687500061452070, -3.027376345333614438, 5.243569643749998122 ) ) ;
#27113 = CARTESIAN_POINT ( 'NONE',  ( 14.44687500061451679, 6.054752690667223547, 3.707466751127219781E-16 ) ) ;
#27114 = CARTESIAN_POINT ( 'NONE',  ( 21.90937500061451715, -4.541064518000417216, -2.621784821875001281 ) ) ;
#27115 = ORIENTED_EDGE ( 'NONE', *, *, #52167, .F. ) ;
#27116 = CARTESIAN_POINT ( 'NONE',  ( -4.243569643749999898, 11.72187500061451892, 27.54997392385601529 ) ) ;
#27117 = CARTESIAN_POINT ( 'NONE',  ( 26.46562500061451573, 3.027376345333613106, -5.243569643749998122 ) ) ;
#27118 = CARTESIAN_POINT ( 'NONE',  ( 25.86562500061451431, -6.054752690667223547, -1.112240025338166033E-15 ) ) ;
#27119 = CARTESIAN_POINT ( 'NONE',  ( 1.592000809091587073E-14, 16.40000000122903501, -34.00000000000000000 ) ) ;
#27120 = CARTESIAN_POINT ( 'NONE',  ( -3.999999999999997335, 18.68750000000000000, 32.30940107675850470 ) ) ;
#27121 = CARTESIAN_POINT ( 'NONE',  ( 4.284375000614518925, -4.541064518000419881, 2.621784821874995952 ) ) ;
#27122 = APPLICATION_PROTOCOL_DEFINITION ( 'draft international standard', 'automotive_design', 1998, #25218 ) ;
#27123 = CARTESIAN_POINT ( 'NONE',  ( 13.12500000122903288, -5.773502691896255534, -1.060575238724906372E-15 ) ) ;
#27124 = CARTESIAN_POINT ( 'NONE',  ( 9.262500001229033941, 4.330127018922192761, -2.499999999999997780 ) ) ;
#27125 = CARTESIAN_POINT ( 'NONE',  ( 29.02500000122903145, 2.886751345948129099, -4.999999999999998224 ) ) ;
#27126 = CARTESIAN_POINT ( 'NONE',  ( 4.000000000000000000, 16.53124999877096712, 27.69059892324149530 ) ) ;
#27127 = CARTESIAN_POINT ( 'NONE',  ( 19.03125000122902932, 6.123233995736764310E-16, -4.999999999999998224 ) ) ;
#27128 = CARTESIAN_POINT ( 'NONE',  ( 12.23437500061451821, 4.541064518000418104, 2.621784821874999949 ) ) ;
#27129 = CARTESIAN_POINT ( 'NONE',  ( -1.626862140677534273E-15, 17.73124999877096641, 34.00000000000000000 ) ) ;
#27130 = ORIENTED_EDGE ( 'NONE', *, *, #65502, .T. ) ;
#27131 = EDGE_CURVE ( 'NONE', #1724, #45117, #60282, .T. ) ;
#27132 = CARTESIAN_POINT ( 'NONE',  ( 19.49062500061451431, -3.027376345333614438, 5.243569643749998122 ) ) ;
#27133 = CARTESIAN_POINT ( 'NONE',  ( 12.30937500061451573, 0.000000000000000000, 5.243569643749999010 ) ) ;
#27134 = CARTESIAN_POINT ( 'NONE',  ( 5.015625000614518214, 3.027376345333611329, 5.243569643749999010 ) ) ;
#27135 = CARTESIAN_POINT ( 'NONE',  ( 22.35937500061451644, -4.541064518000417216, -2.621784821875001281 ) ) ;
#27136 = CARTESIAN_POINT ( 'NONE',  ( 6.140625000614516438, -3.027376345333610441, -5.243569643749999898 ) ) ;
#27137 = CYLINDRICAL_SURFACE ( 'NONE', #4979, 3.999999999999996447 ) ;
#27138 = CARTESIAN_POINT ( 'NONE',  ( 7.537500001229033408, 4.330127018922191873, 2.499999999999999556 ) ) ;
#27139 = CARTESIAN_POINT ( 'NONE',  ( 22.90312500061451573, 4.541064518000418104, -2.621784821874998173 ) ) ;
#27140 = CARTESIAN_POINT ( 'NONE',  ( -2.000000000000000000, 17.78750000122903430, -33.46410161513775705 ) ) ;
#27141 = CARTESIAN_POINT ( 'NONE',  ( 8.737500001229033586, 6.123233995736764310E-16, -4.999999999999998224 ) ) ;
#27142 = CARTESIAN_POINT ( 'NONE',  ( 18.29062500061451502, -3.027376345333610441, -5.243569643749999898 ) ) ;
#27143 = CARTESIAN_POINT ( 'NONE',  ( 15.59062500061451573, -3.027376345333610441, -5.243569643749999898 ) ) ;
#27144 = CARTESIAN_POINT ( 'NONE',  ( 25.65937500061451715, 4.119189519843966529, -2.378215178124998275 ) ) ;
#27145 = CARTESIAN_POINT ( 'NONE',  ( 14.62500000000000000, 4.330127018922191873, 2.499999999999999556 ) ) ;
#27146 = CARTESIAN_POINT ( 'NONE',  ( 11.51250000122903216, 4.330127018922192761, -2.499999999999997780 ) ) ;
#27147 = CARTESIAN_POINT ( 'NONE',  ( 9.065625000614517148, 3.027376345333611329, 5.243569643749999010 ) ) ;
#27148 = CARTESIAN_POINT ( 'NONE',  ( 11.95312500061451644, -4.541064518000417216, -2.621784821875001281 ) ) ;
#27149 = CARTESIAN_POINT ( 'NONE',  ( 20.13750000122903216, 4.330127018922191873, 2.499999999999999556 ) ) ;
#27150 = CARTESIAN_POINT ( 'NONE',  ( -2.121784821874999949, 13.03437500061451715, -33.67503911421598417 ) ) ;
#27151 = CARTESIAN_POINT ( 'NONE',  ( 20.29687500061451644, 6.054752690667223547, 3.707466751127219781E-16 ) ) ;
#27152 = CARTESIAN_POINT ( 'NONE',  ( 45.00000000000000000, 2.500000000000000444, 3.499999999999999112 ) ) ;
#27153 = CARTESIAN_POINT ( 'NONE',  ( 4.650000001229035895, -2.886751345948125991, -5.000000000000000000 ) ) ;
#27154 = CARTESIAN_POINT ( 'NONE',  ( 3.121875000614518836, 3.027376345333613106, -5.243569643749998122 ) ) ;
#27155 = CARTESIAN_POINT ( 'NONE',  ( 19.92187500061451644, 3.027376345333611329, 5.243569643749999010 ) ) ;
#27156 = EDGE_CURVE ( 'NONE', #64487, #46244, #15410, .T. ) ;
#27157 = CARTESIAN_POINT ( 'NONE',  ( 27.71250000000000213, 2.886751345948098901, 5.000000000000047073 ) ) ;
#27158 = CARTESIAN_POINT ( 'NONE',  ( 18.62812500061451715, -4.541064518000419881, 2.621784821874995952 ) ) ;
#27159 = CARTESIAN_POINT ( 'NONE',  ( 10.85625000122903216, -4.330127018922190985, -2.500000000000001332 ) ) ;
#27160 = LINE ( 'NONE', #66311, #48405 ) ;
#27161 = DIRECTION ( 'NONE',  ( -0.000000000000000000, -1.000000000000000000, -0.000000000000000000 ) ) ;
#27162 = CARTESIAN_POINT ( 'NONE',  ( 28.95937500061451431, 0.000000000000000000, 5.243569643749999010 ) ) ;
#27163 = CARTESIAN_POINT ( 'NONE',  ( 21.68437500061451573, -2.746126346562646425, 4.756430356249996549 ) ) ;
#27164 = CARTESIAN_POINT ( 'NONE',  ( 14.76562500061451821, 3.027376345333613106, -5.243569643749998122 ) ) ;
#27165 = CARTESIAN_POINT ( 'NONE',  ( 14.37187500061451928, 3.027376345333613106, -5.243569643749998122 ) ) ;
#27166 = ORIENTED_EDGE ( 'NONE', *, *, #31908, .T. ) ;
#27167 = CARTESIAN_POINT ( 'NONE',  ( 10.55625000122903323, 4.330127018922192761, -2.499999999999997780 ) ) ;
#27168 = CARTESIAN_POINT ( 'NONE',  ( 22.30312500061451431, -4.541064518000417216, -2.621784821875001281 ) ) ;
#27169 = DIRECTION ( 'NONE',  ( -1.000000000000000000, -0.000000000000000000, -0.000000000000000000 ) ) ;
#27170 = CARTESIAN_POINT ( 'NONE',  ( 0.000000000000000000, 27.50000000000000000, 26.00000000000000000 ) ) ;
#27171 = CARTESIAN_POINT ( 'NONE',  ( 11.73750000000000249, -2.886751345948125991, -5.000000000000000000 ) ) ;
#27172 = CARTESIAN_POINT ( 'NONE',  ( 23.55000000122903359, -2.886751345948125991, -5.000000000000000000 ) ) ;
#27173 = CARTESIAN_POINT ( 'NONE',  ( 18.59062500061451573, -3.027376345333614438, 5.243569643749998122 ) ) ;
#27174 = ORIENTED_EDGE ( 'NONE', *, *, #4477, .T. ) ;
#27175 = CARTESIAN_POINT ( 'NONE',  ( 18.93750000000000000, -2.886751345948125991, -5.000000000000000000 ) ) ;
#27176 = CARTESIAN_POINT ( 'NONE',  ( 21.72187500061451715, 3.027376345333611329, 5.243569643749999010 ) ) ;
#27177 = ORIENTED_EDGE ( 'NONE', *, *, #51676, .T. ) ;
#27178 = CARTESIAN_POINT ( 'NONE',  ( -1.626862140677534273E-15, 19.13749999999999929, 34.00000000000000000 ) ) ;
#27179 = CARTESIAN_POINT ( 'NONE',  ( 11.61562500061451608, 3.027376345333613106, -5.243569643749998122 ) ) ;
#27180 = CARTESIAN_POINT ( 'NONE',  ( 45.00000000000000000, 2.500000000000000000, -3.500000000000000000 ) ) ;
#27181 = CARTESIAN_POINT ( 'NONE',  ( 14.82187500061451502, 4.119189519843966529, 2.378215178124999607 ) ) ;
#27182 = CARTESIAN_POINT ( 'NONE',  ( 16.83749999999999858, 5.773502691896255534, 3.535250795749688894E-16 ) ) ;
#27183 = CARTESIAN_POINT ( 'NONE',  ( 25.27499999999999858, 6.123233995736764310E-16, -4.999999999999998224 ) ) ;
#27184 = FACE_OUTER_BOUND ( 'NONE', #35863, .T. ) ;
#27185 = CARTESIAN_POINT ( 'NONE',  ( 4.621875000614516615, 3.027376345333611329, 5.243569643749999010 ) ) ;
#27186 = CARTESIAN_POINT ( 'NONE',  ( 27.87187500061451573, 3.027376345333613106, -5.243569643749998122 ) ) ;
#27187 = ORIENTED_EDGE ( 'NONE', *, *, #5393, .T. ) ;
#27188 = CARTESIAN_POINT ( 'NONE',  ( 26.84062500061451573, -3.027376345333610441, -5.243569643749999898 ) ) ;
#27189 = CARTESIAN_POINT ( 'NONE',  ( 26.63437500061451857, 4.541064518000418104, 2.621784821874999949 ) ) ;
#27190 = CARTESIAN_POINT ( 'NONE',  ( 3.384375000614517237, -4.541064518000419881, 2.621784821874995952 ) ) ;
#27191 = CARTESIAN_POINT ( 'NONE',  ( 12.86250000000000071, 2.886751345948126879, 4.999999999999999112 ) ) ;
#27192 = CARTESIAN_POINT ( 'NONE',  ( 10.82812500061451644, 4.541064518000418104, 2.621784821874999949 ) ) ;
#27193 = CARTESIAN_POINT ( 'NONE',  ( 0.000000000000000000, 20.00000000000000000, 30.00000000000000000 ) ) ;
#27194 = CARTESIAN_POINT ( 'NONE',  ( 1.071796769724490117, 19.23259618943233917, -26.00000000000000000 ) ) ;
#27195 = CARTESIAN_POINT ( 'NONE',  ( 29.50312500061451360, -4.541064518000417216, -2.621784821875001281 ) ) ;
#27196 = CARTESIAN_POINT ( 'NONE',  ( 16.72500000122903430, -5.773502691896255534, -1.060575238724906372E-15 ) ) ;
#27197 = CARTESIAN_POINT ( 'NONE',  ( 29.07187500061451502, 5.824947211148865298E-16, -4.756430356249998326 ) ) ;
#27198 = CARTESIAN_POINT ( 'NONE',  ( 14.85937500061451644, 4.119189519843966529, -2.378215178124998275 ) ) ;
#27199 = CARTESIAN_POINT ( 'NONE',  ( 5.990625000614517859, -3.027376345333614438, 5.243569643749998122 ) ) ;
#27200 = CARTESIAN_POINT ( 'NONE',  ( 22.13437500061451502, 4.541064518000418104, 2.621784821874999949 ) ) ;
#27201 = CARTESIAN_POINT ( 'NONE',  ( -4.243569643749997233, 14.49687500061451928, 32.45002607614398471 ) ) ;
#27202 = CARTESIAN_POINT ( 'NONE',  ( 21.60937500061451644, 4.541064518000418104, -2.621784821874998173 ) ) ;
#27203 = CARTESIAN_POINT ( 'NONE',  ( 3.149999999999999911, -4.330127018922190985, -2.500000000000001332 ) ) ;
#27204 = CARTESIAN_POINT ( 'NONE',  ( -4.243569643749998122, 19.44687500061451857, 32.45002607614398471 ) ) ;
#27205 = CARTESIAN_POINT ( 'NONE',  ( 8.915625000614515017, 3.027376345333613106, -5.243569643749998122 ) ) ;
#27206 = FACE_OUTER_BOUND ( 'NONE', #60553, .T. ) ;
#27207 = CARTESIAN_POINT ( 'NONE',  ( 6.984375000614516438, -4.541064518000419881, 2.621784821874995952 ) ) ;
#27208 = DIRECTION ( 'NONE',  ( 1.000000000000000000, -0.000000000000000000, -0.000000000000000000 ) ) ;
#27209 = CARTESIAN_POINT ( 'NONE',  ( 6.403125000614517504, 0.000000000000000000, 5.243569643749999010 ) ) ;
#27210 = CARTESIAN_POINT ( 'NONE',  ( 12.12187500061451573, 3.027376345333613106, -5.243569643749998122 ) ) ;
#27211 = CARTESIAN_POINT ( 'NONE',  ( 25.61250000000000071, -5.773502691896255534, -1.060575238724906372E-15 ) ) ;
#27212 = CARTESIAN_POINT ( 'NONE',  ( 22.53750000122903430, -4.330127018922194537, 2.499999999999995559 ) ) ;
#27213 = CARTESIAN_POINT ( 'NONE',  ( 8.634375000614518569, 4.541064518000418104, 2.621784821874999949 ) ) ;
#27214 = CARTESIAN_POINT ( 'NONE',  ( 11.01562500061451821, -6.054752690667223547, -1.112240025338166033E-15 ) ) ;
#27215 = CARTESIAN_POINT ( 'NONE',  ( 26.75625000122903430, 4.330127018922192761, -2.499999999999997780 ) ) ;
#27216 = CARTESIAN_POINT ( 'NONE',  ( 18.83437500061451431, 6.421520780324663323E-16, -5.243569643749999010 ) ) ;
#27217 = CARTESIAN_POINT ( 'NONE',  ( 9.528763966825557376E-15, 17.41249999999999787, -26.00000000000000000 ) ) ;
#27218 = CARTESIAN_POINT ( 'NONE',  ( 21.78750000122903074, 6.123233995736764310E-16, -4.999999999999998224 ) ) ;
#27219 = CARTESIAN_POINT ( 'NONE',  ( 28.17187500061451644, -6.054752690667223547, -1.112240025338166033E-15 ) ) ;
#27220 = CARTESIAN_POINT ( 'NONE',  ( -2.121784821874999949, 12.13437500061451857, -33.67503911421598417 ) ) ;
#27221 = CARTESIAN_POINT ( 'NONE',  ( 14.85000000122903252, -2.886751345948129988, 4.999999999999997335 ) ) ;
#27222 = CARTESIAN_POINT ( 'NONE',  ( 4.243569643749999898, 16.39062500061451999, -27.54997392385601529 ) ) ;
#27223 = CARTESIAN_POINT ( 'NONE',  ( 14.25000000122903465, 5.773502691896255534, 3.535250795749688894E-16 ) ) ;
#27224 = CARTESIAN_POINT ( 'NONE',  ( 9.703125000614514661, -4.541064518000417216, -2.621784821875001281 ) ) ;
#27225 = ORIENTED_EDGE ( 'NONE', *, *, #17040, .F. ) ;
#27226 = CARTESIAN_POINT ( 'NONE',  ( 13.53749999999999964, -2.886751345948125991, -5.000000000000000000 ) ) ;
#27227 = CARTESIAN_POINT ( 'NONE',  ( 23.79375000122903216, -2.886751345948102898, 5.000000000000044409 ) ) ;
#27228 = CARTESIAN_POINT ( 'NONE',  ( 22.00312500061451360, 4.541064518000418104, -2.621784821874998173 ) ) ;
#27229 = CARTESIAN_POINT ( 'NONE',  ( 6.834375000614518747, 4.541064518000418104, 2.621784821874999949 ) ) ;
#27230 = PLANE ( 'NONE',  #59836 ) ;
#27231 = CARTESIAN_POINT ( 'NONE',  ( 11.02500000122903501, 2.886751345948129099, -4.999999999999998224 ) ) ;
#27232 = CARTESIAN_POINT ( 'NONE',  ( 18.00000000122903288, -2.886751345948129988, 4.999999999999997335 ) ) ;
#27233 = CARTESIAN_POINT ( 'NONE',  ( 15.14062500061451644, -3.027376345333610441, -5.243569643749999898 ) ) ;
#27234 = CARTESIAN_POINT ( 'NONE',  ( 18.66562500061451146, -6.054752690667223547, -1.112240025338166033E-15 ) ) ;
#27235 = CARTESIAN_POINT ( 'NONE',  ( 26.02500000122903145, 2.886751345948126879, 4.999999999999999112 ) ) ;
#27236 = EDGE_CURVE ( 'NONE', #50521, #59214, #35271, .T. ) ;
#27237 = CARTESIAN_POINT ( 'NONE',  ( 28.08750000122903145, 6.123233995736764310E-16, -4.999999999999998224 ) ) ;
#27238 = CARTESIAN_POINT ( 'NONE',  ( 23.25000000000000000, 0.000000000000000000, 4.999999999999998224 ) ) ;
#27239 = CARTESIAN_POINT ( 'NONE',  ( 2.655984681222220721E-16, 13.20312499938548534, 25.66244784525396483 ) ) ;
#27240 = CARTESIAN_POINT ( 'NONE',  ( 25.39687500061451431, -3.027376345333614438, 5.243569643749998122 ) ) ;
#27241 = CARTESIAN_POINT ( 'NONE',  ( 18.22500000122903074, 2.886751345948129099, -4.999999999999997335 ) ) ;
#27242 = CARTESIAN_POINT ( 'NONE',  ( 12.60000000122903430, -2.886751345948129988, 4.999999999999997335 ) ) ;
#27243 = ADVANCED_FACE ( 'NONE', ( #22162 ), #32159, .T. ) ;
#27244 = CARTESIAN_POINT ( 'NONE',  ( 27.57187500061451857, 3.027376345333611329, 5.243569643749999010 ) ) ;
#27245 =( BOUNDED_CURVE ( )  B_SPLINE_CURVE ( 2, ( #39054, #22413, #39416, #33138, #61567, #27607, #12055 ),
 .UNSPECIFIED., .F., .F. ) 
 B_SPLINE_CURVE_WITH_KNOTS ( ( 3, 2, 2, 3 ),
 ( 0.1416666666666666352, 0.1444444444444444031, 0.1472222222222221710, 0.1499999999999999389 ),
 .UNSPECIFIED. ) 
 CURVE ( )  GEOMETRIC_REPRESENTATION_ITEM ( )  RATIONAL_B_SPLINE_CURVE ( ( 1.000000000000001332, 0.8660254037844373753, 1.000000000000000000, 0.8660254037844387076, 1.000000000000000000, 0.8660254037844413721, 0.9999999999999973355 ) ) 
 REPRESENTATION_ITEM ( '' )  );
#27246 = EDGE_CURVE ( 'NONE', #66704, #44084, #42832, .T. ) ;
#27247 = CARTESIAN_POINT ( 'NONE',  ( 12.44999999999999929, 0.000000000000000000, 4.999999999999998224 ) ) ;
#27248 = CARTESIAN_POINT ( 'NONE',  ( 5.334375000614517859, 6.421520780324663323E-16, -5.243569643749999010 ) ) ;
#27249 = CARTESIAN_POINT ( 'NONE',  ( 25.49062500061451786, -3.027376345333610441, -5.243569643749999898 ) ) ;
#27250 = CARTESIAN_POINT ( 'NONE',  ( -3.756430356249999214, 15.19062499938548427, 27.83122392262697176 ) ) ;
#27251 = CARTESIAN_POINT ( 'NONE',  ( 1.999999999999998668, 19.84999999999999787, -33.46410161513775705 ) ) ;
#27252 = CARTESIAN_POINT ( 'NONE',  ( 10.77187500061451786, 3.027376345333613106, -5.243569643749998122 ) ) ;
#27253 = CARTESIAN_POINT ( 'NONE',  ( 3.632573829565322487, -3.435821811263616521, 3.669822893043289014 ) ) ;
#27254 = CARTESIAN_POINT ( 'NONE',  ( 3.421875000614516882, -6.054752690667223547, -1.112240025338166033E-15 ) ) ;
#27255 = CARTESIAN_POINT ( 'NONE',  ( 9.384375000614518569, 6.421520780324663323E-16, -5.243569643749999010 ) ) ;
#27256 = CARTESIAN_POINT ( 'NONE',  ( 28.80937500061451573, 4.541064518000418104, -2.621784821874998173 ) ) ;
#27257 = CARTESIAN_POINT ( 'NONE',  ( 4.243569643749999898, 12.82812500061459637, 30.00000000000000000 ) ) ;
#27258 = CARTESIAN_POINT ( 'NONE',  ( 19.53749999999999432, 5.773502691896255534, 3.535250795749688894E-16 ) ) ;
#27259 = ORIENTED_EDGE ( 'NONE', *, *, #28959, .F. ) ;
#27261 = EDGE_CURVE ( 'NONE', #45340, #26440, #30517, .T. ) ;
#27260 = CARTESIAN_POINT ( 'NONE',  ( -1.071796769724488563, 17.84240381056766367, -26.00000000000000000 ) ) ;
#27262 = CARTESIAN_POINT ( 'NONE',  ( 3.562500000000000444, -5.773502691896255534, -1.060575238724906372E-15 ) ) ;
#27263 = VERTEX_POINT ( 'NONE', #16608 ) ;
#27264 = CARTESIAN_POINT ( 'NONE',  ( 17.20312500061451644, 0.000000000000000000, 5.243569643749999010 ) ) ;
#27265 = CARTESIAN_POINT ( 'NONE',  ( 8.615625000614517859, 3.027376345333611329, 5.243569643749999010 ) ) ;
#27266 = CARTESIAN_POINT ( 'NONE',  ( 22.39687500061451431, 4.119189519843966529, -2.378215178124998275 ) ) ;
#27267 = CARTESIAN_POINT ( 'NONE',  ( 7.621875000614519280, 3.027376345333613106, -5.243569643749998122 ) ) ;
#27268 = CARTESIAN_POINT ( 'NONE',  ( 17.55000000122903359, -2.886751345948129988, 4.999999999999997335 ) ) ;
#27269 = CARTESIAN_POINT ( 'NONE',  ( 45.00000000000000000, 6.123233995736764310E-16, -4.999999999999998224 ) ) ;
#27270 = CARTESIAN_POINT ( 'NONE',  ( 7.884375000614517681, -4.541064518000419881, 2.621784821874995952 ) ) ;
#27271 = CARTESIAN_POINT ( 'NONE',  ( 12.79687500061451821, -3.027376345333614438, 5.243569643749998122 ) ) ;
#27272 = CARTESIAN_POINT ( 'NONE',  ( 24.83437500061451431, 4.541064518000418104, 2.621784821874999949 ) ) ;
#27273 = CARTESIAN_POINT ( 'NONE',  ( 26.62500000000000000, 6.123233995736764310E-16, -4.999999999999998224 ) ) ;
#27274 = ORIENTED_EDGE ( 'NONE', *, *, #20762, .T. ) ;
#27275 = CARTESIAN_POINT ( 'NONE',  ( 10.57500000000000107, 4.330127018922191873, 2.499999999999999556 ) ) ;
#27276 = CARTESIAN_POINT ( 'NONE',  ( 18.08437500061451431, 4.541064518000418104, 2.621784821874999949 ) ) ;
#27277 = CARTESIAN_POINT ( 'NONE',  ( 8.896875000614517859, -3.027376345333610441, -5.243569643749999898 ) ) ;
#27278 = CARTESIAN_POINT ( 'NONE',  ( -1.878215178125001827, 13.84062499938548285, 33.25316411605952283 ) ) ;
#27279 = CARTESIAN_POINT ( 'NONE',  ( 21.44999999999999929, 0.000000000000000000, 4.999999999999998224 ) ) ;
#27280 = CARTESIAN_POINT ( 'NONE',  ( 2.000000000000000444, 16.62500000000000000, 26.53589838486224650 ) ) ;
#27281 = CARTESIAN_POINT ( 'NONE',  ( 30.00000000000000000, 0.000000000000000000, 4.999999999999998224 ) ) ;
#27282 = CARTESIAN_POINT ( 'NONE',  ( 21.68437500061451573, 4.119189519843966529, 2.378215178124999607 ) ) ;
#27283 = CARTESIAN_POINT ( 'NONE',  ( 13.22812500061451502, -4.541064518000419881, 2.621784821874995952 ) ) ;
#27284 = CARTESIAN_POINT ( 'NONE',  ( 3.000000000000002665, 0.000000000000000000, 4.999999999999998224 ) ) ;
#27285 = CARTESIAN_POINT ( 'NONE',  ( 28.24687500061451573, -3.027376345333610441, -5.243569643749999898 ) ) ;
#27286 = CARTESIAN_POINT ( 'NONE',  ( 9.225000000000001421, 4.330127018922191873, 2.499999999999999556 ) ) ;
#27287 = CARTESIAN_POINT ( 'NONE',  ( 3.999999999999998668, 16.32500000122903216, 27.69059892324149175 ) ) ;
#27288 = CARTESIAN_POINT ( 'NONE',  ( 8.775000001229033231, 2.886751345948129099, -4.999999999999998224 ) ) ;
#27289 = CARTESIAN_POINT ( 'NONE',  ( 20.03437500061451715, -4.541064518000419881, 2.621784821874995952 ) ) ;
#27290 = CARTESIAN_POINT ( 'NONE',  ( 14.93437500061451750, 4.541064518000418104, 2.621784821874999949 ) ) ;
#27291 = CARTESIAN_POINT ( 'NONE',  ( 0.000000000000000000, 20.00000000000000000, 30.00000000000000000 ) ) ;
#27292 = ORIENTED_EDGE ( 'NONE', *, *, #26513, .T. ) ;
#27293 = CARTESIAN_POINT ( 'NONE',  ( 16.11562500061451786, 3.027376345333613106, -5.243569643749998122 ) ) ;
#27294 = CARTESIAN_POINT ( 'NONE',  ( 27.97500000122903074, -5.773502691896255534, -1.060575238724906372E-15 ) ) ;
#27295 = CARTESIAN_POINT ( 'NONE',  ( 14.33437500061451786, 6.421520780324663323E-16, -5.243569643749999010 ) ) ;
#27296 = CARTESIAN_POINT ( 'NONE',  ( 1.587219675395663998, 9.875134926496690113, -24.21030195342116187 ) ) ;
#27297 = CARTESIAN_POINT ( 'NONE',  ( 17.27812500061451217, -4.541064518000419881, 2.621784821874995952 ) ) ;
#27298 = CARTESIAN_POINT ( 'NONE',  ( 4.000000000000000000, 20.09374999877096712, 30.00000000000000000 ) ) ;
#27299 = CARTESIAN_POINT ( 'NONE',  ( 28.95937500061451431, 0.000000000000000000, 5.243569643749999010 ) ) ;
#27300 = CARTESIAN_POINT ( 'NONE',  ( 2.121784821875001281, 13.65312500061451750, 33.67503911421598417 ) ) ;
#27301 = CARTESIAN_POINT ( 'NONE',  ( 16.20937500061451786, 4.541064518000418104, -2.621784821874998173 ) ) ;
#27302 = CARTESIAN_POINT ( 'NONE',  ( 13.35000000122903430, 5.773502691896255534, 3.535250795749688894E-16 ) ) ;
#27303 = CARTESIAN_POINT ( 'NONE',  ( 10.92187500061451644, 2.746126346562643317, 4.756430356249998326 ) ) ;
#27304 = CARTESIAN_POINT ( 'NONE',  ( 3.329819492037558781, -3.729919858448222048, 3.685474251491927866 ) ) ;
#27305 = CARTESIAN_POINT ( 'NONE',  ( 19.62187500061451573, -6.054752690667223547, -1.112240025338166033E-15 ) ) ;
#27306 = CARTESIAN_POINT ( 'NONE',  ( 22.50000000122903288, -2.886751345948129988, 4.999999999999997335 ) ) ;
#27307 =( BOUNDED_CURVE ( )  B_SPLINE_CURVE ( 2, ( #73060, #9905, #17257, #39083, #61244, #44269, #67885, #54978, #22799 ),
 .UNSPECIFIED., .F., .F. ) 
 B_SPLINE_CURVE_WITH_KNOTS ( ( 3, 2, 2, 2, 3 ),
 ( 0.3369565217391304324, 0.3405797101449275499, 0.3478260869565217295, 0.3550724637681159646, 0.3586956521739130821 ),
 .UNSPECIFIED. ) 
 CURVE ( )  GEOMETRIC_REPRESENTATION_ITEM ( )  RATIONAL_B_SPLINE_CURVE ( ( 0.9330127018922194093, 0.9330127018922194093, 1.000000000000000000, 0.8660254037844387076, 1.000000000000000000, 0.8660254037844387076, 1.000000000000000000, 0.9330127018922188542, 0.9330127018922194093 ) ) 
 REPRESENTATION_ITEM ( '' )  );
#27308 = CARTESIAN_POINT ( 'NONE',  ( 17.74687500061451928, -3.027376345333614438, 5.243569643749998122 ) ) ;
#27309 = CARTESIAN_POINT ( 'NONE',  ( 12.70312500061451821, 0.000000000000000000, 5.243569643749999010 ) ) ;
#27310 = CARTESIAN_POINT ( 'NONE',  ( 4.243569643749999898, 12.84687500061451715, 32.45002607614398471 ) ) ;
#27311 = CARTESIAN_POINT ( 'NONE',  ( 18.06562500061451715, 3.027376345333611329, 5.243569643749999010 ) ) ;
#27312 = ORIENTED_EDGE ( 'NONE', *, *, #25778, .F. ) ;
#27313 = VERTEX_POINT ( 'NONE', #32886 ) ;
#27314 = CARTESIAN_POINT ( 'NONE',  ( 21.33749999999999858, 5.773502691896255534, 3.535250795749688894E-16 ) ) ;
#27315 = CYLINDRICAL_SURFACE ( 'NONE', #60937, 4.999999999999998224 ) ;
#27316 = CARTESIAN_POINT ( 'NONE',  ( 25.15312500061451217, 4.541064518000418104, -2.621784821874998173 ) ) ;
#27317 = CARTESIAN_POINT ( 'NONE',  ( 6.478125000614516793, -4.541064518000419881, 2.621784821874995952 ) ) ;
#27318 = CARTESIAN_POINT ( 'NONE',  ( 18.60000000122903430, -2.886751345948125991, -5.000000000000000000 ) ) ;
#27319 = CARTESIAN_POINT ( 'NONE',  ( 23.09062500061451573, -3.027376345333614438, 5.243569643749998122 ) ) ;
#27320 = CARTESIAN_POINT ( 'NONE',  ( 22.27499999999999858, 4.330127018922191873, 2.499999999999999556 ) ) ;
#27321 = CARTESIAN_POINT ( 'NONE',  ( 25.86562500061451431, -6.054752690667223547, -1.112240025338166033E-15 ) ) ;
#27322 = CARTESIAN_POINT ( 'NONE',  ( 6.365625000614518747, 3.027376345333611329, 5.243569643749999010 ) ) ;
#27323 = ORIENTED_EDGE ( 'NONE', *, *, #39141, .F. ) ;
#27324 = CARTESIAN_POINT ( 'NONE',  ( 29.47499999999999787, 4.330127018922191873, 2.499999999999999556 ) ) ;
#27325 = CARTESIAN_POINT ( 'NONE',  ( -4.000000000000000000, 13.11874999877096570, 30.00000000000000000 ) ) ;
#27326 = CARTESIAN_POINT ( 'NONE',  ( 10.54687500061451644, -2.746126346562646425, 4.756430356249996549 ) ) ;
#27327 = CARTESIAN_POINT ( 'NONE',  ( 1.071796769724476572, 12.93259618943233313, 34.00000000000000000 ) ) ;
#27328 = EDGE_CURVE ( 'NONE', #71040, #10011, #2692, .T. ) ;
#27329 = CARTESIAN_POINT ( 'NONE',  ( 8.484601909799253346E-16, 13.47500000122903430, -25.38119784648299770 ) ) ;
#27330 = ADVANCED_FACE ( 'NONE', ( #21425 ), #27715, .F. ) ;
#27331 = CARTESIAN_POINT ( 'NONE',  ( 4.243569643749999010, 19.22187500061452070, -32.45002607614398471 ) ) ;
#27332 = CARTESIAN_POINT ( 'NONE',  ( 11.73750000000000249, -2.886751345948125991, -5.000000000000000000 ) ) ;
#27333 = CARTESIAN_POINT ( 'NONE',  ( 11.74687500061451573, 6.054752690667223547, 3.707466751127219781E-16 ) ) ;
#27334 = CARTESIAN_POINT ( 'NONE',  ( 7.125000001229033764, 2.886751345948126879, 4.999999999999999112 ) ) ;
#27335 = CARTESIAN_POINT ( 'NONE',  ( 13.05937500061451750, 4.541064518000418104, -2.621784821874998173 ) ) ;
#27336 = CARTESIAN_POINT ( 'NONE',  ( 6.496875000614517504, -3.027376345333614438, 5.243569643749998122 ) ) ;
#27337 = CARTESIAN_POINT ( 'NONE',  ( 4.243569643749999010, 10.16562500061451857, -32.45002607614398471 ) ) ;
#27338 = CYLINDRICAL_SURFACE ( 'NONE', #70155, 4.999999999999998224 ) ;
#27339 = CARTESIAN_POINT ( 'NONE',  ( 9.384375000614518569, 6.421520780324663323E-16, -5.243569643749999010 ) ) ;
#27340 = CARTESIAN_POINT ( 'NONE',  ( 13.19999999999999929, 4.330127018922192761, -2.499999999999997780 ) ) ;
#27341 = CARTESIAN_POINT ( 'NONE',  ( 18.47812500061451857, 4.541064518000418104, 2.621784821874999949 ) ) ;
#27342 = CARTESIAN_POINT ( 'NONE',  ( -1.071796769724491005, 12.37009619066136956, -34.00000000000000000 ) ) ;
#27343 = CARTESIAN_POINT ( 'NONE',  ( 4.243569643749999898, 19.09062500061459389, 32.45002607614398471 ) ) ;
#27344 = CARTESIAN_POINT ( 'NONE',  ( 23.40937500061451715, 4.541064518000418104, -2.621784821874998173 ) ) ;
#27345 = CARTESIAN_POINT ( 'NONE',  ( 3.999999999999999112, 19.32500000000000284, 30.00000000000000000 ) ) ;
#27346 = CARTESIAN_POINT ( 'NONE',  ( 28.20000000122903216, 5.773502691896255534, 3.535250795749688894E-16 ) ) ;
#27347 = CARTESIAN_POINT ( 'NONE',  ( 19.05937500061451217, -5.492252693125287522, -1.008910452111647106E-15 ) ) ;
#27348 = CARTESIAN_POINT ( 'NONE',  ( 25.37812500061451715, -4.541064518000419881, 2.621784821874995952 ) ) ;
#27349 = CARTESIAN_POINT ( 'NONE',  ( 18.70312500061451644, -4.541064518000417216, -2.621784821875001281 ) ) ;
#27350 = CARTESIAN_POINT ( 'NONE',  ( 13.14375000122903536, -2.886751345948125991, -5.000000000000000000 ) ) ;
#27351 = CARTESIAN_POINT ( 'NONE',  ( 13.92187500061451644, 3.027376345333613106, -5.243569643749998122 ) ) ;
#27352 = CARTESIAN_POINT ( 'NONE',  ( 7.350000001229033408, -2.886751345948193048, -4.999999999999883649 ) ) ;
#27353 = CARTESIAN_POINT ( 'NONE',  ( 25.68750000122903288, -4.330127018922194537, 2.499999999999995559 ) ) ;
#27354 = CARTESIAN_POINT ( 'NONE',  ( 3.909375000614518481, -4.541064518000417216, -2.621784821875001281 ) ) ;
#27355 = CARTESIAN_POINT ( 'NONE',  ( 14.48437500061451821, 4.541064518000418104, 2.621784821874999949 ) ) ;
#27356 = CARTESIAN_POINT ( 'NONE',  ( 1.999999999999997335, 17.76874999877096428, 33.46410161513775705 ) ) ;
#27357 = CARTESIAN_POINT ( 'NONE',  ( 3.065815551951259543, -3.949781639713015657, 3.065815551951216467 ) ) ;
#27358 = CARTESIAN_POINT ( 'NONE',  ( 3.112500001229034918, 0.000000000000000000, 4.999999999999998224 ) ) ;
#27359 = CARTESIAN_POINT ( 'NONE',  ( 23.63437500061451502, -4.541064518000419881, 2.621784821874995952 ) ) ;
#27360 = CARTESIAN_POINT ( 'NONE',  ( 16.54687500061451644, -3.027376345333610441, -5.243569643749999898 ) ) ;
#27361 = CARTESIAN_POINT ( 'NONE',  ( 1.878215178125000495, 16.42812499938548143, 26.74683588394047007 ) ) ;
#27362 = CARTESIAN_POINT ( 'NONE',  ( 27.48749999999999716, -2.886751345948125991, -5.000000000000000000 ) ) ;
#27363 = CARTESIAN_POINT ( 'NONE',  ( 4.612500001229032698, -4.330127018922190985, -2.500000000000001332 ) ) ;
#27364 = CARTESIAN_POINT ( 'NONE',  ( 5.437500000000001776, -2.886751345948125991, -5.000000000000000000 ) ) ;
#27365 = CARTESIAN_POINT ( 'NONE',  ( 7.996875000614515727, 4.119189519843966529, -2.378215178124998275 ) ) ;
#27366 = CARTESIAN_POINT ( 'NONE',  ( 19.19062500061452070, -3.027376345333610441, -5.243569643749999898 ) ) ;
#27367 = CARTESIAN_POINT ( 'NONE',  ( 10.35000000000000142, -4.330127018922190985, -2.500000000000001332 ) ) ;
#27368 = CARTESIAN_POINT ( 'NONE',  ( 5.353125000614515905, 4.541064518000418104, -2.621784821874998173 ) ) ;
#27369 = CARTESIAN_POINT ( 'NONE',  ( 17.66249999999999787, 2.886751345948129099, -4.999999999999998224 ) ) ;
#27370 = CARTESIAN_POINT ( 'NONE',  ( 4.000000000000000000, 16.53124999877096712, 27.69059892324149885 ) ) ;
#27371 = CARTESIAN_POINT ( 'NONE',  ( 20.58750000122903145, 4.330127018922191873, 2.499999999999999556 ) ) ;
#27372 = CARTESIAN_POINT ( 'NONE',  ( 5.378878668797007379, 8.432125716319056608, 27.31293200927705911 ) ) ;
#27373 = CARTESIAN_POINT ( 'NONE',  ( 29.22187500061451715, 3.027376345333613106, -5.243569643749998122 ) ) ;
#27374 = ORIENTED_EDGE ( 'NONE', *, *, #21176, .F. ) ;
#27375 = CARTESIAN_POINT ( 'NONE',  ( 17.35312500061451502, -4.541064518000417216, -2.621784821875001281 ) ) ;
#27376 = CARTESIAN_POINT ( 'NONE',  ( 25.26562500061451289, 3.027376345333611329, 5.243569643749999010 ) ) ;
#27377 = CARTESIAN_POINT ( 'NONE',  ( 23.14687500061451786, -3.027376345333614438, 5.243569643749998122 ) ) ;
#27378 = CARTESIAN_POINT ( 'NONE',  ( 6.225000000000001421, -4.330127018922194537, 2.499999999999995559 ) ) ;
#27379 = CARTESIAN_POINT ( 'NONE',  ( 8.428125000614517859, 6.421520780324663323E-16, -5.243569643749999010 ) ) ;
#27380 = CARTESIAN_POINT ( 'NONE',  ( 25.15312500061451217, 4.541064518000418104, -2.621784821874998173 ) ) ;
#27381 = CARTESIAN_POINT ( 'NONE',  ( 15.72187500061451892, 3.027376345333613106, -5.243569643749998122 ) ) ;
#27382 = CARTESIAN_POINT ( 'NONE',  ( 18.83437500061451431, 6.421520780324663323E-16, -5.243569643749999010 ) ) ;
#27383 = CARTESIAN_POINT ( 'NONE',  ( 4.421718391856483521, 2.334208790866869609, -4.695382105235059278 ) ) ;
#27384 = CARTESIAN_POINT ( 'NONE',  ( -2.121784821874996840, 10.48437500061451821, 33.67503911421598417 ) ) ;
#27385 = CARTESIAN_POINT ( 'NONE',  ( 20.88750000122903572, 6.123233995736764310E-16, -4.999999999999998224 ) ) ;
#27386 = CARTESIAN_POINT ( 'NONE',  ( 16.84687500061452070, -2.746126346562646425, 4.756430356249996549 ) ) ;
#27387 = CARTESIAN_POINT ( 'NONE',  ( 10.82812500061451644, 4.541064518000418104, 2.621784821874999949 ) ) ;
#27388 = CARTESIAN_POINT ( 'NONE',  ( 7.809375000614519280, 0.000000000000000000, 5.243569643749999010 ) ) ;
#27389 = CARTESIAN_POINT ( 'NONE',  ( 7.096875000614517148, -3.027376345333610441, -5.243569643749999898 ) ) ;
#27390 = ORIENTED_EDGE ( 'NONE', *, *, #27534, .F. ) ;
#27391 = CARTESIAN_POINT ( 'NONE',  ( 28.43437500061451573, 4.541064518000418104, 2.621784821874999949 ) ) ;
#27392 = CARTESIAN_POINT ( 'NONE',  ( 18.89062500061451644, 6.054752690667223547, 3.707466751127219781E-16 ) ) ;
#27393 = CARTESIAN_POINT ( 'NONE',  ( 29.13750000122903216, 4.330127018922191873, 2.499999999999999556 ) ) ;
#27394 = ADVANCED_FACE ( 'NONE', ( #4463 ), #48013, .T. ) ;
#27395 = CARTESIAN_POINT ( 'NONE',  ( 28.49062500061451431, -3.027376345333614438, 5.243569643749998122 ) ) ;
#27396 = AXIS2_PLACEMENT_3D ( 'NONE', #12393, #23835, #28666 ) ;
#27397 = CARTESIAN_POINT ( 'NONE',  ( 24.90937500061451715, 0.000000000000000000, 5.243569643749999010 ) ) ;
#27398 = CARTESIAN_POINT ( 'NONE',  ( 19.15312500061451573, -4.541064518000417216, -2.621784821875001281 ) ) ;
#27399 = CARTESIAN_POINT ( 'NONE',  ( 4.243569643749999010, 19.67187500061451644, 27.54997392385601174 ) ) ;
#27400 = CARTESIAN_POINT ( 'NONE',  ( 25.67812500061451431, 4.541064518000418104, 2.621784821874999949 ) ) ;
#27401 = CARTESIAN_POINT ( 'NONE',  ( 4.875000001229034652, 2.886751345948126879, 4.999999999999999112 ) ) ;
#27402 = EDGE_LOOP ( 'NONE', ( #18862, #36998, #25972, #45756 ) ) ;
#27403 = CARTESIAN_POINT ( 'NONE',  ( 26.62500000000000000, 6.123233995736764310E-16, -4.999999999999998224 ) ) ;
#27404 = CARTESIAN_POINT ( 'NONE',  ( 4.000000000000000000, 16.58750000000000213, -27.69059892324149530 ) ) ;
#27405 = CARTESIAN_POINT ( 'NONE',  ( -3.756430356250000102, 18.37812499938548427, 30.00000000000000000 ) ) ;
#27406 = CARTESIAN_POINT ( 'NONE',  ( 4.059375000614519280, 4.541064518000418104, -2.621784821874998173 ) ) ;
#27407 = CARTESIAN_POINT ( 'NONE',  ( 11.69062500061451360, 6.054752690667223547, 3.707466751127219781E-16 ) ) ;
#27408 = CARTESIAN_POINT ( 'NONE',  ( 6.084375000614518747, -4.541064518000419881, 2.621784821874995952 ) ) ;
#27409 = CARTESIAN_POINT ( 'NONE',  ( 24.93750000122903288, 6.123233995736764310E-16, -4.999999999999998224 ) ) ;
#27410 = CARTESIAN_POINT ( 'NONE',  ( 15.30937500061451750, 4.541064518000418104, -2.621784821874998173 ) ) ;
#27411 = CARTESIAN_POINT ( 'NONE',  ( 29.46562500061451573, -6.054752690667223547, -1.112240025338166033E-15 ) ) ;
#27412 = CARTESIAN_POINT ( 'NONE',  ( 29.13749999999999929, -2.886751345948129988, 4.999999999999997335 ) ) ;
#27413 = CARTESIAN_POINT ( 'NONE',  ( 27.57187500061451857, 3.027376345333611329, 5.243569643749999010 ) ) ;
#27414 = CARTESIAN_POINT ( 'NONE',  ( 3.328125000614516438, -4.541064518000419881, 2.621784821874995952 ) ) ;
#27415 = CARTESIAN_POINT ( 'NONE',  ( 13.64062500061451644, -3.027376345333614438, 5.243569643749998122 ) ) ;
#27416 = VERTEX_POINT ( 'NONE', #12532 ) ;
#27417 = CARTESIAN_POINT ( 'NONE',  ( 11.09062500061451573, -3.027376345333610441, -5.243569643749999898 ) ) ;
#27418 = CARTESIAN_POINT ( 'NONE',  ( 8.765625000614518214, -6.054752690667223547, -1.112240025338166033E-15 ) ) ;
#27419 = CARTESIAN_POINT ( 'NONE',  ( 17.70937500061451431, 0.000000000000000000, 4.756430356249998326 ) ) ;
#27420 = CARTESIAN_POINT ( 'NONE',  ( 8.137500000000002842, -2.886751345948125991, -5.000000000000000000 ) ) ;
#27421 = EDGE_CURVE ( 'NONE', #52965, #24228, #38073, .T. ) ;
#27422 = CYLINDRICAL_SURFACE ( 'NONE', #14924, 4.000000000000000000 ) ;
#27423 = CARTESIAN_POINT ( 'NONE',  ( 16.91250000000000142, 2.886751345948126879, 4.999999999999999112 ) ) ;
#27424 = CARTESIAN_POINT ( 'NONE',  ( 17.85937500061451999, -4.541064518000417216, -2.621784821875001281 ) ) ;
#27425 = CARTESIAN_POINT ( 'NONE',  ( 14.32500000122903394, 2.886751345948126879, 4.999999999999999112 ) ) ;
#27426 = CARTESIAN_POINT ( 'NONE',  ( 19.91250000000000142, 2.886751345948129099, -4.999999999999998224 ) ) ;
#27427 = CARTESIAN_POINT ( 'NONE',  ( -4.243569643749997233, 15.79062500061451857, -27.54997392385601174 ) ) ;
#27428 = CARTESIAN_POINT ( 'NONE',  ( 26.44687500061451502, 4.119189519843966529, -2.378215178124998275 ) ) ;
#27429 = FACE_OUTER_BOUND ( 'NONE', #36560, .T. ) ;
#27430 = CARTESIAN_POINT ( 'NONE',  ( 25.94062500061451715, -3.027376345333610441, -5.243569643749999898 ) ) ;
#27431 = EDGE_CURVE ( 'NONE', #675, #26527, #50404, .T. ) ;
#27432 = CARTESIAN_POINT ( 'NONE',  ( 20.21250000122903145, 0.000000000000000000, 4.999999999999998224 ) ) ;
#27433 = FACE_OUTER_BOUND ( 'NONE', #48934, .T. ) ;
#27434 = CARTESIAN_POINT ( 'NONE',  ( 12.72187500061451537, 3.027376345333611329, 5.243569643749999010 ) ) ;
#27435 = CARTESIAN_POINT ( 'NONE',  ( 27.78749999999999787, -2.886751345948129988, 4.999999999999997335 ) ) ;
#27436 = CARTESIAN_POINT ( 'NONE',  ( 10.37812500061451715, 4.541064518000418104, 2.621784821874999949 ) ) ;
#27437 = AXIS2_PLACEMENT_3D ( 'NONE', #43454, #48625, #59690 ) ;
#27438 = CARTESIAN_POINT ( 'NONE',  ( 27.75937500061451502, 2.746126346562645981, -4.756430356249997438 ) ) ;
#27439 = CARTESIAN_POINT ( 'NONE',  ( 21.45937500061451786, -4.541064518000417216, -2.621784821875001281 ) ) ;
#27440 = CARTESIAN_POINT ( 'NONE',  ( 14.48437500061451644, -2.746126346562646425, 4.756430356249996549 ) ) ;
#27441 = CARTESIAN_POINT ( 'NONE',  ( 7.003125000614518036, -4.541064518000417216, -2.621784821875001281 ) ) ;
#27442 = CARTESIAN_POINT ( 'NONE',  ( 10.95937500061451964, 0.000000000000000000, 5.243569643749999010 ) ) ;
#27443 = ORIENTED_EDGE ( 'NONE', *, *, #62569, .F. ) ;
#27444 = CARTESIAN_POINT ( 'NONE',  ( 21.72187500061451715, 3.027376345333611329, 5.243569643749999010 ) ) ;
#27445 = CARTESIAN_POINT ( 'NONE',  ( 3.182906284435136790, 3.860443623060027640, -32.43517853776187110 ) ) ;
#27446 = CARTESIAN_POINT ( 'NONE',  ( 26.17500000000000071, 6.123233995736764310E-16, -4.999999999999998224 ) ) ;
#27447 = CARTESIAN_POINT ( 'NONE',  ( 4.162499999999999645, 2.886751345948129099, -4.999999999999998224 ) ) ;
#27448 = CARTESIAN_POINT ( 'NONE',  ( 14.77500000122903501, 2.886751345948126879, 4.999999999999999112 ) ) ;
#27449 = CYLINDRICAL_SURFACE ( 'NONE', #18356, 4.000000000000000000 ) ;
#27450 = CARTESIAN_POINT ( 'NONE',  ( 3.791863662739624274, -3.259105699911376774, 4.107706494585713131 ) ) ;
#27451 = ORIENTED_EDGE ( 'NONE', *, *, #2787, .T. ) ;
#27452 = CARTESIAN_POINT ( 'NONE',  ( 13.35000000000000142, 0.000000000000000000, 4.999999999999998224 ) ) ;
#27453 = CARTESIAN_POINT ( 'NONE',  ( 15.45000000000000107, 4.330127018922192761, -2.499999999999997780 ) ) ;
#27454 = CARTESIAN_POINT ( 'NONE',  ( 12.26250000122903394, -4.330127018922190985, -2.500000000000001332 ) ) ;
#27455 = CARTESIAN_POINT ( 'NONE',  ( 10.34062500061451750, 6.054752690667223547, 3.707466751127219781E-16 ) ) ;
#27456 = ORIENTED_EDGE ( 'NONE', *, *, #14038, .T. ) ;
#27457 = CARTESIAN_POINT ( 'NONE',  ( 9.750000000000001776, 0.000000000000000000, 4.999999999999998224 ) ) ;
#27458 = CARTESIAN_POINT ( 'NONE',  ( 0.000000000000000000, 20.00000000000000000, -30.00000000000000000 ) ) ;
#27459 = CARTESIAN_POINT ( 'NONE',  ( 4.243569643749999898, 15.58437500061451786, -30.00000000000000000 ) ) ;
#27460 = CARTESIAN_POINT ( 'NONE',  ( 3.215625000614518836, 3.027376345333611329, 5.243569643749999010 ) ) ;
#27461 = CARTESIAN_POINT ( 'NONE',  ( 1.878215178125000495, 15.86562499938548321, 26.74683588394047007 ) ) ;
#27462 = CARTESIAN_POINT ( 'NONE',  ( 10.98750000000000071, 5.773502691896255534, 3.535250795749688894E-16 ) ) ;
#27463 = CARTESIAN_POINT ( 'NONE',  ( 3.801890562635342086, 3.247887812877087832, -3.801890562635342086 ) ) ;
#27464 = EDGE_LOOP ( 'NONE', ( #7668, #48244, #37998, #50910 ) ) ;
#27465 = CARTESIAN_POINT ( 'NONE',  ( 23.84062500061451928, 6.054752690667223547, 3.707466751127219781E-16 ) ) ;
#27466 = CARTESIAN_POINT ( 'NONE',  ( 4.247151432104769420, -2.638504256727666863, 4.531370421416291983 ) ) ;
#27467 = CARTESIAN_POINT ( 'NONE',  ( 29.29687500061451644, 6.054752690667223547, 3.707466751127219781E-16 ) ) ;
#27468 = CARTESIAN_POINT ( 'NONE',  ( 21.49687500061451573, -3.027376345333610441, -5.243569643749999898 ) ) ;
#27469 = CARTESIAN_POINT ( 'NONE',  ( 16.37812500061451715, -4.541064518000419881, 2.621784821874995952 ) ) ;
#27470 = CARTESIAN_POINT ( 'NONE',  ( 2.121784821875001281, 12.30312500061459247, -26.32496088578401938 ) ) ;
#27471 = CARTESIAN_POINT ( 'NONE',  ( 5.578125000614518214, -4.541064518000419881, 2.621784821874995952 ) ) ;
#27472 = CARTESIAN_POINT ( 'NONE',  ( 28.05000000122903359, -2.886751345948125991, -5.000000000000000000 ) ) ;
#27473 = CARTESIAN_POINT ( 'NONE',  ( 24.30937500061451573, 4.119189519843966529, -2.378215178124998275 ) ) ;
#27474 = CARTESIAN_POINT ( 'NONE',  ( 19.94062500061451715, -3.027376345333614438, 5.243569643749998122 ) ) ;
#27475 = CARTESIAN_POINT ( 'NONE',  ( 8.934375000614517504, 5.824947211148865298E-16, -4.756430356249998326 ) ) ;
#27476 = CARTESIAN_POINT ( 'NONE',  ( 1.878215178125000495, 18.56562499938548427, 26.74683588394047007 ) ) ;
#27477 = CARTESIAN_POINT ( 'NONE',  ( 14.07187500061451679, 3.027376345333611329, 5.243569643749999010 ) ) ;
#27478 = CARTESIAN_POINT ( 'NONE',  ( 13.77187500061451786, -6.054752690667223547, -1.112240025338166033E-15 ) ) ;
#27479 = CARTESIAN_POINT ( 'NONE',  ( 21.75937500061451502, 0.000000000000000000, 5.243569643749999010 ) ) ;
#27480 = ORIENTED_EDGE ( 'NONE', *, *, #67858, .F. ) ;
#27481 = CARTESIAN_POINT ( 'NONE',  ( -4.243569643749999898, 12.20937500061451608, 30.00000000000000000 ) ) ;
#27482 = CARTESIAN_POINT ( 'NONE',  ( 2.953125000614516438, -4.541064518000417216, -2.621784821875001281 ) ) ;
#27483 = CARTESIAN_POINT ( 'NONE',  ( 26.95312500061451644, 4.541064518000418104, -2.621784821874998173 ) ) ;
#27484 = CARTESIAN_POINT ( 'NONE',  ( 27.51562500061451644, 3.027376345333611329, 5.243569643749999010 ) ) ;
#27485 = CARTESIAN_POINT ( 'NONE',  ( -3.999999999999999112, 20.00000000000000000, 30.00000000000000000 ) ) ;
#27486 = CARTESIAN_POINT ( 'NONE',  ( 4.734375000614518214, -4.541064518000419881, 2.621784821874995952 ) ) ;
#27487 = CARTESIAN_POINT ( 'NONE',  ( 12.48750000122903359, 4.330127018922191873, 2.499999999999999556 ) ) ;
#27488 = CARTESIAN_POINT ( 'NONE',  ( 9.375000001229036428, 2.886751345948126879, 4.999999999999999112 ) ) ;
#27489 = CARTESIAN_POINT ( 'NONE',  ( 28.68750000122903288, 4.330127018922191873, 2.499999999999999556 ) ) ;
#27490 = CARTESIAN_POINT ( 'NONE',  ( -4.000000000000000888, 19.00624999877096499, 32.30940107675850470 ) ) ;
#27491 = CARTESIAN_POINT ( 'NONE',  ( 18.88125000122903430, -4.330127018922194537, 2.499999999999995559 ) ) ;
#27492 = CARTESIAN_POINT ( 'NONE',  ( 12.64687500061451608, 6.054752690667223547, 3.707466751127219781E-16 ) ) ;
#27493 = DIRECTION ( 'NONE',  ( 0.4999999999999975575, 0.000000000000000000, -0.8660254037844400399 ) ) ;
#27494 = ORIENTED_EDGE ( 'NONE', *, *, #58732, .F. ) ;
#27495 = CARTESIAN_POINT ( 'NONE',  ( 20.24062500061451431, 6.054752690667223547, 3.707466751127219781E-16 ) ) ;
#27496 = CARTESIAN_POINT ( 'NONE',  ( 14.18437500061451750, -4.541064518000419881, 2.621784821874995952 ) ) ;
#27497 = CARTESIAN_POINT ( 'NONE',  ( 5.653125000614517504, -4.541064518000417216, -2.621784821875001281 ) ) ;
#27498 = CARTESIAN_POINT ( 'NONE',  ( 21.64687500061451786, 6.054752690667223547, 3.707466751127219781E-16 ) ) ;
#27499 = CARTESIAN_POINT ( 'NONE',  ( 5.653125000614517504, -4.541064518000417216, -2.621784821875001281 ) ) ;
#27500 = CARTESIAN_POINT ( 'NONE',  ( 6.600000001229032520, 5.773502691896255534, 3.535250795749688401E-16 ) ) ;
#27502 = EDGE_CURVE ( 'NONE', #18316, #70559, #23248, .T. ) ;
#27501 = CARTESIAN_POINT ( 'NONE',  ( 5.662500001229035185, 4.330127018922192761, -2.499999999999997780 ) ) ;
#27503 = CARTESIAN_POINT ( 'NONE',  ( 19.94062500061451715, -3.027376345333614438, 5.243569643749998122 ) ) ;
#27504 = CARTESIAN_POINT ( 'NONE',  ( 8.925000001229033586, 2.886751345948126879, 4.999999999999999112 ) ) ;
#27505 = CARTESIAN_POINT ( 'NONE',  ( 16.22812500061451857, 4.541064518000418104, 2.621784821874999949 ) ) ;
#27506 = CARTESIAN_POINT ( 'NONE',  ( 15.92812500061451608, -4.541064518000419881, 2.621784821874995952 ) ) ;
#27507 = CARTESIAN_POINT ( 'NONE',  ( 26.07187500061451857, 2.746126346562645981, -4.756430356249997438 ) ) ;
#27508 = CARTESIAN_POINT ( 'NONE',  ( 16.12500000000000000, -4.330127018922194537, 2.499999999999995559 ) ) ;
#27509 = CARTESIAN_POINT ( 'NONE',  ( 10.65000000122903323, 5.773502691896255534, 3.535250795749688894E-16 ) ) ;
#27510 = CARTESIAN_POINT ( 'NONE',  ( 6.890625000614516438, -3.027376345333614438, 5.243569643749998122 ) ) ;
#27511 = CARTESIAN_POINT ( 'NONE',  ( 10.26562500061451644, 3.027376345333613106, -5.243569643749998122 ) ) ;
#27512 = CARTESIAN_POINT ( 'NONE',  ( 20.92500000122903714, 2.886751345948129099, -4.999999999999998224 ) ) ;
#27513 = CARTESIAN_POINT ( 'NONE',  ( -4.243569643749999898, 13.52187500061451786, -32.45002607614398471 ) ) ;
#27514 = CARTESIAN_POINT ( 'NONE',  ( 4.547618213146977340, -2.078260952684914731, 4.652852879716590451 ) ) ;
#27515 = CARTESIAN_POINT ( 'NONE',  ( 4.912500001229034297, 0.000000000000000000, 4.999999999999998224 ) ) ;
#27516 = CARTESIAN_POINT ( 'NONE',  ( 4.246875000614519280, -3.027376345333614438, 5.243569643749998122 ) ) ;
#27517 = CARTESIAN_POINT ( 'NONE',  ( 21.57187500061451502, 3.027376345333613106, -5.243569643749998122 ) ) ;
#27518 =( BOUNDED_CURVE ( )  B_SPLINE_CURVE ( 2, ( #52870, #40338, #7082, #6722, #40706, #29611, #24060 ),
 .UNSPECIFIED., .F., .F. ) 
 B_SPLINE_CURVE_WITH_KNOTS ( ( 3, 2, 2, 3 ),
 ( 0.6199999999999999956, 0.6233333333333332948, 0.6266666666666668162, 0.6300000000000001155 ),
 .UNSPECIFIED. ) 
 CURVE ( )  GEOMETRIC_REPRESENTATION_ITEM ( )  RATIONAL_B_SPLINE_CURVE ( ( 1.000000000000000000, 0.8660254037844387076, 1.000000000000000000, 0.8660254037844387076, 1.000000000000000000, 0.8660254037844342667, 1.000000000000004441 ) ) 
 REPRESENTATION_ITEM ( '' )  );
#27519 = CARTESIAN_POINT ( 'NONE',  ( 16.07812500061451289, 6.421520780324663323E-16, -5.243569643749999010 ) ) ;
#27520 = CARTESIAN_POINT ( 'NONE',  ( 12.50625000122903430, 0.000000000000000000, 4.999999999999998224 ) ) ;
#27521 = CARTESIAN_POINT ( 'NONE',  ( 1.626862140677534273E-15, 13.81250000000000000, -26.00000000000000355 ) ) ;
#27522 = FACE_OUTER_BOUND ( 'NONE', #50737, .T. ) ;
#27523 = CARTESIAN_POINT ( 'NONE',  ( 28.73437500061451644, 6.421520780324663323E-16, -5.243569643749999010 ) ) ;
#27524 = CARTESIAN_POINT ( 'NONE',  ( 21.00937500061451857, 2.746126346562645981, -4.756430356249997438 ) ) ;
#27525 = CARTESIAN_POINT ( 'NONE',  ( 14.61562500061451608, -6.054752690667223547, -1.112240025338166033E-15 ) ) ;
#27526 = CARTESIAN_POINT ( 'NONE',  ( 12.87187500061451750, -6.054752690667223547, -1.112240025338166033E-15 ) ) ;
#27527 = ORIENTED_EDGE ( 'NONE', *, *, #58189, .T. ) ;
#27528 = CARTESIAN_POINT ( 'NONE',  ( 29.12812500061451715, 6.421520780324663323E-16, -5.243569643749999010 ) ) ;
#27529 = CARTESIAN_POINT ( 'NONE',  ( 23.46562500061451573, 3.027376345333611329, 5.243569643749999010 ) ) ;
#27530 = CARTESIAN_POINT ( 'NONE',  ( 17.58750000122903145, -4.330127018922194537, 2.499999999999995559 ) ) ;
#27531 = CARTESIAN_POINT ( 'NONE',  ( 28.57500000122903572, 2.886751345948099789, -5.000000000000048850 ) ) ;
#27532 = EDGE_CURVE ( 'NONE', #12792, #13938, #68697, .T. ) ;
#27533 = CARTESIAN_POINT ( 'NONE',  ( 12.18750000000000000, -2.886751345948125991, -5.000000000000000000 ) ) ;
#27534 = EDGE_CURVE ( 'NONE', #27030, #18997, #7426, .T. ) ;
#27535 = CARTESIAN_POINT ( 'NONE',  ( 22.50000000122903288, -2.886751345948129988, 4.999999999999997335 ) ) ;
#27536 = CARTESIAN_POINT ( 'NONE',  ( 15.89062500061451289, -3.027376345333614438, 5.243569643749998122 ) ) ;
#27537 = CARTESIAN_POINT ( 'NONE',  ( 13.32187500061451502, 5.824947211148865298E-16, -4.756430356249998326 ) ) ;
#27538 = VERTEX_POINT ( 'NONE', #31714 ) ;
#27539 = CARTESIAN_POINT ( 'NONE',  ( 20.58750000000000213, -2.886751345948129988, 4.999999999999997335 ) ) ;
#27540 = CARTESIAN_POINT ( 'NONE',  ( 22.20937500061451431, 0.000000000000000000, 5.243569643749999010 ) ) ;
#27541 = CARTESIAN_POINT ( 'NONE',  ( 26.99062500061451431, 6.054752690667223547, 3.707466751127219781E-16 ) ) ;
#27542 = VERTEX_POINT ( 'NONE', #9544 ) ;
#27543 = CARTESIAN_POINT ( 'NONE',  ( 19.94999999999999929, 4.330127018922192761, -2.499999999999997780 ) ) ;
#27544 = CARTESIAN_POINT ( 'NONE',  ( 9.628125000614517148, -4.541064518000419881, 2.621784821874995952 ) ) ;
#27545 = CARTESIAN_POINT ( 'NONE',  ( 0.000000000000000000, 0.000000000000000000, 50.00000000000000000 ) ) ;
#27546 = CARTESIAN_POINT ( 'NONE',  ( 14.67187500061451644, 5.824947211148865298E-16, -4.756430356249998326 ) ) ;
#27547 = CARTESIAN_POINT ( 'NONE',  ( 17.32499999999999929, 4.330127018922191873, 2.499999999999999556 ) ) ;
#27548 = CARTESIAN_POINT ( 'NONE',  ( 23.43750000000000000, -2.886751345948125991, -5.000000000000000000 ) ) ;
#27549 = CARTESIAN_POINT ( 'NONE',  ( 2.121784821874999061, 19.65312500061451573, 26.32496088578401583 ) ) ;
#27550 = CARTESIAN_POINT ( 'NONE',  ( 3.646875000614520079, 6.054752690667223547, 3.707466751127219781E-16 ) ) ;
#27551 = CARTESIAN_POINT ( 'NONE',  ( 28.43437500061451573, 4.541064518000418104, 2.621784821874999949 ) ) ;
#27552 = ORIENTED_EDGE ( 'NONE', *, *, #14692, .T. ) ;
#27553 = CARTESIAN_POINT ( 'NONE',  ( 23.91562500061451502, 3.027376345333611329, 5.243569643749999010 ) ) ;
#27554 = CARTESIAN_POINT ( 'NONE',  ( 25.95937500061451431, -4.541064518000417216, -2.621784821875001281 ) ) ;
#27555 = CARTESIAN_POINT ( 'NONE',  ( 4.243569643749999898, 18.67812500061459247, -30.00000000000000000 ) ) ;
#27556 = VECTOR ( 'NONE', #22721, 1000.000000000000000 ) ;
#27557 = CARTESIAN_POINT ( 'NONE',  ( 13.68750000000000178, 5.773502691896255534, 3.535250795749688894E-16 ) ) ;
#27558 = CARTESIAN_POINT ( 'NONE',  ( 12.21562500061451573, 3.027376345333611329, 5.243569643749999010 ) ) ;
#27559 = FACE_OUTER_BOUND ( 'NONE', #33737, .T. ) ;
#27560 = CARTESIAN_POINT ( 'NONE',  ( 7.087499999999999467, -2.886751345948130876, 4.999999999999996447 ) ) ;
#27561 = CARTESIAN_POINT ( 'NONE',  ( 25.79062500061451502, -3.027376345333614438, 5.243569643749998122 ) ) ;
#27562 = CARTESIAN_POINT ( 'NONE',  ( 16.31250000122903288, -4.330127018922190985, -2.500000000000001332 ) ) ;
#27563 = CARTESIAN_POINT ( 'NONE',  ( 0.000000000000000000, 20.00000000000000000, 30.00000000000000000 ) ) ;
#27564 = CARTESIAN_POINT ( 'NONE',  ( 16.13437500061451502, 5.824947211148865298E-16, -4.756430356249998326 ) ) ;
#27565 = CARTESIAN_POINT ( 'NONE',  ( 2.803125000614518747, 0.000000000000000000, 5.243569643749999010 ) ) ;
#27566 = CARTESIAN_POINT ( 'NONE',  ( 21.15937500061451715, 4.541064518000418104, -2.621784821874998173 ) ) ;
#27567 = CARTESIAN_POINT ( 'NONE',  ( 4.243569643749999010, 13.82187500061451857, 27.54997392385601174 ) ) ;
#27568 = CARTESIAN_POINT ( 'NONE',  ( 22.47187500061451715, 3.027376345333613106, -5.243569643749998122 ) ) ;
#27569 = CARTESIAN_POINT ( 'NONE',  ( 3.862500000000001155, 2.886751345948126879, 4.999999999999999112 ) ) ;
#27570 = CARTESIAN_POINT ( 'NONE',  ( 10.46250000000000036, 2.886751345948129099, -4.999999999999997335 ) ) ;
#27571 = CARTESIAN_POINT ( 'NONE',  ( 8.765625000614518214, -6.054752690667223547, -1.112240025338166033E-15 ) ) ;
#27572 = CYLINDRICAL_SURFACE ( 'NONE', #39529, 5.000000000000000000 ) ;
#27573 = CARTESIAN_POINT ( 'NONE',  ( 6.421875000614519102, 3.027376345333611329, 5.243569643749999010 ) ) ;
#27574 = DIRECTION ( 'NONE',  ( -1.000000000000000000, -0.000000000000000000, -0.000000000000000000 ) ) ;
#27575 = CARTESIAN_POINT ( 'NONE',  ( 8.128125000614515372, 4.541064518000418104, 2.621784821874999949 ) ) ;
#27576 = CARTESIAN_POINT ( 'NONE',  ( 12.45937500061451786, -4.541064518000417216, -2.621784821875001281 ) ) ;
#27577 = CYLINDRICAL_SURFACE ( 'NONE', #9605, 4.999999999999998224 ) ;
#27578 = CARTESIAN_POINT ( 'NONE',  ( 18.45000000122903216, -2.886751345948129988, 4.999999999999997335 ) ) ;
#27579 = CARTESIAN_POINT ( 'NONE',  ( 8.746875000614515727, -3.027376345333614438, 5.243569643749998122 ) ) ;
#27580 = CARTESIAN_POINT ( 'NONE',  ( 10.07812500061451644, -4.541064518000419881, 2.621784821874995952 ) ) ;
#27581 = CARTESIAN_POINT ( 'NONE',  ( 6.778125000614518392, 4.541064518000418104, 2.621784821874999949 ) ) ;
#27582 = CARTESIAN_POINT ( 'NONE',  ( 25.66875000122903216, -5.773502691896255534, -1.060575238724906372E-15 ) ) ;
#27583 = CARTESIAN_POINT ( 'NONE',  ( 18.34687500061451715, -3.027376345333610441, -5.243569643749999898 ) ) ;
#27584 = CARTESIAN_POINT ( 'NONE',  ( 1.071796769724491893, 13.04509619066137027, 33.99999999999999289 ) ) ;
#27585 = CARTESIAN_POINT ( 'NONE',  ( 12.21562500061451573, 3.027376345333611329, 5.243569643749999010 ) ) ;
#27586 = EDGE_CURVE ( 'NONE', #64681, #23474, #14979, .T. ) ;
#27587 = CARTESIAN_POINT ( 'NONE',  ( 28.65937500061451715, -4.541064518000417216, -2.621784821875001281 ) ) ;
#27588 = CARTESIAN_POINT ( 'NONE',  ( 4.243569643749999898, 11.04687500061451644, -27.54997392385601529 ) ) ;
#27589 = CARTESIAN_POINT ( 'NONE',  ( 11.81250000122903465, -4.330127018922190985, -2.500000000000001332 ) ) ;
#27590 = CARTESIAN_POINT ( 'NONE',  ( 4.243569643749999898, 16.42812500061451786, -30.00000000000000000 ) ) ;
#27591 = CARTESIAN_POINT ( 'NONE',  ( 15.45000000122903216, -2.886751345948125991, -5.000000000000000000 ) ) ;
#27592 = CARTESIAN_POINT ( 'NONE',  ( 10.22812500061451679, 6.421520780324663323E-16, -5.243569643749999010 ) ) ;
#27593 = ORIENTED_EDGE ( 'NONE', *, *, #41247, .T. ) ;
#27594 = CARTESIAN_POINT ( 'NONE',  ( 13.16249999999999964, 2.886751345948129099, -4.999999999999998224 ) ) ;
#27595 = CARTESIAN_POINT ( 'NONE',  ( 45.00000000000000000, 0.000000000000000000, 0.000000000000000000 ) ) ;
#27596 = CARTESIAN_POINT ( 'NONE',  ( 22.52812500061451573, 4.541064518000418104, 2.621784821874999949 ) ) ;
#27597 = CARTESIAN_POINT ( 'NONE',  ( 8.034375000614518925, 6.421520780324663323E-16, -5.243569643749999010 ) ) ;
#27598 = CARTESIAN_POINT ( 'NONE',  ( 10.83750000122903501, -4.330127018922194537, 2.499999999999995559 ) ) ;
#27599 = CARTESIAN_POINT ( 'NONE',  ( 18.45000000122903216, -2.886751345948129988, 4.999999999999997335 ) ) ;
#27600 = CARTESIAN_POINT ( 'NONE',  ( 16.34062500061451573, -3.027376345333614438, 5.243569643749998122 ) ) ;
#27601 = CARTESIAN_POINT ( 'NONE',  ( 19.04062500061451146, -3.027376345333614438, 5.243569643749998122 ) ) ;
#27602 = CARTESIAN_POINT ( 'NONE',  ( 25.20000000122903216, -2.886751345948129988, 4.999999999999997335 ) ) ;
#27603 = CARTESIAN_POINT ( 'NONE',  ( 28.76250000122903216, 0.000000000000000000, 4.999999999999998224 ) ) ;
#27604 = CARTESIAN_POINT ( 'NONE',  ( 22.16250000000000142, 2.886751345948129099, -4.999999999999998224 ) ) ;
#27605 = CARTESIAN_POINT ( 'NONE',  ( -3.756430356250000102, 13.31562499938548427, 30.00000000000000000 ) ) ;
#27606 = CARTESIAN_POINT ( 'NONE',  ( 26.44687500061451502, -3.027376345333610441, -5.243569643749999898 ) ) ;
#27607 = CARTESIAN_POINT ( 'NONE',  ( 25.65000000122903856, -2.886751345948163738, 4.999999999999939604 ) ) ;
#27608 = CARTESIAN_POINT ( 'NONE',  ( 12.22500000122903430, -5.773502691896255534, -1.060575238724906372E-15 ) ) ;
#27609 = CARTESIAN_POINT ( 'NONE',  ( 27.15937500061451360, 0.000000000000000000, 5.243569643749999010 ) ) ;
#27610 = CARTESIAN_POINT ( 'NONE',  ( 4.546875000614517326, 6.054752690667223547, 3.707466751127219781E-16 ) ) ;
#27611 = CARTESIAN_POINT ( 'NONE',  ( 24.06562500061451715, -6.054752690667223547, -1.112240025338166033E-15 ) ) ;
#27612 = CARTESIAN_POINT ( 'NONE',  ( 3.756430356250000546, 13.69062499938548250, 27.83122392262697886 ) ) ;
#27613 = CARTESIAN_POINT ( 'NONE',  ( 3.486133158594716510E-16, 19.88749999999999929, -34.00000000000000000 ) ) ;
#27614 = CARTESIAN_POINT ( 'NONE',  ( 9.909375000614517148, 4.541064518000418104, -2.621784821874998173 ) ) ;
#27615 = B_SPLINE_CURVE_WITH_KNOTS ( 'NONE', 3,
 ( #70943, #20314, #54679, #9251, #42867, #37323, #72037, #48780, #15143, #14781 ),
 .UNSPECIFIED., .F., .F.,
 ( 4, 3, 3, 4 ),
 ( 6.133173666733496745E-19, 2.812507128105724141E-05, 5.625014365164849055E-05, 9.987238900461527181E-05 ),
 .UNSPECIFIED. ) ;
#27616 = CARTESIAN_POINT ( 'NONE',  ( 45.00000000000000000, 0.000000000000000000, 4.999999999999998224 ) ) ;
#27617 = CARTESIAN_POINT ( 'NONE',  ( 3.046875000614519990, -3.027376345333610441, -5.243569643749999898 ) ) ;
#27618 = CARTESIAN_POINT ( 'NONE',  ( 7.546875000614517326, -3.027376345333610441, -5.243569643749999898 ) ) ;
#27619 = CARTESIAN_POINT ( 'NONE',  ( 27.94687500061451502, 6.054752690667223547, 3.707466751127219781E-16 ) ) ;
#27620 = LINE ( 'NONE', #44625, #26673 ) ;
#27621 = CARTESIAN_POINT ( 'NONE',  ( 19.68750000000000355, -2.886751345948129988, 4.999999999999997335 ) ) ;
#27622 = ORIENTED_EDGE ( 'NONE', *, *, #11874, .T. ) ;
#27623 = CARTESIAN_POINT ( 'NONE',  ( 26.58750000000000213, -2.886751345948125991, -5.000000000000000000 ) ) ;
#27624 = EDGE_CURVE ( 'NONE', #35328, #28339, #53888, .T. ) ;
#27625 = CARTESIAN_POINT ( 'NONE',  ( 28.09687500061451360, -3.027376345333614438, 5.243569643749998122 ) ) ;
#27626 = ORIENTED_EDGE ( 'NONE', *, *, #36651, .F. ) ;
#27627 = CARTESIAN_POINT ( 'NONE',  ( 17.12812500061451715, 4.541064518000418104, 2.621784821874999949 ) ) ;
#27628 = CARTESIAN_POINT ( 'NONE',  ( 7.603125000614517681, 4.541064518000418104, -2.621784821874998173 ) ) ;
#27629 = CARTESIAN_POINT ( 'NONE',  ( 22.47187500061451360, 4.119189519843966529, 2.378215178124999607 ) ) ;
#27630 = CARTESIAN_POINT ( 'NONE',  ( 5.709375000614517859, -4.541064518000417216, -2.621784821875001281 ) ) ;
#27631 = CARTESIAN_POINT ( 'NONE',  ( 18.78750000122903430, 4.330127018922191873, 2.499999999999999556 ) ) ;
#27632 = CARTESIAN_POINT ( 'NONE',  ( 3.999999999999998668, 19.66249999999999787, 32.30940107675850470 ) ) ;
#27633 = CARTESIAN_POINT ( 'NONE',  ( 7.471875000614519813, -6.054752690667223547, -1.112240025338166033E-15 ) ) ;
#27634 = CARTESIAN_POINT ( 'NONE',  ( 10.99687500061451750, -3.027376345333614438, 5.243569643749998122 ) ) ;
#27635 = CARTESIAN_POINT ( 'NONE',  ( 20.67187500061451289, 3.027376345333613106, -5.243569643749998122 ) ) ;
#27636 = ORIENTED_EDGE ( 'NONE', *, *, #52167, .T. ) ;
#27637 = CARTESIAN_POINT ( 'NONE',  ( 11.81250000000000000, 2.886751345948129099, -4.999999999999998224 ) ) ;
#27638 = CARTESIAN_POINT ( 'NONE',  ( 6.346875000614517148, 6.054752690667223547, 3.707466751127219781E-16 ) ) ;
#27639 = CARTESIAN_POINT ( 'NONE',  ( -1.878215178125001827, 15.64062499938548356, 33.25316411605952283 ) ) ;
#27640 = CARTESIAN_POINT ( 'NONE',  ( 20.28750000000000142, -2.886751345948125991, -5.000000000000000000 ) ) ;
#27641 = CARTESIAN_POINT ( 'NONE',  ( 17.39062500061451644, -3.027376345333610441, -5.243569643749999898 ) ) ;
#27642 = CARTESIAN_POINT ( 'NONE',  ( -3.999999999999999556, 17.63749999999999929, 27.69059892324149175 ) ) ;
#27643 = CARTESIAN_POINT ( 'NONE',  ( 2.121784821874999061, 10.70937500061451964, -33.67503911421598417 ) ) ;
#27644 = CARTESIAN_POINT ( 'NONE',  ( 22.05937500061451573, 4.119189519843966529, -2.378215178124998275 ) ) ;
#27645 = CARTESIAN_POINT ( 'NONE',  ( 12.25312500061451537, 0.000000000000000000, 5.243569643749999010 ) ) ;
#27646 = CARTESIAN_POINT ( 'NONE',  ( 28.02187500061451431, 3.027376345333611329, 5.243569643749999010 ) ) ;
#27647 = CARTESIAN_POINT ( 'NONE',  ( 28.25625000122903074, 0.000000000000000000, 4.999999999999998224 ) ) ;
#27648 = CARTESIAN_POINT ( 'NONE',  ( 28.65937500061451715, -4.541064518000417216, -2.621784821875001281 ) ) ;
#27649 = CARTESIAN_POINT ( 'NONE',  ( 10.72500000000000142, -4.330127018922194537, 2.499999999999995559 ) ) ;
#27650 = CARTESIAN_POINT ( 'NONE',  ( -2.000000000000000000, 15.98750000122903181, 26.53589838486224650 ) ) ;
#27651 = CARTESIAN_POINT ( 'NONE',  ( 8.850000001229034297, 5.773502691896255534, 3.535250795749688894E-16 ) ) ;
#27652 = CARTESIAN_POINT ( 'NONE',  ( 20.40937500061451715, 0.000000000000000000, 5.243569643749999010 ) ) ;
#27653 = CARTESIAN_POINT ( 'NONE',  ( 15.38437500061451679, 4.541064518000418104, 2.621784821874999949 ) ) ;
#27654 = CARTESIAN_POINT ( 'NONE',  ( -3.999999999999999112, 12.31250000000000000, 27.69059892324149885 ) ) ;
#27655 = VERTEX_POINT ( 'NONE', #9179 ) ;
#27656 = CARTESIAN_POINT ( 'NONE',  ( 15.59062500061451573, -3.027376345333610441, -5.243569643749999898 ) ) ;
#27657 = CARTESIAN_POINT ( 'NONE',  ( 29.47500000122903430, 2.886751345948129099, -4.999999999999998224 ) ) ;
#27658 = CARTESIAN_POINT ( 'NONE',  ( 16.13437500061451502, 6.421520780324663323E-16, -5.243569643749999010 ) ) ;
#27659 = CARTESIAN_POINT ( 'NONE',  ( 27.28125000122902932, 4.330127018922191873, 2.499999999999999556 ) ) ;
#27660 = CARTESIAN_POINT ( 'NONE',  ( 18.06562500061451715, 3.027376345333611329, 5.243569643749999010 ) ) ;
#27661 = DIRECTION ( 'NONE',  ( -0.000000000000000000, -1.000000000000000000, -0.000000000000000000 ) ) ;
#27662 = CARTESIAN_POINT ( 'NONE',  ( 26.93437500061451573, 6.421520780324663323E-16, -5.243569643749999010 ) ) ;
#27663 = CYLINDRICAL_SURFACE ( 'NONE', #8917, 4.000000000000000000 ) ;
#27664 = CARTESIAN_POINT ( 'NONE',  ( 15.19687500061451857, -3.027376345333610441, -5.243569643749999898 ) ) ;
#27665 = CARTESIAN_POINT ( 'NONE',  ( 14.92500000122903181, -5.773502691896255534, -1.060575238724906372E-15 ) ) ;
#27666 = CARTESIAN_POINT ( 'NONE',  ( 9.009375000614518569, 4.119189519843966529, -2.378215178124998275 ) ) ;
#27667 = CARTESIAN_POINT ( 'NONE',  ( 3.323491336998473322, -3.735569206101108986, 3.679756774564975519 ) ) ;
#27668 = CARTESIAN_POINT ( 'NONE',  ( 19.54687500061451644, -3.027376345333614438, 5.243569643749998122 ) ) ;
#27669 = CARTESIAN_POINT ( 'NONE',  ( 22.01250000122903216, 0.000000000000000000, 4.999999999999998224 ) ) ;
#27670 = EDGE_CURVE ( 'NONE', #38854, #58120, #22536, .T. ) ;
#27671 = CARTESIAN_POINT ( 'NONE',  ( 18.15937500061451715, 0.000000000000000000, 5.243569643749999010 ) ) ;
#27672 = CARTESIAN_POINT ( 'NONE',  ( 4.243569643749999898, 11.53437500061451892, 30.00000000000000000 ) ) ;
#27673 = CARTESIAN_POINT ( 'NONE',  ( 18.21562500061451573, -6.054752690667223547, -1.112240025338166033E-15 ) ) ;
#27674 = ORIENTED_EDGE ( 'NONE', *, *, #7253, .T. ) ;
#27675 = VERTEX_POINT ( 'NONE', #2904 ) ;
#27676 = CARTESIAN_POINT ( 'NONE',  ( 20.40000000000000213, 4.330127018922192761, -2.499999999999997780 ) ) ;
#27677 = CARTESIAN_POINT ( 'NONE',  ( 28.08750000122903145, 6.123233995736764310E-16, -4.999999999999998224 ) ) ;
#27678 = CARTESIAN_POINT ( 'NONE',  ( 23.46562500061451573, 3.027376345333611329, 5.243569643749999010 ) ) ;
#27679 = CARTESIAN_POINT ( 'NONE',  ( 5.803125000614517859, 4.541064518000418104, -2.621784821874998173 ) ) ;
#27680 = CARTESIAN_POINT ( 'NONE',  ( 16.31250000122903288, -4.330127018922190985, -2.500000000000001332 ) ) ;
#27681 = CARTESIAN_POINT ( 'NONE',  ( 21.96562500061451573, 3.027376345333613106, -5.243569643749998122 ) ) ;
#27682 = CARTESIAN_POINT ( 'NONE',  ( 19.68750000000000355, -2.886751345948129988, 4.999999999999997335 ) ) ;
#27683 =( BOUNDED_CURVE ( )  B_SPLINE_CURVE ( 2, ( #53672, #14137, #52576, #19298, #52215, #18933, #18208 ),
 .UNSPECIFIED., .F., .F. ) 
 B_SPLINE_CURVE_WITH_KNOTS ( ( 3, 2, 2, 3 ),
 ( 0.2416666666666666963, 0.2444444444444444642, 0.2472222222222222321, 0.2500000000000000000 ),
 .UNSPECIFIED. ) 
 CURVE ( )  GEOMETRIC_REPRESENTATION_ITEM ( )  RATIONAL_B_SPLINE_CURVE ( ( 0.9999999999999986677, 0.8660254037844400399, 1.000000000000000000, 0.8660254037844387076, 1.000000000000000000, 0.8660254037844387076, 1.000000000000000000 ) ) 
 REPRESENTATION_ITEM ( '' )  );
#27684 = CARTESIAN_POINT ( 'NONE',  ( 26.16562500061451502, 3.027376345333611329, 5.243569643749999010 ) ) ;
#27685 = CARTESIAN_POINT ( 'NONE',  ( 5.765625000614519102, 3.027376345333613106, -5.243569643749998122 ) ) ;
#27686 = ORIENTED_EDGE ( 'NONE', *, *, #61290, .F. ) ;
#27687 = CARTESIAN_POINT ( 'NONE',  ( -5.810221930991193690E-16, 14.48749999999999893, -34.00000000000000000 ) ) ;
#27688 = CARTESIAN_POINT ( 'NONE',  ( 2.953125000614516438, -4.541064518000417216, -2.621784821875001281 ) ) ;
#27689 = CARTESIAN_POINT ( 'NONE',  ( 11.78437500061451892, 4.119189519843966529, 2.378215178124999607 ) ) ;
#27690 = CARTESIAN_POINT ( 'NONE',  ( 2.000000000000001332, 18.80000000000000071, 33.46410161513774995 ) ) ;
#27691 = CARTESIAN_POINT ( 'NONE',  ( -2.828200636599751609E-16, 10.55000000122903359, -34.61880215351700230 ) ) ;
#27692 = CARTESIAN_POINT ( 'NONE',  ( -2.121784821874996840, 19.48437500061451644, -26.32496088578401583 ) ) ;
#27693 = CARTESIAN_POINT ( 'NONE',  ( 9.000000000000001776, -4.330127018922190985, -2.500000000000001332 ) ) ;
#27694 = CARTESIAN_POINT ( 'NONE',  ( 9.721875000614517148, -6.054752690667223547, -1.112240025338166033E-15 ) ) ;
#27695 = CARTESIAN_POINT ( 'NONE',  ( 6.337500001229033231, -4.330127018922194537, 2.499999999999995559 ) ) ;
#27696 = CARTESIAN_POINT ( 'NONE',  ( 12.27187500061451786, 3.027376345333611329, 5.243569643749999010 ) ) ;
#27697 = CARTESIAN_POINT ( 'NONE',  ( 3.159375000614518036, 4.541064518000418104, -2.621784821874998173 ) ) ;
#27698 = CARTESIAN_POINT ( 'NONE',  ( 1.071796769724490117, 18.89509619066136992, 33.99999999999999289 ) ) ;
#27699 = VECTOR ( 'NONE', #33048, 1000.000000000000000 ) ;
#27700 = CARTESIAN_POINT ( 'NONE',  ( 0.000000000000000000, -10.00000000000000000, 0.000000000000000000 ) ) ;
#27701 = CARTESIAN_POINT ( 'NONE',  ( 9.046875000614518214, 6.054752690667223547, 3.707466751127219781E-16 ) ) ;
#27702 = CARTESIAN_POINT ( 'NONE',  ( 1.626862140677534273E-15, 18.76250000000000284, -26.00000000000000355 ) ) ;
#27703 = CARTESIAN_POINT ( 'NONE',  ( 20.61562500061451431, 3.027376345333613106, -5.243569643749998122 ) ) ;
#27704 = CARTESIAN_POINT ( 'NONE',  ( 4.612500001229032698, -4.330127018922190985, -2.500000000000001332 ) ) ;
#27705 = CARTESIAN_POINT ( 'NONE',  ( -4.243569643749999898, 17.96562500061459389, 27.54997392385601529 ) ) ;
#27706 = CARTESIAN_POINT ( 'NONE',  ( 22.88437500061451857, 6.421520780324663323E-16, -5.243569643749999010 ) ) ;
#27707 = CARTESIAN_POINT ( 'NONE',  ( 9.525000000000002132, 6.123233995736764310E-16, -4.999999999999998224 ) ) ;
#27708 = CARTESIAN_POINT ( 'NONE',  ( 29.55000000122903003, 5.773502691896255534, 3.535250795749688894E-16 ) ) ;
#27709 = VECTOR ( 'NONE', #21271, 1000.000000000000000 ) ;
#27710 = CARTESIAN_POINT ( 'NONE',  ( 20.40937500061451360, -5.492252693125287522, -1.008910452111647106E-15 ) ) ;
#27711 = CARTESIAN_POINT ( 'NONE',  ( 24.96562500061451573, -6.054752690667223547, -1.112240025338166033E-15 ) ) ;
#27712 = CARTESIAN_POINT ( 'NONE',  ( 15.66562500061451857, 3.027376345333613106, -5.243569643749998122 ) ) ;
#27713 = CARTESIAN_POINT ( 'NONE',  ( 13.21875000122903288, 2.886751345948129099, -4.999999999999998224 ) ) ;
#27714 = CARTESIAN_POINT ( 'NONE',  ( 13.69687500061451679, -3.027376345333614438, 5.243569643749998122 ) ) ;
#27715 = CYLINDRICAL_SURFACE ( 'NONE', #35968, 1.500000000000000444 ) ;
#27716 = CARTESIAN_POINT ( 'NONE',  ( 24.56250000122903288, 4.330127018922192761, -2.499999999999997780 ) ) ;
#27717 = CARTESIAN_POINT ( 'NONE',  ( 3.384375000614517237, -4.541064518000419881, 2.621784821874995952 ) ) ;
#27718 = AXIS2_PLACEMENT_3D ( 'NONE', #58655, #52764, #8790 ) ;
#27719 = CARTESIAN_POINT ( 'NONE',  ( 13.17187500061451999, 3.027376345333611329, 5.243569643749999010 ) ) ;
#27720 = CARTESIAN_POINT ( 'NONE',  ( 14.96250000000000036, 2.886751345948129099, -4.999999999999997335 ) ) ;
#27721 = CARTESIAN_POINT ( 'NONE',  ( 30.00000000000000000, 0.000000000000000000, 0.000000000000000000 ) ) ;
#27722 = CARTESIAN_POINT ( 'NONE',  ( -5.810221930991193690E-16, 11.90000000122903501, 26.00000000000000355 ) ) ;
#27723 = CARTESIAN_POINT ( 'NONE',  ( 25.62187500061451573, 3.027376345333613106, -5.243569643749998122 ) ) ;
#27724 = CARTESIAN_POINT ( 'NONE',  ( 15.49687500061451750, -3.027376345333614438, 5.243569643749998122 ) ) ;
#27725 = CARTESIAN_POINT ( 'NONE',  ( 3.756430356249998770, 14.96562499938548108, 32.16877607737302469 ) ) ;
#27726 = CARTESIAN_POINT ( 'NONE',  ( 27.15000000000000213, 4.330127018922192761, -2.499999999999997780 ) ) ;
#27727 = CARTESIAN_POINT ( 'NONE',  ( 4.275000001229035895, 2.886751345948129099, -4.999999999999998224 ) ) ;
#27728 = CARTESIAN_POINT ( 'NONE',  ( 6.675000000000000711, -4.330127018922194537, 2.499999999999995559 ) ) ;
#27729 = CARTESIAN_POINT ( 'NONE',  ( 29.44687500061451857, -2.746126346562646425, 4.756430356249996549 ) ) ;
#27730 = CARTESIAN_POINT ( 'NONE',  ( 20.50312500061451715, -4.541064518000417216, -2.621784821875001281 ) ) ;
#27731 = CARTESIAN_POINT ( 'NONE',  ( 9.150000000000002132, 4.330127018922192761, -2.499999999999997780 ) ) ;
#27732 = CARTESIAN_POINT ( 'NONE',  ( -5.810221930991193690E-16, 13.70000000122903394, 26.00000000000000355 ) ) ;
#27733 =( BOUNDED_CURVE ( )  B_SPLINE_CURVE ( 2, ( #386, #22541, #67624, #40913, #63426, #28453, #12813 ),
 .UNSPECIFIED., .F., .F. ) 
 B_SPLINE_CURVE_WITH_KNOTS ( ( 3, 2, 2, 3 ),
 ( 0.8100000000000000533, 0.8133333333333333526, 0.8166666666666667629, 0.8200000000000000622 ),
 .UNSPECIFIED. ) 
 CURVE ( )  GEOMETRIC_REPRESENTATION_ITEM ( )  RATIONAL_B_SPLINE_CURVE ( ( 1.000000000000000000, 0.8660254037844387076, 1.000000000000000000, 0.8660254037844387076, 1.000000000000000000, 0.8660254037844342667, 1.000000000000004441 ) ) 
 REPRESENTATION_ITEM ( '' )  );
#27734 = CARTESIAN_POINT ( 'NONE',  ( 17.58749999999999858, -2.886751345948125991, -5.000000000000000000 ) ) ;
#27735 = CARTESIAN_POINT ( 'NONE',  ( -3.999999999999997335, 17.33749999999999858, 32.30940107675850470 ) ) ;
#27736 = CARTESIAN_POINT ( 'NONE',  ( 20.25000000122903288, -2.886751345948129988, 4.999999999999997335 ) ) ;
#27737 = CARTESIAN_POINT ( 'NONE',  ( 14.92500000000000071, 6.123233995736764310E-16, -4.999999999999998224 ) ) ;
#27738 = CARTESIAN_POINT ( 'NONE',  ( 27.23437500061451644, -4.541064518000419881, 2.621784821874995952 ) ) ;
#27739 = ORIENTED_EDGE ( 'NONE', *, *, #53141, .T. ) ;
#27740 = CARTESIAN_POINT ( 'NONE',  ( 16.04062500061451857, -3.027376345333610441, -5.243569643749999898 ) ) ;
#27741 = CARTESIAN_POINT ( 'NONE',  ( 22.07812500061451644, 4.541064518000418104, 2.621784821874999949 ) ) ;
#27742 = CARTESIAN_POINT ( 'NONE',  ( 23.59687500061451715, -3.027376345333614438, 5.243569643749998122 ) ) ;
#27743 = CARTESIAN_POINT ( 'NONE',  ( 7.200000000000001954, -4.330127018922190985, -2.500000000000001332 ) ) ;
#27744 = CARTESIAN_POINT ( 'NONE',  ( 8.353125000614518569, -4.541064518000417216, -2.621784821875001281 ) ) ;
#27745 = CARTESIAN_POINT ( 'NONE',  ( 23.57812500061451289, -4.541064518000419881, 2.621784821874995952 ) ) ;
#27746 = CARTESIAN_POINT ( 'NONE',  ( 14.07187500061451679, 3.027376345333611329, 5.243569643749999010 ) ) ;
#27747 = CARTESIAN_POINT ( 'NONE',  ( 19.28437500061451360, 6.421520780324663323E-16, -5.243569643749999010 ) ) ;
#27748 = CARTESIAN_POINT ( 'NONE',  ( -5.810221930991193690E-16, 12.35000000122903430, -34.00000000000000000 ) ) ;
#27749 = CARTESIAN_POINT ( 'NONE',  ( -2.121784821874996840, 18.97812500061451857, 33.67503911421598417 ) ) ;
#27750 = CARTESIAN_POINT ( 'NONE',  ( 20.62500000122903288, 2.886751345948126879, 4.999999999999999112 ) ) ;
#27751 = CARTESIAN_POINT ( 'NONE',  ( 16.28437500061452070, 4.119189519843966529, 2.378215178124999607 ) ) ;
#27752 = CARTESIAN_POINT ( 'NONE',  ( 12.66562500061451502, 3.027376345333611329, 5.243569643749999010 ) ) ;
#27753 = CARTESIAN_POINT ( 'NONE',  ( 6.009375000614519458, 0.000000000000000000, 5.243569643749999010 ) ) ;
#27754 = CARTESIAN_POINT ( 'NONE',  ( 6.271875000614517859, 3.027376345333613106, -5.243569643749998122 ) ) ;
#27755 = EDGE_LOOP ( 'NONE', ( #7214, #66012, #21831, #4946 ) ) ;
#27756 = CARTESIAN_POINT ( 'NONE',  ( 27.57187500061451857, 3.027376345333611329, 5.243569643749999010 ) ) ;
#27757 = CARTESIAN_POINT ( 'NONE',  ( 19.30312500061451786, 4.541064518000418104, -2.621784821874998173 ) ) ;
#27758 = CARTESIAN_POINT ( 'NONE',  ( 28.95000000122903572, -2.886751345948125991, -5.000000000000000000 ) ) ;
#27759 = EDGE_CURVE ( 'NONE', #61054, #16658, #48709, .T. ) ;
#27760 = CARTESIAN_POINT ( 'NONE',  ( 26.87812500061451360, 6.421520780324663323E-16, -5.243569643749999010 ) ) ;
#27761 = CARTESIAN_POINT ( 'NONE',  ( 23.29687500061451644, -3.027376345333610441, -5.243569643749999898 ) ) ;
#27762 = CARTESIAN_POINT ( 'NONE',  ( 18.55312500061451431, 0.000000000000000000, 5.243569643749999010 ) ) ;
#27763 = CARTESIAN_POINT ( 'NONE',  ( 4.243569643749999898, 18.73437500061451644, 30.00000000000000000 ) ) ;
#27764 = CARTESIAN_POINT ( 'NONE',  ( 24.44062500061451715, -3.027376345333614438, 5.243569643749998122 ) ) ;
#27765 = CARTESIAN_POINT ( 'NONE',  ( 5.062500001229035540, -4.330127018922190985, -2.500000000000001332 ) ) ;
#27766 = VERTEX_POINT ( 'NONE', #42796 ) ;
#27767 = CARTESIAN_POINT ( 'NONE',  ( 28.61249999999999716, 2.886751345948126879, 4.999999999999999112 ) ) ;
#27768 = CARTESIAN_POINT ( 'NONE',  ( 4.000000000000000000, 15.23750000000000071, -27.69059892324149530 ) ) ;
#27769 = CARTESIAN_POINT ( 'NONE',  ( -1.878215178124999163, 17.40312499938548285, 26.74683588394047007 ) ) ;
#27770 = CARTESIAN_POINT ( 'NONE',  ( 4.884375000614518569, 6.421520780324663323E-16, -5.243569643749999010 ) ) ;
#27771 = CARTESIAN_POINT ( 'NONE',  ( 12.36562500061451608, -6.054752690667223547, -1.112240025338166033E-15 ) ) ;
#27772 = CARTESIAN_POINT ( 'NONE',  ( 6.159375000614517148, -4.541064518000417216, -2.621784821875001281 ) ) ;
#27773 = CARTESIAN_POINT ( 'NONE',  ( 24.97500000122903430, 2.886751345948129099, -4.999999999999998224 ) ) ;
#27774 = AXIS2_PLACEMENT_3D ( 'NONE', #45261, #46343, #24155 ) ;
#27775 = CARTESIAN_POINT ( 'NONE',  ( 16.13437500061451502, 6.421520780324663323E-16, -5.243569643749999010 ) ) ;
#27776 = CARTESIAN_POINT ( 'NONE',  ( 29.42812500061451431, -4.541064518000419881, 2.621784821874995952 ) ) ;
#27777 = CARTESIAN_POINT ( 'NONE',  ( 27.00000000000000000, -4.330127018922190985, -2.500000000000001332 ) ) ;
#27778 = CARTESIAN_POINT ( 'NONE',  ( 25.95937500061451431, -4.541064518000417216, -2.621784821875001281 ) ) ;
#27779 = CARTESIAN_POINT ( 'NONE',  ( 4.153125000614515727, 0.000000000000000000, 5.243569643749999010 ) ) ;
#27780 = CARTESIAN_POINT ( 'NONE',  ( 13.56562500061451892, 3.027376345333611329, 5.243569643749999010 ) ) ;
#27781 = ORIENTED_EDGE ( 'NONE', *, *, #33711, .T. ) ;
#27782 = AXIS2_PLACEMENT_3D ( 'NONE', #29781, #52317, #1720 ) ;
#27783 = CARTESIAN_POINT ( 'NONE',  ( 11.24062500061451608, 6.054752690667223547, 3.707466751127219781E-16 ) ) ;
#27784 = AXIS2_PLACEMENT_3D ( 'NONE', #18985, #64064, #23095 ) ;
#27785 = CARTESIAN_POINT ( 'NONE',  ( 9.290625000614515017, -3.027376345333610441, -5.243569643749999898 ) ) ;
#27786 = CARTESIAN_POINT ( 'NONE',  ( 19.32187500061451857, 2.746126346562645981, -4.756430356249997438 ) ) ;
#27787 = CARTESIAN_POINT ( 'NONE',  ( 14.56875000122903252, 2.886751345948129099, -4.999999999999997335 ) ) ;
#27788 = CARTESIAN_POINT ( 'NONE',  ( 16.50000000000000000, 0.000000000000000000, 4.999999999999998224 ) ) ;
#27789 = CARTESIAN_POINT ( 'NONE',  ( 16.20937500061451786, 4.541064518000418104, -2.621784821874998173 ) ) ;
#27790 = CARTESIAN_POINT ( 'NONE',  ( 12.71250000122903145, -4.330127018922190985, -2.500000000000001332 ) ) ;
#27791 = CARTESIAN_POINT ( 'NONE',  ( 19.31250000000000000, -5.773502691896255534, -1.060575238724906372E-15 ) ) ;
#27792 = CARTESIAN_POINT ( 'NONE',  ( 22.02187500061452141, 3.027376345333613106, -5.243569643749998122 ) ) ;
#27793 = CARTESIAN_POINT ( 'NONE',  ( -4.243569643749999898, 13.01562500061451999, -32.45002607614398471 ) ) ;
#27794 = DIRECTION ( 'NONE',  ( -0.000000000000000000, -1.000000000000000000, -0.000000000000000000 ) ) ;
#27795 = CARTESIAN_POINT ( 'NONE',  ( 26.33437500061451431, -2.746126346562641984, -4.756430356249999214 ) ) ;
#27796 = CARTESIAN_POINT ( 'NONE',  ( 14.30625000122903145, 0.000000000000000000, 4.999999999999998224 ) ) ;
#27797 = CARTESIAN_POINT ( 'NONE',  ( 27.89062500061451289, 6.054752690667223547, 3.707466751127219781E-16 ) ) ;
#27798 = CARTESIAN_POINT ( 'NONE',  ( 0.000000000000000000, 20.00000000000000000, -33.99999999999999289 ) ) ;
#27799 = DIRECTION ( 'NONE',  ( 1.000000000000000000, 0.000000000000000000, 0.000000000000000000 ) ) ;
#27800 = CARTESIAN_POINT ( 'NONE',  ( 27.82499999999999929, -4.330127018922194537, 2.499999999999995559 ) ) ;
#27801 = EDGE_CURVE ( 'NONE', #5961, #40656, #25060, .T. ) ;
#27802 = CARTESIAN_POINT ( 'NONE',  ( 10.22812500061451679, 6.421520780324663323E-16, -5.243569643749999010 ) ) ;
#27803 = CARTESIAN_POINT ( 'NONE',  ( 27.49687500061451573, 0.000000000000000000, 4.756430356249998326 ) ) ;
#27804 = CARTESIAN_POINT ( 'NONE',  ( 20.67187500061451289, 3.027376345333613106, -5.243569643749998122 ) ) ;
#27805 = CARTESIAN_POINT ( 'NONE',  ( 12.53437500061451537, 5.492252693125287522, 3.363034840372157021E-16 ) ) ;
#27806 = ADVANCED_FACE ( 'NONE', ( #59773 ), #25807, .T. ) ;
#27807 = AXIS2_PLACEMENT_3D ( 'NONE', #4751, #49818, #26551 ) ;
#27808 = CARTESIAN_POINT ( 'NONE',  ( 5.203125000614518214, -4.541064518000417216, -2.621784821875001281 ) ) ;
#27809 = CARTESIAN_POINT ( 'NONE',  ( 11.59687500061451892, -3.027376345333610441, -5.243569643749999898 ) ) ;
#27810 = ORIENTED_EDGE ( 'NONE', *, *, #39698, .T. ) ;
#27811 = CARTESIAN_POINT ( 'NONE',  ( 22.02187500061452141, 3.027376345333613106, -5.243569643749998122 ) ) ;
#27812 = FACE_OUTER_BOUND ( 'NONE', #30421, .T. ) ;
#27813 = CARTESIAN_POINT ( 'NONE',  ( 28.91250000000000497, 2.886751345948129099, -4.999999999999998224 ) ) ;
#27814 = CARTESIAN_POINT ( 'NONE',  ( 3.975000000000002753, -4.330127018922194537, 2.499999999999995559 ) ) ;
#27815 = CARTESIAN_POINT ( 'NONE',  ( 15.63750000122903216, 4.330127018922191873, 2.499999999999999556 ) ) ;
#27816 = CARTESIAN_POINT ( 'NONE',  ( 18.01875000122903003, -5.773502691896255534, -1.060575238724906372E-15 ) ) ;
#27817 = CARTESIAN_POINT ( 'NONE',  ( 17.36250000000000071, 2.886751345948161074, 4.999999999999941380 ) ) ;
#27818 = ORIENTED_EDGE ( 'NONE', *, *, #49856, .F. ) ;
#27819 = CARTESIAN_POINT ( 'NONE',  ( 13.57500000000000107, 6.123233995736764310E-16, -4.999999999999998224 ) ) ;
#27820 = CARTESIAN_POINT ( 'NONE',  ( 17.47499999999999787, -4.330127018922194537, 2.499999999999995559 ) ) ;
#27821 = ADVANCED_FACE ( 'NONE', ( #26539 ), #20611, .F. ) ;
#27822 = CARTESIAN_POINT ( 'NONE',  ( 12.30000000122903181, -2.886751345948125991, -5.000000000000000000 ) ) ;
#27823 = CARTESIAN_POINT ( 'NONE',  ( 10.26562500061451644, 3.027376345333613106, -5.243569643749998122 ) ) ;
#27824 = VECTOR ( 'NONE', #19685, 1000.000000000000000 ) ;
#27825 = CARTESIAN_POINT ( 'NONE',  ( 8.699999999999999289, 4.330127018922192761, -2.499999999999997780 ) ) ;
#27826 = CARTESIAN_POINT ( 'NONE',  ( 26.17500000000000071, 6.123233995736764310E-16, -4.999999999999998224 ) ) ;
#27827 = CARTESIAN_POINT ( 'NONE',  ( 4.243569643749999898, 15.54687500061451644, -27.54997392385601529 ) ) ;
#27828 = CARTESIAN_POINT ( 'NONE',  ( 27.30000000122903359, 5.773502691896255534, 3.535250795749688894E-16 ) ) ;
#27829 = CARTESIAN_POINT ( 'NONE',  ( -3.756430356250000990, 14.25312499938548250, 32.16877607737301048 ) ) ;
#27830 = CARTESIAN_POINT ( 'NONE',  ( 6.412500000000001421, 2.886751345948129099, -4.999999999999998224 ) ) ;
#27831 = CARTESIAN_POINT ( 'NONE',  ( 16.18125000122903145, -4.330127018922194537, 2.499999999999995559 ) ) ;
#27832 = VERTEX_POINT ( 'NONE', #59038 ) ;
#27833 = CARTESIAN_POINT ( 'NONE',  ( 24.66562500061451502, 3.027376345333613106, -5.243569643749998122 ) ) ;
#27834 = CARTESIAN_POINT ( 'NONE',  ( 1.071796769724491893, 13.38259618943233598, -26.00000000000000355 ) ) ;
#27835 = VECTOR ( 'NONE', #7440, 1000.000000000000000 ) ;
#27836 = FACE_OUTER_BOUND ( 'NONE', #16941, .T. ) ;
#27837 = CARTESIAN_POINT ( 'NONE',  ( 22.35937500061451644, -4.541064518000417216, -2.621784821875001281 ) ) ;
#27838 = EDGE_CURVE ( 'NONE', #69794, #68418, #52750, .T. ) ;
#27839 = CARTESIAN_POINT ( 'NONE',  ( 15.77812500061451573, 4.541064518000418104, 2.621784821874999949 ) ) ;
#27840 = CARTESIAN_POINT ( 'NONE',  ( 4.243569643749999010, 10.61562500061459602, -32.45002607614398471 ) ) ;
#27841 = CARTESIAN_POINT ( 'NONE',  ( 7.678125000614516082, 4.541064518000418104, 2.621784821874999949 ) ) ;
#27842 = CARTESIAN_POINT ( 'NONE',  ( 28.42500000122904069, -5.773502691896255534, -1.060575238724906372E-15 ) ) ;
#27843 = CARTESIAN_POINT ( 'NONE',  ( 25.39687500061451431, -2.746126346562646425, 4.756430356249996549 ) ) ;
#27844 = CARTESIAN_POINT ( 'NONE',  ( 19.67812500061451786, 6.421520780324663323E-16, -5.243569643749999010 ) ) ;
#27845 = CARTESIAN_POINT ( 'NONE',  ( 8.671875000614518214, 2.746126346562643317, 4.756430356249998326 ) ) ;
#27846 = CARTESIAN_POINT ( 'NONE',  ( 3.756430356250000546, 18.07812499938548711, 27.83122392262697886 ) ) ;
#27847 = CARTESIAN_POINT ( 'NONE',  ( 14.70937500061451786, -4.541064518000417216, -2.621784821875001281 ) ) ;
#27848 = CARTESIAN_POINT ( 'NONE',  ( 13.54687500061451999, 6.054752690667223547, 3.707466751127219781E-16 ) ) ;
#27849 = CARTESIAN_POINT ( 'NONE',  ( 21.60937500061451644, 4.541064518000418104, -2.621784821874998173 ) ) ;
#27850 = ORIENTED_EDGE ( 'NONE', *, *, #16519, .F. ) ;
#27851 = CARTESIAN_POINT ( 'NONE',  ( 3.703125000614516882, 0.000000000000000000, 5.243569643749999010 ) ) ;
#27852 = CARTESIAN_POINT ( 'NONE',  ( 26.72812500061451502, -4.541064518000419881, 2.621784821874995952 ) ) ;
#27853 = CARTESIAN_POINT ( 'NONE',  ( 26.61562500061451786, 3.027376345333611329, 5.243569643749999010 ) ) ;
#27854 = CARTESIAN_POINT ( 'NONE',  ( 8.484601909799253346E-16, 17.41250000000000142, 34.61880215351700230 ) ) ;
#27855 = CARTESIAN_POINT ( 'NONE',  ( 5.409375000614516260, 4.541064518000418104, -2.621784821874998173 ) ) ;
#27856 = ITEM_DEFINED_TRANSFORMATION ( 'NONE', 'NONE', #32064,  #23765 ) ;
#27857 = CARTESIAN_POINT ( 'NONE',  ( 12.63750000122903394, -4.330127018922194537, 2.499999999999995559 ) ) ;
#27858 = CARTESIAN_POINT ( 'NONE',  ( 6.187500001229032875, 4.330127018922191873, 2.499999999999999556 ) ) ;
#27859 = CARTESIAN_POINT ( 'NONE',  ( 28.76250000122903216, 0.000000000000000000, 4.999999999999998224 ) ) ;
#27860 = CARTESIAN_POINT ( 'NONE',  ( -3.999999999999999556, 18.48124999877096997, 27.69059892324149175 ) ) ;
#27861 = CARTESIAN_POINT ( 'NONE',  ( 18.91875000122903216, -5.773502691896255534, -1.060575238724906372E-15 ) ) ;
#27862 = CARTESIAN_POINT ( 'NONE',  ( 12.45937500061451786, -4.541064518000417216, -2.621784821875001281 ) ) ;
#27863 = ORIENTED_EDGE ( 'NONE', *, *, #65098, .T. ) ;
#27864 = CARTESIAN_POINT ( 'NONE',  ( 20.65312500061451573, 4.541064518000418104, -2.621784821874998173 ) ) ;
#27865 = CARTESIAN_POINT ( 'NONE',  ( 14.25937500061451679, -4.541064518000417216, -2.621784821875001281 ) ) ;
#27866 = CARTESIAN_POINT ( 'NONE',  ( 4.753125000614515372, -4.541064518000417216, -2.621784821875001281 ) ) ;
#27867 = CARTESIAN_POINT ( 'NONE',  ( 21.42187500061451644, -6.054752690667223547, -1.112240025338166033E-15 ) ) ;
#27868 = CARTESIAN_POINT ( 'NONE',  ( 9.384375000614518569, 6.421520780324663323E-16, -5.243569643749999010 ) ) ;
#27869 = CARTESIAN_POINT ( 'NONE',  ( 4.303125000614516971, -4.541064518000417216, -2.621784821875001281 ) ) ;
#27870 = DIRECTION ( 'NONE',  ( 0.000000000000000000, 0.000000000000000000, -1.000000000000000000 ) ) ;
#27871 = CARTESIAN_POINT ( 'NONE',  ( 5.062500001229035540, -4.330127018922190985, -2.500000000000001332 ) ) ;
#27872 = CARTESIAN_POINT ( 'NONE',  ( 19.00312500061451715, 0.000000000000000000, 5.243569643749999010 ) ) ;
#27873 = CARTESIAN_POINT ( 'NONE',  ( 7.537500001229033408, 4.330127018922191873, 2.499999999999999556 ) ) ;
#27874 = CARTESIAN_POINT ( 'NONE',  ( 18.17812500061451786, -4.541064518000419881, 2.621784821874995952 ) ) ;
#27875 = CARTESIAN_POINT ( 'NONE',  ( 15.47812500061451679, -4.541064518000419881, 2.621784821874995952 ) ) ;
#27876 = CARTESIAN_POINT ( 'NONE',  ( 26.29687500061451644, -2.746126346562646425, 4.756430356249996549 ) ) ;
#27877 = CARTESIAN_POINT ( 'NONE',  ( 15.67500000000000071, -4.330127018922194537, 2.499999999999995559 ) ) ;
#27878 = CARTESIAN_POINT ( 'NONE',  ( 9.412500001229034297, 0.000000000000000000, 4.999999999999998224 ) ) ;
#27879 = CARTESIAN_POINT ( 'NONE',  ( 4.490625000614516971, 6.054752690667223547, 3.707466751127219781E-16 ) ) ;
#27880 = CARTESIAN_POINT ( 'NONE',  ( 20.73750000122903359, -4.330127018922194537, 2.499999999999995559 ) ) ;
#27881 = CARTESIAN_POINT ( 'NONE',  ( 28.04999999999999716, 4.330127018922192761, -2.499999999999997780 ) ) ;
#27882 = CARTESIAN_POINT ( 'NONE',  ( 4.243569643749999010, 11.57187500061451679, -32.45002607614398471 ) ) ;
#27883 = CARTESIAN_POINT ( 'NONE',  ( 3.187500001229033764, -4.330127018922194537, 2.499999999999995559 ) ) ;
#27884 = CARTESIAN_POINT ( 'NONE',  ( 4.171875000614517326, 3.027376345333611329, 5.243569643749999010 ) ) ;
#27885 = CARTESIAN_POINT ( 'NONE',  ( 21.53437500061451715, 6.421520780324663323E-16, -5.243569643749999010 ) ) ;
#27886 =( BOUNDED_CURVE ( )  B_SPLINE_CURVE ( 2, ( #47709, #31457, #43282, #36991, #8191, #70248, #64702 ),
 .UNSPECIFIED., .F., .F. ) 
 B_SPLINE_CURVE_WITH_KNOTS ( ( 3, 2, 2, 3 ),
 ( 0.6800000000000001599, 0.6833333333333334592, 0.6866666666666667584, 0.6900000000000000577 ),
 .UNSPECIFIED. ) 
 CURVE ( )  GEOMETRIC_REPRESENTATION_ITEM ( )  RATIONAL_B_SPLINE_CURVE ( ( 0.9999999999999955591, 0.8660254037844431485, 1.000000000000000000, 0.8660254037844387076, 1.000000000000000000, 0.8660254037844342667, 1.000000000000004441 ) ) 
 REPRESENTATION_ITEM ( '' )  );
#27887 = CARTESIAN_POINT ( 'NONE',  ( 8.737500000000002487, 5.773502691896255534, 3.535250795749688401E-16 ) ) ;
#27888 = CARTESIAN_POINT ( 'NONE',  ( 15.32812500061451644, 4.541064518000418104, 2.621784821874999949 ) ) ;
#27889 = CARTESIAN_POINT ( 'NONE',  ( 10.66875000122903216, 2.886751345948126879, 4.999999999999999112 ) ) ;
#27890 = CARTESIAN_POINT ( 'NONE',  ( -2.000000000000001776, 14.59999999999999964, 33.46410161513775705 ) ) ;
#27891 = CARTESIAN_POINT ( 'NONE',  ( 29.10937500061451644, -4.541064518000417216, -2.621784821875001281 ) ) ;
#27892 = CARTESIAN_POINT ( 'NONE',  ( 21.34687500061451715, -4.119189519843965641, -2.378215178125001383 ) ) ;
#27893 = CARTESIAN_POINT ( 'NONE',  ( 11.87812500061451537, -4.541064518000419881, 2.621784821874995952 ) ) ;
#27894 = CARTESIAN_POINT ( 'NONE',  ( 11.14687500061451608, -3.027376345333610441, -5.243569643749999898 ) ) ;
#27895 = ORIENTED_EDGE ( 'NONE', *, *, #20120, .F. ) ;
#27896 = CARTESIAN_POINT ( 'NONE',  ( 28.75312500061451715, 4.541064518000418104, -2.621784821874998173 ) ) ;
#27897 = CARTESIAN_POINT ( 'NONE',  ( 23.16562500061451502, -6.054752690667223547, -1.112240025338166033E-15 ) ) ;
#27898 = CYLINDRICAL_SURFACE ( 'NONE', #1500, 5.999999999999998224 ) ;
#27899 = LINE ( 'NONE', #51870, #10096 ) ;
#27900 = CARTESIAN_POINT ( 'NONE',  ( 11.47499999999999964, 4.330127018922191873, 2.499999999999999556 ) ) ;
#27901 = CARTESIAN_POINT ( 'NONE',  ( 21.26250000122903572, -4.330127018922190985, -2.500000000000001332 ) ) ;
#27902 = CARTESIAN_POINT ( 'NONE',  ( 16.79062500061451857, -3.027376345333614438, 5.243569643749998122 ) ) ;
#27903 = CARTESIAN_POINT ( 'NONE',  ( 13.88437500061451502, 5.492252693125287522, 3.363034840372157021E-16 ) ) ;
#27904 = ORIENTED_EDGE ( 'NONE', *, *, #38380, .T. ) ;
#27905 = CARTESIAN_POINT ( 'NONE',  ( 20.85000000000000142, 4.330127018922192761, -2.499999999999997780 ) ) ;
#27906 = EDGE_CURVE ( 'NONE', #27013, #65422, #2257, .T. ) ;
#27907 = CARTESIAN_POINT ( 'NONE',  ( 23.92499999999999716, 6.123233995736764310E-16, -4.999999999999998224 ) ) ;
#27908 = CARTESIAN_POINT ( 'NONE',  ( 20.74687500061451573, 6.054752690667223547, 3.707466751127219781E-16 ) ) ;
#27909 = CARTESIAN_POINT ( 'NONE',  ( 26.54062500061451146, 6.054752690667223547, 3.707466751127219781E-16 ) ) ;
#27910 = VERTEX_POINT ( 'NONE', #50532 ) ;
#27911 = CARTESIAN_POINT ( 'NONE',  ( 4.000000000000000000, 17.93750000000000355, -27.69059892324149885 ) ) ;
#27912 = CARTESIAN_POINT ( 'NONE',  ( 9.215625000614515727, -6.054752690667223547, -1.112240025338166033E-15 ) ) ;
#27913 = CARTESIAN_POINT ( 'NONE',  ( 16.42500000000000071, 4.330127018922191873, 2.499999999999999556 ) ) ;
#27914 = CARTESIAN_POINT ( 'NONE',  ( 7.687500001229033764, -4.330127018922194537, 2.499999999999995559 ) ) ;
#27915 = CARTESIAN_POINT ( 'NONE',  ( 4.584375000614516971, 4.541064518000418104, 2.621784821874999949 ) ) ;
#27916 = CARTESIAN_POINT ( 'NONE',  ( 29.70937500061451431, 4.541064518000418104, -2.621784821874998173 ) ) ;
#27917 = VERTEX_POINT ( 'NONE', #33521 ) ;
#27918 = CARTESIAN_POINT ( 'NONE',  ( 24.14062500061451289, -3.027376345333610441, -5.243569643749999898 ) ) ;
#27919 = CARTESIAN_POINT ( 'NONE',  ( 25.73437500061451644, 4.541064518000418104, 2.621784821874999949 ) ) ;
#27920 = CARTESIAN_POINT ( 'NONE',  ( 4.243569643749999010, 19.16562500061459318, -32.45002607614398471 ) ) ;
#27921 = CARTESIAN_POINT ( 'NONE',  ( 11.02500000000000036, 4.330127018922191873, 2.499999999999999556 ) ) ;
#27922 = CARTESIAN_POINT ( 'NONE',  ( 8.203125000614518214, 0.000000000000000000, 5.243569643749999010 ) ) ;
#27923 = CARTESIAN_POINT ( 'NONE',  ( 6.112500000000001599, 2.886751345948126879, 4.999999999999998224 ) ) ;
#27924 = CARTESIAN_POINT ( 'NONE',  ( 19.42499999999999716, 6.123233995736764310E-16, -4.999999999999998224 ) ) ;
#27925 = CARTESIAN_POINT ( 'NONE',  ( 25.64062500061451644, 6.054752690667223547, 3.707466751127219781E-16 ) ) ;
#27926 = CARTESIAN_POINT ( 'NONE',  ( 12.71250000122903145, -4.330127018922190985, -2.500000000000001332 ) ) ;
#27927 = CARTESIAN_POINT ( 'NONE',  ( 14.63437500061451679, -4.119189519843968306, 2.378215178124996054 ) ) ;
#27928 = CARTESIAN_POINT ( 'NONE',  ( 3.478125000614517237, 6.421520780324663323E-16, -5.243569643749999010 ) ) ;
#27929 = CARTESIAN_POINT ( 'NONE',  ( 20.07187500061451857, -6.054752690667223547, -1.112240025338166033E-15 ) ) ;
#27930 = CARTESIAN_POINT ( 'NONE',  ( -2.121784821874996840, 15.43437500061451928, 33.67503911421598417 ) ) ;
#27931 = CARTESIAN_POINT ( 'NONE',  ( 21.98437500061451644, 6.421520780324663323E-16, -5.243569643749999010 ) ) ;
#27932 = CARTESIAN_POINT ( 'NONE',  ( 3.412500000000002309, 2.886751345948126879, 4.999999999999999112 ) ) ;
#27933 = CARTESIAN_POINT ( 'NONE',  ( 2.121784821875001281, 19.55937500061451573, 33.67503911421598417 ) ) ;
#27934 = CARTESIAN_POINT ( 'NONE',  ( 10.41562500061451679, 3.027376345333611329, 5.243569643749999010 ) ) ;
#27935 = LINE ( 'NONE', #11665, #30074 ) ;
#27936 = CARTESIAN_POINT ( 'NONE',  ( 6.084375000614518747, -4.541064518000419881, 2.621784821874995952 ) ) ;
#27937 = CYLINDRICAL_SURFACE ( 'NONE', #37184, 4.999999999999998224 ) ;
#27938 = CARTESIAN_POINT ( 'NONE',  ( 7.078125000614516438, 6.421520780324663323E-16, -5.243569643749999010 ) ) ;
#27939 = CARTESIAN_POINT ( 'NONE',  ( 12.68437500061451573, 4.541064518000418104, 2.621784821874999949 ) ) ;
#27940 =( NAMED_UNIT ( * ) SI_UNIT ( $, .STERADIAN. ) SOLID_ANGLE_UNIT ( ) );
#27941 = CARTESIAN_POINT ( 'NONE',  ( 19.98750000122903359, 6.123233995736764310E-16, -4.999999999999998224 ) ) ;
#27942 = CARTESIAN_POINT ( 'NONE',  ( 8.596875000614518925, 6.054752690667223547, 3.707466751127219781E-16 ) ) ;
#27943 = CARTESIAN_POINT ( 'NONE',  ( 9.365625000614519635, 3.027376345333613106, -5.243569643749998122 ) ) ;
#27944 = DIRECTION ( 'NONE',  ( 0.000000000000000000, 0.000000000000000000, -1.000000000000000000 ) ) ;
#27945 = CARTESIAN_POINT ( 'NONE',  ( 26.19375000122903785, -2.886751345948125991, -5.000000000000000000 ) ) ;
#27946 = CARTESIAN_POINT ( 'NONE',  ( 18.42187500061451644, 3.027376345333613106, -5.243569643749998122 ) ) ;
#27947 = CARTESIAN_POINT ( 'NONE',  ( 4.442661813835188767, 2.294285635476659646, 4.469955633307156617 ) ) ;
#27948 = CARTESIAN_POINT ( 'NONE',  ( 27.47812500061451502, 4.541064518000418104, 2.621784821874999949 ) ) ;
#27950 = CARTESIAN_POINT ( 'NONE',  ( 11.12812500061451715, 6.421520780324663323E-16, -5.243569643749999010 ) ) ;
#27949 =( BOUNDED_CURVE ( )  B_SPLINE_CURVE ( 2, ( #64033, #35599, #58848, #52957, #47058, #40799, #12340, #57404, #35240 ),
 .UNSPECIFIED., .F., .F. ) 
 B_SPLINE_CURVE_WITH_KNOTS ( ( 3, 2, 2, 2, 3 ),
 ( 0.9456521739130434590, 0.9492753623188405765, 0.9565217391304348116, 0.9637681159420289356, 0.9662083058201528241 ),
 .UNSPECIFIED. ) 
 CURVE ( )  GEOMETRIC_REPRESENTATION_ITEM ( )  RATIONAL_B_SPLINE_CURVE ( ( 0.9330127018922194093, 0.9330127018922194093, 1.000000000000000000, 0.8660254037844387076, 1.000000000000000000, 0.8660254037844387076, 1.000000000000000000, 0.9548845634016894790, 0.9401540307620559478 ) ) 
 REPRESENTATION_ITEM ( '' )  );
#27951 = EDGE_CURVE ( 'NONE', #22963, #51457, #27307, .T. ) ;
#27952 = CARTESIAN_POINT ( 'NONE',  ( 29.82187500061451502, 3.027376345333611329, 5.243569643749999010 ) ) ;
#27953 = CARTESIAN_POINT ( 'NONE',  ( -2.121784821874999949, 13.03437500061451715, -33.67503911421598417 ) ) ;
#27954 = CARTESIAN_POINT ( 'NONE',  ( 12.33750000122903145, 6.123233995736764310E-16, -4.999999999999998224 ) ) ;
#27955 = CARTESIAN_POINT ( 'NONE',  ( 27.59062500061451573, -3.027376345333614438, 5.243569643749998122 ) ) ;
#27956 = CARTESIAN_POINT ( 'NONE',  ( 2.121784821875001281, 16.35312500061451857, -26.32496088578401938 ) ) ;
#27957 = CARTESIAN_POINT ( 'NONE',  ( 15.30000000122903359, -2.886751345948129988, 4.999999999999997335 ) ) ;
#27958 = CARTESIAN_POINT ( 'NONE',  ( 13.08750000000000036, -2.886751345948125991, -5.000000000000000000 ) ) ;
#27959 = AXIS2_PLACEMENT_3D ( 'NONE', #8822, #65331, #43182 ) ;
#27960 = CARTESIAN_POINT ( 'NONE',  ( 22.67812500061451431, -4.541064518000419881, 2.621784821874995952 ) ) ;
#27961 = CARTESIAN_POINT ( 'NONE',  ( 6.684375000614518392, 6.421520780324663323E-16, -5.243569643749999010 ) ) ;
#27962 = EDGE_CURVE ( 'NONE', #65794, #15563, #44787, .T. ) ;
#27963 = CARTESIAN_POINT ( 'NONE',  ( 8.437500001229034652, 4.330127018922191873, 2.499999999999999556 ) ) ;
#27964 = CARTESIAN_POINT ( 'NONE',  ( 16.61250000122903359, 0.000000000000000000, 4.999999999999998224 ) ) ;
#27965 = CARTESIAN_POINT ( 'NONE',  ( 13.86562500061451431, 3.027376345333613106, -5.243569643749998122 ) ) ;
#27966 = CARTESIAN_POINT ( 'NONE',  ( 17.39062500061451644, -3.027376345333610441, -5.243569643749999898 ) ) ;
#27967 = CARTESIAN_POINT ( 'NONE',  ( 26.43750000122903288, 4.330127018922191873, 2.499999999999999556 ) ) ;
#27968 =( BOUNDED_CURVE ( )  B_SPLINE_CURVE ( 3, ( #53932, #20656, #3691, #32121 ),
 .UNSPECIFIED., .F., .T. ) 
 B_SPLINE_CURVE_WITH_KNOTS ( ( 4, 4 ),
 ( 4.133880465060611797, 4.712388980384689674 ),
 .UNSPECIFIED. ) 
 CURVE ( )  GEOMETRIC_REPRESENTATION_ITEM ( )  RATIONAL_B_SPLINE_CURVE ( ( 1.000000000000000000, 0.9723045704793149557, 0.9723045704793149557, 1.000000000000000000 ) ) 
 REPRESENTATION_ITEM ( '' )  );
#27969 = CARTESIAN_POINT ( 'NONE',  ( 29.10000000122903074, 5.773502691896255534, 3.535250795749688894E-16 ) ) ;
#27970 = CARTESIAN_POINT ( 'NONE',  ( 23.40000000000000213, -4.330127018922190985, -2.500000000000001332 ) ) ;
#27971 = CARTESIAN_POINT ( 'NONE',  ( 25.69687500061451502, 6.054752690667223547, 3.707466751127219781E-16 ) ) ;
#27972 = DIRECTION ( 'NONE',  ( 0.000000000000000000, 0.000000000000000000, 1.000000000000000000 ) ) ;
#27973 = CARTESIAN_POINT ( 'NONE',  ( 9.675000001229035362, 2.886751345948129099, -4.999999999999998224 ) ) ;
#27974 = CARTESIAN_POINT ( 'NONE',  ( 26.93437500061451573, 6.421520780324663323E-16, -5.243569643749999010 ) ) ;
#27975 = CARTESIAN_POINT ( 'NONE',  ( 24.48749999999999716, 5.773502691896255534, 3.535250795749688401E-16 ) ) ;
#27976 = CARTESIAN_POINT ( 'NONE',  ( 5.784375000614517148, 6.421520780324663323E-16, -5.243569643749999010 ) ) ;
#27977 = CARTESIAN_POINT ( 'NONE',  ( 24.02812500061451573, -4.541064518000419881, 2.621784821874995952 ) ) ;
#27978 =( BOUNDED_CURVE ( )  B_SPLINE_CURVE ( 2, ( #10795, #55142, #10435, #55502, #4175, #4898, #33330 ),
 .UNSPECIFIED., .F., .F. ) 
 B_SPLINE_CURVE_WITH_KNOTS ( ( 3, 2, 2, 3 ),
 ( 0.2499999999999999722, 0.2533333333333333548, 0.2566666666666667096, 0.2600000000000000644 ),
 .UNSPECIFIED. ) 
 CURVE ( )  GEOMETRIC_REPRESENTATION_ITEM ( )  RATIONAL_B_SPLINE_CURVE ( ( 1.000000000000001110, 0.8660254037844374864, 1.000000000000000000, 0.8660254037844387076, 1.000000000000000000, 0.8660254037844364872, 1.000000000000002220 ) ) 
 REPRESENTATION_ITEM ( '' )  );
#27979 = CARTESIAN_POINT ( 'NONE',  ( 3.756430356250000102, 14.10312499938548392, 30.00000000000000000 ) ) ;
#27980 = CARTESIAN_POINT ( 'NONE',  ( -4.000000000000000000, 15.36874999877096570, 30.00000000000000000 ) ) ;
#27981 = CARTESIAN_POINT ( 'NONE',  ( 11.37187500061451750, 3.027376345333611329, 5.243569643749999010 ) ) ;
#27982 = CARTESIAN_POINT ( 'NONE',  ( 4.453125000614517326, 4.541064518000418104, -2.621784821874998173 ) ) ;
#27983 = CARTESIAN_POINT ( 'NONE',  ( 3.984375000614517326, 6.421520780324663323E-16, -5.243569643749999010 ) ) ;
#27984 = CARTESIAN_POINT ( 'NONE',  ( 5.784375000614517148, 6.421520780324663323E-16, -5.243569643749999010 ) ) ;
#27985 = CARTESIAN_POINT ( 'NONE',  ( 29.07187500061451502, -6.054752690667223547, -1.112240025338166033E-15 ) ) ;
#27986 = CARTESIAN_POINT ( 'NONE',  ( 4.243569643749999898, 10.99062500061459424, 32.45002607614398471 ) ) ;
#27987 = CARTESIAN_POINT ( 'NONE',  ( 20.10000000000000142, 0.000000000000000000, 4.999999999999998224 ) ) ;
#27988 = ORIENTED_EDGE ( 'NONE', *, *, #57093, .F. ) ;
#27989 = CARTESIAN_POINT ( 'NONE',  ( 26.17500000000000071, 6.123233995736764310E-16, -4.999999999999998224 ) ) ;
#27990 = ADVANCED_FACE ( 'NONE', ( #11001 ), #26913, .F. ) ;
#27991 = CARTESIAN_POINT ( 'NONE',  ( 28.80937500061451573, 4.541064518000418104, -2.621784821874998173 ) ) ;
#27992 = ORIENTED_EDGE ( 'NONE', *, *, #11628, .F. ) ;
#27993 = CARTESIAN_POINT ( 'NONE',  ( 18.74062500061451431, -3.027376345333610441, -5.243569643749999898 ) ) ;
#27994 = CARTESIAN_POINT ( 'NONE',  ( 7.453125000614516438, -4.541064518000417216, -2.621784821875001281 ) ) ;
#27995 = CARTESIAN_POINT ( 'NONE',  ( 21.08437500061451786, 5.492252693125287522, 3.363034840372157021E-16 ) ) ;
#27996 = CARTESIAN_POINT ( 'NONE',  ( 3.646875000614520079, 6.054752690667223547, 3.707466751127219781E-16 ) ) ;
#27997 = CARTESIAN_POINT ( 'NONE',  ( 18.26250000122903216, 4.330127018922192761, -2.499999999999997780 ) ) ;
#27998 = CARTESIAN_POINT ( 'NONE',  ( 24.18750000000000355, -2.886751345948129988, 4.999999999999997335 ) ) ;
#27999 = CARTESIAN_POINT ( 'NONE',  ( 16.05000000000000071, 0.000000000000000000, 4.999999999999998224 ) ) ;
#28000 = CARTESIAN_POINT ( 'NONE',  ( 8.146875000614516082, 6.054752690667223547, 3.707466751127219781E-16 ) ) ;
#28001 = CARTESIAN_POINT ( 'NONE',  ( 10.84687500061451892, 6.054752690667223547, 3.707466751127219781E-16 ) ) ;
#28002 = CARTESIAN_POINT ( 'NONE',  ( 21.79687500061451644, -3.027376345333614438, 5.243569643749998122 ) ) ;
#28003 = CARTESIAN_POINT ( 'NONE',  ( 45.00000000000000000, 0.000000000000000000, 0.000000000000000000 ) ) ;
#28004 = ORIENTED_EDGE ( 'NONE', *, *, #53941, .F. ) ;
#28005 = CARTESIAN_POINT ( 'NONE',  ( 3.384375000614517237, -4.541064518000419881, 2.621784821874995952 ) ) ;
#28006 = CARTESIAN_POINT ( 'NONE',  ( 10.42500000000000071, 6.123233995736764310E-16, -4.999999999999998224 ) ) ;
#28007 = CARTESIAN_POINT ( 'NONE',  ( 7.246875000614518392, 6.054752690667223547, 3.707466751127219781E-16 ) ) ;
#28008 = AXIS2_PLACEMENT_3D ( 'NONE', #52725, #69368, #6938 ) ;
#28009 = CARTESIAN_POINT ( 'NONE',  ( 21.18749999999999645, -2.886751345948125991, -5.000000000000000000 ) ) ;
#28010 = CARTESIAN_POINT ( 'NONE',  ( 17.16562500061451502, 3.027376345333611329, 5.243569643749999010 ) ) ;
#28011 = CARTESIAN_POINT ( 'NONE',  ( -2.000000000000001776, 18.19999999999999929, 33.46410161513775705 ) ) ;
#28012 = CARTESIAN_POINT ( 'NONE',  ( 22.34999999999999787, 0.000000000000000000, 4.999999999999998224 ) ) ;
#28013 = CARTESIAN_POINT ( 'NONE',  ( 23.10937500061451644, 0.000000000000000000, 4.756430356249998326 ) ) ;
#28014 = CARTESIAN_POINT ( 'NONE',  ( 9.028125000614517504, 4.541064518000418104, 2.621784821874999949 ) ) ;
#28015 = CARTESIAN_POINT ( 'NONE',  ( 26.59687500061451360, 6.054752690667223547, 3.707466751127219781E-16 ) ) ;
#28016 = DIRECTION ( 'NONE',  ( -1.000000000000000000, -0.000000000000000000, -0.000000000000000000 ) ) ;
#28017 = CARTESIAN_POINT ( 'NONE',  ( 28.69687500061451502, -3.027376345333610441, -5.243569643749999898 ) ) ;
#28018 = CARTESIAN_POINT ( 'NONE',  ( 9.150000000000002132, 4.330127018922192761, -2.499999999999997780 ) ) ;
#28019 = CARTESIAN_POINT ( 'NONE',  ( -2.828200636599751609E-16, 15.05000000122903536, 25.38119784648299770 ) ) ;
#28020 = CARTESIAN_POINT ( 'NONE',  ( 9.525000001229033231, -5.773502691896255534, -1.060575238724906372E-15 ) ) ;
#28021 = CARTESIAN_POINT ( 'NONE',  ( 19.92187500061451644, 3.027376345333611329, 5.243569643749999010 ) ) ;
#28022 = CARTESIAN_POINT ( 'NONE',  ( 13.50937500061451679, 4.541064518000418104, -2.621784821874998173 ) ) ;
#28023 = CARTESIAN_POINT ( 'NONE',  ( 0.000000000000000000, 20.00000000000000000, -30.00000000000000000 ) ) ;
#28024 = ORIENTED_EDGE ( 'NONE', *, *, #55282, .T. ) ;
#28025 = CARTESIAN_POINT ( 'NONE',  ( 13.90312500061451750, 4.541064518000418104, -2.621784821874998173 ) ) ;
#28026 = CARTESIAN_POINT ( 'NONE',  ( 25.91250000122903074, 4.330127018922192761, -2.499999999999997780 ) ) ;
#28027 = CARTESIAN_POINT ( 'NONE',  ( 14.03437500061451715, 4.541064518000418104, 2.621784821874999949 ) ) ;
#28028 = CARTESIAN_POINT ( 'NONE',  ( 1.968632615237262629, 9.806224642577898720, -24.32863725417373857 ) ) ;
#28029 = CARTESIAN_POINT ( 'NONE',  ( 18.21562500061451573, -6.054752690667223547, -1.112240025338166033E-15 ) ) ;
#28030 = DIRECTION ( 'NONE',  ( -1.000000000000000000, -0.000000000000000000, -0.000000000000000000 ) ) ;
#28031 = CARTESIAN_POINT ( 'NONE',  ( 26.67187500061451644, 3.027376345333611329, 5.243569643749999010 ) ) ;
#28032 = CARTESIAN_POINT ( 'NONE',  ( -3.000416591977282496E-16, 11.59062500061451750, 25.09994784771203058 ) ) ;
#28033 = CARTESIAN_POINT ( 'NONE',  ( 15.87187500061451573, 3.027376345333611329, 5.243569643749999010 ) ) ;
#28034 = CARTESIAN_POINT ( 'NONE',  ( 14.85000000122903252, -2.886751345948129988, 4.999999999999997335 ) ) ;
#28035 = CARTESIAN_POINT ( 'NONE',  ( 8.484375000614518214, 5.824947211148865298E-16, -4.756430356249998326 ) ) ;
#28036 = CARTESIAN_POINT ( 'NONE',  ( 3.336147517545859920, -3.724270626431634312, 3.691191611388044524 ) ) ;
#28037 = CARTESIAN_POINT ( 'NONE',  ( 21.00937500061451857, -4.541064518000417216, -2.621784821875001281 ) ) ;
#28038 = CARTESIAN_POINT ( 'NONE',  ( 20.43750000122903643, 6.123233995736764310E-16, -4.999999999999998224 ) ) ;
#28039 = CARTESIAN_POINT ( 'NONE',  ( 14.44687500061451679, 6.054752690667223547, 3.707466751127219781E-16 ) ) ;
#28040 = CARTESIAN_POINT ( 'NONE',  ( 2.121784821874999061, 12.05937500061451750, 26.32496088578401583 ) ) ;
#28041 = CARTESIAN_POINT ( 'NONE',  ( 22.16250000122903074, -4.330127018922190985, -2.500000000000001332 ) ) ;
#28042 = CARTESIAN_POINT ( 'NONE',  ( 16.37812500061451715, -4.541064518000419881, 2.621784821874995952 ) ) ;
#28043 = ORIENTED_EDGE ( 'NONE', *, *, #25975, .F. ) ;
#28044 = ORIENTED_EDGE ( 'NONE', *, *, #13788, .F. ) ;
#28045 = CARTESIAN_POINT ( 'NONE',  ( 19.42499999999999716, 6.123233995736764310E-16, -4.999999999999998224 ) ) ;
#28046 = CARTESIAN_POINT ( 'NONE',  ( -4.243569643749999898, 19.85937500061451644, -30.00000000000000000 ) ) ;
#28047 = CARTESIAN_POINT ( 'NONE',  ( 25.37812500061451715, -4.541064518000419881, 2.621784821874995952 ) ) ;
#28048 = CARTESIAN_POINT ( 'NONE',  ( 1.838027276006278798, 4.657088507379086195, 33.56272475032025682 ) ) ;
#28049 = EDGE_CURVE ( 'NONE', #48298, #69560, #64604, .T. ) ;
#28050 = CARTESIAN_POINT ( 'NONE',  ( 16.38750000122903216, 6.123233995736764310E-16, -4.999999999999998224 ) ) ;
#28051 = CARTESIAN_POINT ( 'NONE',  ( 22.75312500061451360, -4.541064518000417216, -2.621784821875001281 ) ) ;
#28052 = CARTESIAN_POINT ( 'NONE',  ( 24.55312500061451786, -4.541064518000417216, -2.621784821875001281 ) ) ;
#28053 = CARTESIAN_POINT ( 'NONE',  ( 4.865625000614517859, 3.027376345333613106, -5.243569643749998122 ) ) ;
#28054 = ORIENTED_EDGE ( 'NONE', *, *, #60470, .T. ) ;
#28055 = CARTESIAN_POINT ( 'NONE',  ( 29.17500000000000071, -4.330127018922194537, 2.499999999999995559 ) ) ;
#28056 = CARTESIAN_POINT ( 'NONE',  ( 3.628125000614518036, 4.541064518000418104, 2.621784821874999949 ) ) ;
#28057 = CARTESIAN_POINT ( 'NONE',  ( 12.23437500061451821, 4.119189519843966529, 2.378215178124999607 ) ) ;
#28058 = DIRECTION ( 'NONE',  ( -0.000000000000000000, -1.000000000000000000, -0.000000000000000000 ) ) ;
#28059 = CARTESIAN_POINT ( 'NONE',  ( -2.828200636599751609E-16, 11.00000000122903288, -34.61880215351700230 ) ) ;
#28060 = CARTESIAN_POINT ( 'NONE',  ( 2.121784821875001281, 17.75937500061451502, -26.32496088578401938 ) ) ;
#28061 = CARTESIAN_POINT ( 'NONE',  ( 7.575000000000001954, -4.330127018922194537, 2.499999999999995559 ) ) ;
#28062 = CARTESIAN_POINT ( 'NONE',  ( 5.025000001229035895, -5.773502691896255534, -1.060575238724906372E-15 ) ) ;
#28063 = CARTESIAN_POINT ( 'NONE',  ( 12.34687500061452070, -3.027376345333614438, 5.243569643749998122 ) ) ;
#28064 = CARTESIAN_POINT ( 'NONE',  ( 34.99999999999999289, -9.000000000000000000, 0.000000000000000000 ) ) ;
#28065 = CARTESIAN_POINT ( 'NONE',  ( 4.434375000614519280, 6.421520780324663323E-16, -5.243569643749999010 ) ) ;
#28066 = LINE ( 'NONE', #5164, #40877 ) ;
#28067 = CARTESIAN_POINT ( 'NONE',  ( 12.54375000122903572, -2.886751345948130876, 4.999999999999996447 ) ) ;
#28068 = CARTESIAN_POINT ( 'NONE',  ( 10.05937500061451750, 0.000000000000000000, 5.243569643749999010 ) ) ;
#28069 = CARTESIAN_POINT ( 'NONE',  ( 1.999999999999998668, 17.26250000122903572, -33.46410161513775705 ) ) ;
#28070 = CARTESIAN_POINT ( 'NONE',  ( 19.82812500061451644, 4.541064518000418104, 2.621784821874999949 ) ) ;
#28071 = CARTESIAN_POINT ( 'NONE',  ( 16.64999999999999858, -4.330127018922190985, -2.500000000000001332 ) ) ;
#28072 = CARTESIAN_POINT ( 'NONE',  ( -4.243569643749999898, 18.00312500061459176, 30.00000000000000000 ) ) ;
#28073 = CARTESIAN_POINT ( 'NONE',  ( 22.92187500061451644, 3.027376345333613106, -5.243569643749998122 ) ) ;
#28074 = DIRECTION ( 'NONE',  ( 0.000000000000000000, 0.000000000000000000, 1.000000000000000000 ) ) ;
#28075 = EDGE_CURVE ( 'NONE', #35566, #2080, #42400, .T. ) ;
#28076 = CARTESIAN_POINT ( 'NONE',  ( 28.42500000122904069, -5.773502691896255534, -1.060575238724906372E-15 ) ) ;
#28077 = CARTESIAN_POINT ( 'NONE',  ( 20.22187500061451715, 4.119189519843966529, 2.378215178124999607 ) ) ;
#28078 = CARTESIAN_POINT ( 'NONE',  ( 24.55312500061451786, -4.541064518000417216, -2.621784821875001281 ) ) ;
#28079 = CARTESIAN_POINT ( 'NONE',  ( 15.02812500061451750, -4.541064518000419881, 2.621784821874995952 ) ) ;
#28080 = CARTESIAN_POINT ( 'NONE',  ( 14.64375000122903181, 5.773502691896255534, 3.535250795749688894E-16 ) ) ;
#28081 = CARTESIAN_POINT ( 'NONE',  ( 10.84687500061451892, 6.054752690667223547, 3.707466751127219781E-16 ) ) ;
#28082 = CARTESIAN_POINT ( 'NONE',  ( 28.61249999999999716, 2.886751345948126879, 4.999999999999999112 ) ) ;
#28083 = CARTESIAN_POINT ( 'NONE',  ( 23.77500000122903145, 2.886751345948126879, 4.999999999999999112 ) ) ;
#28084 = CARTESIAN_POINT ( 'NONE',  ( 4.696875000614518569, -3.027376345333614438, 5.243569643749998122 ) ) ;
#28085 = CARTESIAN_POINT ( 'NONE',  ( 14.29687500061451821, -3.027376345333610441, -5.243569643749999898 ) ) ;
#28086 = CARTESIAN_POINT ( 'NONE',  ( 28.77187500061451431, 3.027376345333613106, -5.243569643749998122 ) ) ;
#28087 = CARTESIAN_POINT ( 'NONE',  ( 3.160880256176461511, -3.874123901750303300, -3.160880256176591185 ) ) ;
#28088 = CARTESIAN_POINT ( 'NONE',  ( 15.84375000122903643, -2.886751345948237457, -4.999999999999807265 ) ) ;
#28089 = CARTESIAN_POINT ( 'NONE',  ( 24.60937500061451644, -4.541064518000417216, -2.621784821875001281 ) ) ;
#28090 = CARTESIAN_POINT ( 'NONE',  ( 15.08437500061451786, -4.541064518000419881, 2.621784821874995952 ) ) ;
#28091 = CARTESIAN_POINT ( 'NONE',  ( 1.878215178125000495, 15.97812499938548392, 26.74683588394047007 ) ) ;
#28092 = CARTESIAN_POINT ( 'NONE',  ( 28.35000000000000142, -4.330127018922190985, -2.500000000000001332 ) ) ;
#28093 = CARTESIAN_POINT ( 'NONE',  ( 3.037500001229032964, 4.330127018922191873, 2.499999999999999556 ) ) ;
#28094 = CARTESIAN_POINT ( 'NONE',  ( 7.921875000614517326, 5.824947211148865298E-16, -4.756430356249998326 ) ) ;
#28095 = CARTESIAN_POINT ( 'NONE',  ( 16.79062500061451857, -3.027376345333614438, 5.243569643749998122 ) ) ;
#28096 = CARTESIAN_POINT ( 'NONE',  ( 8.324999999999999289, 4.330127018922191873, 2.499999999999999556 ) ) ;
#28097 = CARTESIAN_POINT ( 'NONE',  ( 0.000000000000000000, 27.50000000000000000, 26.00000000000000000 ) ) ;
#28098 = CARTESIAN_POINT ( 'NONE',  ( 16.23750000000000071, -2.886751345948125991, -5.000000000000000000 ) ) ;
#28099 = CARTESIAN_POINT ( 'NONE',  ( -2.121784821874999949, 12.97812500061451679, 26.32496088578401938 ) ) ;
#28100 = DIRECTION ( 'NONE',  ( 0.000000000000000000, 0.000000000000000000, 1.000000000000000000 ) ) ;
#28101 = CARTESIAN_POINT ( 'NONE',  ( 21.11250000122903359, 0.000000000000000000, 4.999999999999998224 ) ) ;
#28102 = CARTESIAN_POINT ( 'NONE',  ( -1.071796769724488563, 10.19240381056766687, -26.00000000000000000 ) ) ;
#28103 = CARTESIAN_POINT ( 'NONE',  ( 26.63437500061451857, 4.541064518000418104, 2.621784821874999949 ) ) ;
#28104 = ORIENTED_EDGE ( 'NONE', *, *, #69060, .F. ) ;
#28105 = CARTESIAN_POINT ( 'NONE',  ( 17.05312500061451786, 4.541064518000418104, -2.621784821874998173 ) ) ;
#28106 = CARTESIAN_POINT ( 'NONE',  ( 22.30312500061451431, -4.541064518000417216, -2.621784821875001281 ) ) ;
#28107 = CARTESIAN_POINT ( 'NONE',  ( 22.02187500061452141, 3.027376345333613106, -5.243569643749998122 ) ) ;
#28108 = CARTESIAN_POINT ( 'NONE',  ( 7.575000000000001954, -4.330127018922194537, 2.499999999999995559 ) ) ;
#28109 = CARTESIAN_POINT ( 'NONE',  ( 9.103125000614515017, 0.000000000000000000, 5.243569643749999010 ) ) ;
#28110 = CARTESIAN_POINT ( 'NONE',  ( 24.29062500061451502, 6.054752690667223547, 3.707466751127219781E-16 ) ) ;
#28111 = CARTESIAN_POINT ( 'NONE',  ( 14.40937500061451715, 4.541064518000418104, -2.621784821874998173 ) ) ;
#28112 = CARTESIAN_POINT ( 'NONE',  ( 20.18437500061451573, 6.421520780324663323E-16, -5.243569643749999010 ) ) ;
#28113 = LINE ( 'NONE', #49554, #6234 ) ;
#28114 = CARTESIAN_POINT ( 'NONE',  ( 2.121784821875001281, 18.60312500061451857, 33.67503911421598417 ) ) ;
#28115 = CARTESIAN_POINT ( 'NONE',  ( 22.20000000122903216, -2.886751345948125991, -5.000000000000000000 ) ) ;
#28116 = CARTESIAN_POINT ( 'NONE',  ( 15.34687500061451892, 5.492252693125287522, 3.363034840372157021E-16 ) ) ;
#28117 = CARTESIAN_POINT ( 'NONE',  ( 11.46562500061451573, -6.054752690667223547, -1.112240025338166033E-15 ) ) ;
#28118 = CARTESIAN_POINT ( 'NONE',  ( 6.234375000614519102, 6.421520780324663323E-16, -5.243569643749999010 ) ) ;
#28119 = CARTESIAN_POINT ( 'NONE',  ( 5.934375000614517504, 4.541064518000418104, 2.621784821874999949 ) ) ;
#28120 =( BOUNDED_CURVE ( )  B_SPLINE_CURVE ( 2, ( #52843, #35124, #41401, #1890, #24757, #19200, #18112 ),
 .UNSPECIFIED., .F., .F. ) 
 B_SPLINE_CURVE_WITH_KNOTS ( ( 3, 2, 2, 3 ),
 ( 0.4333333333333333481, 0.4361111111111111160, 0.4388888888888888840, 0.4416666666666666519 ),
 .UNSPECIFIED. ) 
 CURVE ( )  GEOMETRIC_REPRESENTATION_ITEM ( )  RATIONAL_B_SPLINE_CURVE ( ( 1.000000000000000000, 0.8660254037844387076, 1.000000000000000000, 0.8660254037844387076, 1.000000000000000000, 0.8660254037844387076, 1.000000000000000000 ) ) 
 REPRESENTATION_ITEM ( '' )  );
#28121 = ORIENTED_EDGE ( 'NONE', *, *, #24238, .F. ) ;
#28122 = CARTESIAN_POINT ( 'NONE',  ( 27.04687500061451644, 6.054752690667223547, 3.707466751127219781E-16 ) ) ;
#28123 = CARTESIAN_POINT ( 'NONE',  ( 19.52812500061451573, -4.541064518000419881, 2.621784821874995952 ) ) ;
#28124 = CARTESIAN_POINT ( 'NONE',  ( 27.86250000122903359, 0.000000000000000000, 4.999999999999998224 ) ) ;
#28125 = CARTESIAN_POINT ( 'NONE',  ( 26.65312500061451573, 0.000000000000000000, 5.243569643749999010 ) ) ;
#28126 = CARTESIAN_POINT ( 'NONE',  ( 25.05937500061451573, -4.541064518000417216, -2.621784821875001281 ) ) ;
#28127 = CARTESIAN_POINT ( 'NONE',  ( 17.54062500061451502, 6.054752690667223547, 3.707466751127219781E-16 ) ) ;
#28128 = CARTESIAN_POINT ( 'NONE',  ( -4.243569643749999898, 19.40937500061451715, 30.00000000000000000 ) ) ;
#28129 = CARTESIAN_POINT ( 'NONE',  ( 24.17812500061451786, 6.421520780324663323E-16, -5.243569643749999010 ) ) ;
#28130 = CARTESIAN_POINT ( 'NONE',  ( 5.362500001229033586, 0.000000000000000000, 4.999999999999998224 ) ) ;
#28131 = ORIENTED_EDGE ( 'NONE', *, *, #59897, .F. ) ;
#28132 = CARTESIAN_POINT ( 'NONE',  ( 28.68749999999999645, -2.886751345948129988, 4.999999999999997335 ) ) ;
#28133 = CARTESIAN_POINT ( 'NONE',  ( 3.999999999999999112, 16.17500000000000071, -30.00000000000000000 ) ) ;
#28134 = CARTESIAN_POINT ( 'NONE',  ( -1.878215178125001827, 17.55312499938548498, 33.25316411605952283 ) ) ;
#28135 = CARTESIAN_POINT ( 'NONE',  ( 4.584375000614516971, 4.541064518000418104, 2.621784821874999949 ) ) ;
#28136 = CARTESIAN_POINT ( 'NONE',  ( 11.20312500061451644, 4.541064518000418104, -2.621784821874998173 ) ) ;
#28137 = CARTESIAN_POINT ( 'NONE',  ( 6.384375000614516793, 4.541064518000418104, 2.621784821874999949 ) ) ;
#28138 = CARTESIAN_POINT ( 'NONE',  ( 24.26250000122903216, 0.000000000000000000, 4.999999999999998224 ) ) ;
#28139 = CARTESIAN_POINT ( 'NONE',  ( 15.04687500061451644, -3.027376345333614438, 5.243569643749998122 ) ) ;
#28140 = CARTESIAN_POINT ( 'NONE',  ( 29.54062500061451502, -3.027376345333610441, -5.243569643749999898 ) ) ;
#28141 = CARTESIAN_POINT ( 'NONE',  ( 28.42499999999999716, 6.123233995736764310E-16, -4.999999999999998224 ) ) ;
#28142 = CARTESIAN_POINT ( 'NONE',  ( 27.42187500061451644, 3.027376345333613106, -5.243569643749998122 ) ) ;
#28143 = CYLINDRICAL_SURFACE ( 'NONE', #18437, 4.999999999999998224 ) ;
#28144 = CARTESIAN_POINT ( 'NONE',  ( 14.01562500061451644, 3.027376345333611329, 5.243569643749999010 ) ) ;
#28145 = VERTEX_POINT ( 'NONE', #72331 ) ;
#28146 = CARTESIAN_POINT ( 'NONE',  ( 8.990625000614516082, 6.054752690667223547, 3.707466751127219781E-16 ) ) ;
#28147 = CARTESIAN_POINT ( 'NONE',  ( 6.440625000614517148, -3.027376345333614438, 5.243569643749998122 ) ) ;
#28148 = CARTESIAN_POINT ( 'NONE',  ( 17.89687500061451431, -2.746126346562642428, -4.756430356249999214 ) ) ;
#28149 = FACE_OUTER_BOUND ( 'NONE', #41074, .T. ) ;
#28150 = CARTESIAN_POINT ( 'NONE',  ( 16.35000000000000142, 4.330127018922192761, -2.499999999999997780 ) ) ;
#28151 = CARTESIAN_POINT ( 'NONE',  ( 15.98437500061451821, -4.541064518000419881, 2.621784821874995952 ) ) ;
#28152 = CARTESIAN_POINT ( 'NONE',  ( 12.11250000122903181, 0.000000000000000000, 4.999999999999998224 ) ) ;
#28153 = EDGE_CURVE ( 'NONE', #17794, #69491, #50890, .T. ) ;
#28154 = CARTESIAN_POINT ( 'NONE',  ( 20.51249999999999929, 2.886751345948126879, 4.999999999999999112 ) ) ;
#28155 = CARTESIAN_POINT ( 'NONE',  ( 20.67187500061451289, 3.027376345333613106, -5.243569643749998122 ) ) ;
#28156 = CARTESIAN_POINT ( 'NONE',  ( -3.000416591977282496E-16, 15.19062500061451715, -34.90005215228797653 ) ) ;
#28157 = CARTESIAN_POINT ( 'NONE',  ( -1.071796769724496556, 16.94240381056766509, 33.99999999999998579 ) ) ;
#28158 = CARTESIAN_POINT ( 'NONE',  ( 25.62187500061451573, 4.119189519843966529, 2.378215178124999607 ) ) ;
#28159 = CARTESIAN_POINT ( 'NONE',  ( 18.35625000122903216, 0.000000000000000000, 4.999999999999998224 ) ) ;
#28160 = CARTESIAN_POINT ( 'NONE',  ( 25.97812500061451502, 6.421520780324663323E-16, -5.243569643749999010 ) ) ;
#28161 = FACE_OUTER_BOUND ( 'NONE', #11558, .T. ) ;
#28162 =( BOUNDED_CURVE ( )  B_SPLINE_CURVE ( 2, ( #71056, #30439, #52968, #3470, #2364, #8268, #48895 ),
 .UNSPECIFIED., .F., .F. ) 
 B_SPLINE_CURVE_WITH_KNOTS ( ( 3, 2, 2, 3 ),
 ( 0.7249999999999999778, 0.7277777777777777457, 0.7305555555555555136, 0.7333333333333332815 ),
 .UNSPECIFIED. ) 
 CURVE ( )  GEOMETRIC_REPRESENTATION_ITEM ( )  RATIONAL_B_SPLINE_CURVE ( ( 1.000000000000000000, 0.8660254037844387076, 1.000000000000000000, 0.8660254037844387076, 1.000000000000000000, 0.8660254037844387076, 1.000000000000000000 ) ) 
 REPRESENTATION_ITEM ( '' )  );
#28163 = CARTESIAN_POINT ( 'NONE',  ( 26.69999999999999929, 4.330127018922192761, -2.499999999999997780 ) ) ;
#28164 = EDGE_CURVE ( 'NONE', #71509, #40722, #22441, .T. ) ;
#28165 = CARTESIAN_POINT ( 'NONE',  ( 8.503125000614515372, 4.541064518000418104, -2.621784821874998173 ) ) ;
#28166 = CARTESIAN_POINT ( 'NONE',  ( 28.09687500061451715, -4.119189519843965641, -2.378215178125001383 ) ) ;
#28167 = CARTESIAN_POINT ( 'NONE',  ( 19.20937500061451786, -4.541064518000417216, -2.621784821875001281 ) ) ;
#28168 = CARTESIAN_POINT ( 'NONE',  ( 10.95937500061451608, -5.492252693125287522, -1.008910452111647106E-15 ) ) ;
#28169 = CARTESIAN_POINT ( 'NONE',  ( 4.228125000614517681, -4.541064518000419881, 2.621784821874995952 ) ) ;
#28170 = CARTESIAN_POINT ( 'NONE',  ( 10.09687500061451715, -3.027376345333614438, 5.243569643749998122 ) ) ;
#28171 = ORIENTED_EDGE ( 'NONE', *, *, #17037, .T. ) ;
#28172 = CARTESIAN_POINT ( 'NONE',  ( 20.89687500061452141, -3.027376345333614438, 5.243569643749998122 ) ) ;
#28173 = CARTESIAN_POINT ( 'NONE',  ( -1.999999999999999112, 15.74374999877096570, 26.53589838486224650 ) ) ;
#28174 = CARTESIAN_POINT ( 'NONE',  ( 29.13749999999999929, -2.886751345948129988, 4.999999999999997335 ) ) ;
#28175 = CARTESIAN_POINT ( 'NONE',  ( 5.924999999999999822, 6.123233995736764310E-16, -4.999999999999998224 ) ) ;
#28176 = CARTESIAN_POINT ( 'NONE',  ( 14.96250000122903323, -4.330127018922190985, -2.500000000000001332 ) ) ;
#28177 = DIRECTION ( 'NONE',  ( -1.000000000000000000, -0.000000000000000000, -0.000000000000000000 ) ) ;
#28178 = ORIENTED_EDGE ( 'NONE', *, *, #63321, .F. ) ;
#28179 = CARTESIAN_POINT ( 'NONE',  ( 13.79999999999999893, 0.000000000000000000, 4.999999999999998224 ) ) ;
#28180 = CARTESIAN_POINT ( 'NONE',  ( 25.86562500061451431, -6.054752690667223547, -1.112240025338166033E-15 ) ) ;
#28181 = CARTESIAN_POINT ( 'NONE',  ( 16.72500000000000142, 6.123233995736764310E-16, -4.999999999999998224 ) ) ;
#28182 = CARTESIAN_POINT ( 'NONE',  ( 10.38750000122903572, -4.330127018922194537, 2.499999999999995559 ) ) ;
#28183 = CARTESIAN_POINT ( 'NONE',  ( 8.240625000614516082, -3.027376345333614438, 5.243569643749998122 ) ) ;
#28184 = CARTESIAN_POINT ( 'NONE',  ( 8.887499999999999289, -2.886751345948129988, 4.999999999999997335 ) ) ;
#28185 = CARTESIAN_POINT ( 'NONE',  ( 30.00000000000000000, 0.000000000000000000, 0.000000000000000000 ) ) ;
#28186 = CARTESIAN_POINT ( 'NONE',  ( 4.243569643749999898, 15.09687500061451892, -27.54997392385601529 ) ) ;
#28187 = CARTESIAN_POINT ( 'NONE',  ( 27.03750000122903430, -4.330127018922194537, 2.499999999999995559 ) ) ;
#28188 = CARTESIAN_POINT ( 'NONE',  ( 3.756430356249998770, 15.30312499938548321, 32.16877607737301759 ) ) ;
#28189 = CARTESIAN_POINT ( 'NONE',  ( 7.762500000000001954, 2.886751345948129099, -4.999999999999998224 ) ) ;
#28190 = CARTESIAN_POINT ( 'NONE',  ( -3.999999999999999112, 12.80000000000000071, 30.00000000000000000 ) ) ;
#28191 = VERTEX_POINT ( 'NONE', #55706 ) ;
#28192 = CARTESIAN_POINT ( 'NONE',  ( 23.61562500061451431, -6.054752690667223547, -1.112240025338166033E-15 ) ) ;
#28193 = CARTESIAN_POINT ( 'NONE',  ( 12.78750000122903430, 6.123233995736764310E-16, -4.999999999999998224 ) ) ;
#28194 = CARTESIAN_POINT ( 'NONE',  ( 28.60312500061451502, -4.541064518000417216, -2.621784821875001281 ) ) ;
#28195 = CARTESIAN_POINT ( 'NONE',  ( 29.82187500061451502, 3.027376345333611329, 5.243569643749999010 ) ) ;
#28196 = CARTESIAN_POINT ( 'NONE',  ( 19.28437500061451360, 6.421520780324663323E-16, -5.243569643749999010 ) ) ;
#28197 = CARTESIAN_POINT ( 'NONE',  ( 17.46562500061451217, 3.027376345333613106, -5.243569643749998122 ) ) ;
#28198 = CARTESIAN_POINT ( 'NONE',  ( -2.121784821874996840, 10.42812500061459424, -26.32496088578401583 ) ) ;
#28199 = CARTESIAN_POINT ( 'NONE',  ( 6.590625000614518392, -3.027376345333610441, -5.243569643749999898 ) ) ;
#28200 = CARTESIAN_POINT ( 'NONE',  ( 27.41250000122903430, 0.000000000000000000, 4.999999999999998224 ) ) ;
#28201 = CARTESIAN_POINT ( 'NONE',  ( 24.72187500061451360, 2.746126346562645981, -4.756430356249997438 ) ) ;
#28202 = CARTESIAN_POINT ( 'NONE',  ( 20.09062500061451573, -3.027376345333610441, -5.243569643749999898 ) ) ;
#28203 = CARTESIAN_POINT ( 'NONE',  ( 13.57500000000000107, 6.123233995736764310E-16, -4.999999999999998224 ) ) ;
#28204 = CARTESIAN_POINT ( 'NONE',  ( -3.756430356250001434, 18.75312499938548427, 32.16877607737301048 ) ) ;
#28205 = CARTESIAN_POINT ( 'NONE',  ( 13.47187500061451537, 3.027376345333613106, -5.243569643749998122 ) ) ;
#28206 = CARTESIAN_POINT ( 'NONE',  ( 12.30937500061451573, 0.000000000000000000, 5.243569643749999010 ) ) ;
#28207 = CARTESIAN_POINT ( 'NONE',  ( 21.34687500061451715, -3.027376345333614438, 5.243569643749998122 ) ) ;
#28208 = EDGE_LOOP ( 'NONE', ( #58448, #53327, #53161, #26313 ) ) ;
#28209 = CARTESIAN_POINT ( 'NONE',  ( 2.878125000614517592, -4.541064518000419881, 2.621784821874995952 ) ) ;
#28210 = CARTESIAN_POINT ( 'NONE',  ( 25.52812500061451573, 6.421520780324663323E-16, -5.243569643749999010 ) ) ;
#28211 = CARTESIAN_POINT ( 'NONE',  ( 27.74062500061451431, -3.027376345333610441, -5.243569643749999898 ) ) ;
#28212 = FACE_OUTER_BOUND ( 'NONE', #7885, .T. ) ;
#28213 = CARTESIAN_POINT ( 'NONE',  ( -1.999999999999997113, 16.02500000000000213, 33.46410161513775705 ) ) ;
#28214 = CARTESIAN_POINT ( 'NONE',  ( 5.559375000614517504, 0.000000000000000000, 5.243569643749999010 ) ) ;
#28215 = CARTESIAN_POINT ( 'NONE',  ( 12.56250000122903465, 0.000000000000000000, 4.999999999999998224 ) ) ;
#28216 = CARTESIAN_POINT ( 'NONE',  ( 8.100000001229034297, -2.886751345948129988, 4.999999999999997335 ) ) ;
#28217 = CARTESIAN_POINT ( 'NONE',  ( 3.853125000614517681, -4.541064518000417216, -2.621784821875001281 ) ) ;
#28218 = CARTESIAN_POINT ( 'NONE',  ( 4.000000000000000000, 19.19374999877096499, 30.00000000000000000 ) ) ;
#28219 = CARTESIAN_POINT ( 'NONE',  ( 16.21875000122903288, -5.773502691896255534, -1.060575238724906372E-15 ) ) ;
#28220 = CARTESIAN_POINT ( 'NONE',  ( 11.03437500061451715, -4.541064518000419881, 2.621784821874995952 ) ) ;
#28221 = CARTESIAN_POINT ( 'NONE',  ( 18.85312500061451502, 4.541064518000418104, -2.621784821874998173 ) ) ;
#28222 = CARTESIAN_POINT ( 'NONE',  ( 12.87187500061451750, -6.054752690667223547, -1.112240025338166033E-15 ) ) ;
#28223 = CARTESIAN_POINT ( 'NONE',  ( 4.190625000614518925, -3.027376345333614438, 5.243569643749998122 ) ) ;
#28224 = CARTESIAN_POINT ( 'NONE',  ( 23.03437500061451715, 4.541064518000418104, 2.621784821874999949 ) ) ;
#28225 = CARTESIAN_POINT ( 'NONE',  ( 8.784375000614518925, -4.541064518000419881, 2.621784821874995952 ) ) ;
#28226 = CARTESIAN_POINT ( 'NONE',  ( 5.428125000614517859, 4.541064518000418104, 2.621784821874999949 ) ) ;
#28227 = DIRECTION ( 'NONE',  ( -1.000000000000000000, -0.000000000000000000, -0.000000000000000000 ) ) ;
#28228 = CARTESIAN_POINT ( 'NONE',  ( 6.525000001229033231, 2.886751345948129099, -4.999999999999998224 ) ) ;
#28229 = CARTESIAN_POINT ( 'NONE',  ( 20.61562500061451431, 3.027376345333613106, -5.243569643749998122 ) ) ;
#28230 = CARTESIAN_POINT ( 'NONE',  ( 7.012500001229035718, 4.330127018922192761, -2.499999999999997780 ) ) ;
#28231 = CARTESIAN_POINT ( 'NONE',  ( 16.90312500061451573, -4.541064518000417216, -2.621784821875001281 ) ) ;
#28232 = CARTESIAN_POINT ( 'NONE',  ( 13.07812500061451821, 4.541064518000418104, 2.621784821874999949 ) ) ;
#28233 = CARTESIAN_POINT ( 'NONE',  ( 26.70937500061451431, 0.000000000000000000, 4.756430356249998326 ) ) ;
#28234 = CARTESIAN_POINT ( 'NONE',  ( 13.64999999999999858, 4.330127018922192761, -2.499999999999997780 ) ) ;
#28235 = CARTESIAN_POINT ( 'NONE',  ( 9.300000001229035362, 5.773502691896255534, 3.535250795749688894E-16 ) ) ;
#28236 = CARTESIAN_POINT ( 'NONE',  ( 6.740625000614516082, 6.054752690667223547, 3.707466751127219781E-16 ) ) ;
#28237 = CARTESIAN_POINT ( 'NONE',  ( 19.83750000122903145, -4.330127018922194537, 2.499999999999995559 ) ) ;
#28238 = CARTESIAN_POINT ( 'NONE',  ( 26.32499999999999929, 4.330127018922191873, 2.499999999999999556 ) ) ;
#28239 = CARTESIAN_POINT ( 'NONE',  ( 4.243569643749999898, 11.98437500061451821, -30.00000000000000000 ) ) ;
#28240 = CARTESIAN_POINT ( 'NONE',  ( 4.898734551532200499, 1.001199177798645534, 4.898734551532190729 ) ) ;
#28241 = EDGE_CURVE ( 'NONE', #16088, #55534, #72179, .T. ) ;
#28242 = CARTESIAN_POINT ( 'NONE',  ( 3.787500001229033408, 6.123233995736764310E-16, -4.999999999999998224 ) ) ;
#28243 = DIRECTION ( 'NONE',  ( 0.000000000000000000, 0.000000000000000000, -1.000000000000000000 ) ) ;
#28244 = CARTESIAN_POINT ( 'NONE',  ( 21.60937500061451644, 4.541064518000418104, -2.621784821874998173 ) ) ;
#28245 = CARTESIAN_POINT ( 'NONE',  ( -5.810221930991193690E-16, 18.65000000122903501, 26.00000000000000355 ) ) ;
#28246 = CARTESIAN_POINT ( 'NONE',  ( 17.16562500061451502, 3.027376345333611329, 5.243569643749999010 ) ) ;
#28247 = CARTESIAN_POINT ( 'NONE',  ( 11.53125000122903465, 4.330127018922191873, 2.499999999999999556 ) ) ;
#28248 = CARTESIAN_POINT ( 'NONE',  ( 0.000000000000000000, 27.50000000000000000, 26.00000000000000000 ) ) ;
#28249 = CARTESIAN_POINT ( 'NONE',  ( 4.500000000000000888, -4.330127018922190985, -2.500000000000001332 ) ) ;
#28250 = CARTESIAN_POINT ( 'NONE',  ( 28.09687500061451360, -3.027376345333614438, 5.243569643749998122 ) ) ;
#28251 = CARTESIAN_POINT ( 'NONE',  ( 21.75937500061451146, -5.492252693125287522, -1.008910452111647106E-15 ) ) ;
#28252 = CARTESIAN_POINT ( 'NONE',  ( 11.69062500061451360, 6.054752690667223547, 3.707466751127219781E-16 ) ) ;
#28253 = CARTESIAN_POINT ( 'NONE',  ( 10.20937500061451786, -4.541064518000417216, -2.621784821875001281 ) ) ;
#28254 = ORIENTED_EDGE ( 'NONE', *, *, #34819, .T. ) ;
#28255 = CARTESIAN_POINT ( 'NONE',  ( 29.76562500061451644, 3.027376345333611329, 5.243569643749999010 ) ) ;
#28256 = CARTESIAN_POINT ( 'NONE',  ( 21.89062500061451289, -3.027376345333610441, -5.243569643749999898 ) ) ;
#28257 = DIRECTION ( 'NONE',  ( 0.000000000000000000, 0.000000000000000000, -1.000000000000000000 ) ) ;
#28258 = CARTESIAN_POINT ( 'NONE',  ( -5.810221930991193690E-16, 15.50000000122903465, -34.00000000000000000 ) ) ;
#28259 = CARTESIAN_POINT ( 'NONE',  ( 11.28749999999999787, -2.886751345948125991, -5.000000000000000000 ) ) ;
#28260 = CARTESIAN_POINT ( 'NONE',  ( 22.42500000122903359, 2.886751345948126879, 4.999999999999999112 ) ) ;
#28261 = CARTESIAN_POINT ( 'NONE',  ( 16.97812500061451502, 6.421520780324663323E-16, -5.243569643749999010 ) ) ;
#28262 = CARTESIAN_POINT ( 'NONE',  ( 12.75937500061451502, -5.492252693125287522, -1.008910452111647106E-15 ) ) ;
#28263 = EDGE_LOOP ( 'NONE', ( #2841, #44322, #26359, #33069 ) ) ;
#28264 = CARTESIAN_POINT ( 'NONE',  ( 18.97499999999999787, 6.123233995736764310E-16, -4.999999999999998224 ) ) ;
#28265 = CARTESIAN_POINT ( 'NONE',  ( 24.93750000000000355, 5.773502691896255534, 3.535250795749688894E-16 ) ) ;
#28266 = CARTESIAN_POINT ( 'NONE',  ( 21.23437500061451644, 4.541064518000418104, 2.621784821874999949 ) ) ;
#28267 = CARTESIAN_POINT ( 'NONE',  ( 26.35312500061451857, -4.541064518000417216, -2.621784821875001281 ) ) ;
#28268 = ORIENTED_EDGE ( 'NONE', *, *, #10575, .F. ) ;
#28269 = CARTESIAN_POINT ( 'NONE',  ( -1.999999999999997113, 17.03750000122903430, 33.46410161513775705 ) ) ;
#28270 = CARTESIAN_POINT ( 'NONE',  ( 8.803125000614517859, -4.541064518000417216, -2.621784821875001281 ) ) ;
#28271 = CARTESIAN_POINT ( 'NONE',  ( 0.000000000000000000, 20.00000000000000000, -33.99999999999999289 ) ) ;
#28272 = CARTESIAN_POINT ( 'NONE',  ( 15.45000000000000107, 4.330127018922192761, -2.499999999999997780 ) ) ;
#28273 = CARTESIAN_POINT ( 'NONE',  ( -4.243569643749999898, 18.00312500061451715, 30.00000000000000000 ) ) ;
#28274 = CARTESIAN_POINT ( 'NONE',  ( 5.296875000614518214, -3.027376345333610441, -5.243569643749999898 ) ) ;
#28275 = CARTESIAN_POINT ( 'NONE',  ( 28.24687500061451573, -3.027376345333610441, -5.243569643749999898 ) ) ;
#28276 = EDGE_LOOP ( 'NONE', ( #17061, #18319, #61264, #10091 ) ) ;
#28277 = CARTESIAN_POINT ( 'NONE',  ( 24.96562500061451573, -6.054752690667223547, -1.112240025338166033E-15 ) ) ;
#28278 = CARTESIAN_POINT ( 'NONE',  ( 26.29687500061451644, -3.027376345333614438, 5.243569643749998122 ) ) ;
#28279 = CARTESIAN_POINT ( 'NONE',  ( -4.243569643749999898, 18.86562500061459247, -32.45002607614398471 ) ) ;
#28280 = CARTESIAN_POINT ( 'NONE',  ( 10.76250000000000107, -5.773502691896255534, -1.060575238724906372E-15 ) ) ;
#28281 = CARTESIAN_POINT ( 'NONE',  ( 8.428125000614517859, 6.421520780324663323E-16, -5.243569643749999010 ) ) ;
#28282 = DIRECTION ( 'NONE',  ( -1.000000000000000000, -0.000000000000000000, -0.000000000000000000 ) ) ;
#28283 = CARTESIAN_POINT ( 'NONE',  ( 19.53749999999999432, 5.773502691896255534, 3.535250795749688401E-16 ) ) ;
#28284 = CARTESIAN_POINT ( 'NONE',  ( 26.69062500061451715, -3.027376345333614438, 5.243569643749998122 ) ) ;
#28285 = CARTESIAN_POINT ( 'NONE',  ( 29.37187500061451573, -4.119189519843968306, 2.378215178124996054 ) ) ;
#28286 = CARTESIAN_POINT ( 'NONE',  ( 12.57187500061451857, 2.746126346562645981, -4.756430356249997438 ) ) ;
#28287 = CARTESIAN_POINT ( 'NONE',  ( 3.140625000614516882, 6.054752690667223547, 3.707466751127219781E-16 ) ) ;
#28288 = CARTESIAN_POINT ( 'NONE',  ( 20.25937500061451857, 4.541064518000418104, -2.621784821874998173 ) ) ;
#28289 = CARTESIAN_POINT ( 'NONE',  ( -4.243569643749997233, 14.94687500061451679, 32.45002607614398471 ) ) ;
#28290 = CARTESIAN_POINT ( 'NONE',  ( 21.45937500061451786, -4.541064518000417216, -2.621784821875001281 ) ) ;
#28291 = CARTESIAN_POINT ( 'NONE',  ( 3.637500000000001954, -2.886751345948125991, -5.000000000000000000 ) ) ;
#28292 = CARTESIAN_POINT ( 'NONE',  ( 9.001249775931846008E-16, 18.62187500061451573, 34.90005215228797653 ) ) ;
#28293 = CARTESIAN_POINT ( 'NONE',  ( 9.515625000614518214, 3.027376345333611329, 5.243569643749999010 ) ) ;
#28294 = CARTESIAN_POINT ( 'NONE',  ( 5.859375000614519102, 4.541064518000418104, -2.621784821874998173 ) ) ;
#28295 = CARTESIAN_POINT ( 'NONE',  ( 11.75625000122903430, -4.330127018922190985, -2.500000000000001332 ) ) ;
#28296 = CARTESIAN_POINT ( 'NONE',  ( 7.265625000614516438, 3.027376345333611329, 5.243569643749999010 ) ) ;
#28297 = CARTESIAN_POINT ( 'NONE',  ( 11.40937500061451892, 0.000000000000000000, 5.243569643749999010 ) ) ;
#28298 = CARTESIAN_POINT ( 'NONE',  ( 18.15000000122903501, -2.886751345948125991, -5.000000000000000000 ) ) ;
#28299 = CARTESIAN_POINT ( 'NONE',  ( 8.821875000614518569, -6.054752690667223547, -1.112240025338166033E-15 ) ) ;
#28300 = CARTESIAN_POINT ( 'NONE',  ( 8.990625000614516082, 6.054752690667223547, 3.707466751127219781E-16 ) ) ;
#28301 = CARTESIAN_POINT ( 'NONE',  ( 4.125000001229034652, -5.773502691896255534, -1.060575238724906372E-15 ) ) ;
#28302 = CARTESIAN_POINT ( 'NONE',  ( 25.89375000122903003, 5.773502691896255534, 3.535250795749688894E-16 ) ) ;
#28303 = CARTESIAN_POINT ( 'NONE',  ( 20.10937500061451289, -4.541064518000417216, -2.621784821875001281 ) ) ;
#28304 = CARTESIAN_POINT ( 'NONE',  ( 4.486351857634337748, 2.207646840049596992, 4.593693573296974364 ) ) ;
#28305 = CARTESIAN_POINT ( 'NONE',  ( 26.80312500061451431, -4.541064518000417216, -2.621784821875001281 ) ) ;
#28306 = CARTESIAN_POINT ( 'NONE',  ( 12.29062500061451857, -3.027376345333614438, 5.243569643749998122 ) ) ;
#28307 = CARTESIAN_POINT ( 'NONE',  ( 29.14687500061451431, -3.027376345333610441, -5.243569643749999898 ) ) ;
#28308 = CARTESIAN_POINT ( 'NONE',  ( 13.27500000122903323, 2.886751345948129099, -4.999999999999998224 ) ) ;
#28309 = ADVANCED_FACE ( 'NONE', ( #5100, #44990 ), #67528, .F. ) ;
#28310 = CARTESIAN_POINT ( 'NONE',  ( 26.72812500061451502, -4.541064518000419881, 2.621784821874995952 ) ) ;
#28311 = CARTESIAN_POINT ( 'NONE',  ( -4.243569643749999898, 14.81562500061451715, -32.45002607614398471 ) ) ;
#28312 = CARTESIAN_POINT ( 'NONE',  ( 16.05000000122903359, 5.773502691896255534, 3.535250795749688894E-16 ) ) ;
#28313 = CARTESIAN_POINT ( 'NONE',  ( 13.76250000000000107, 2.886751345948126879, 4.999999999999999112 ) ) ;
#28314 = CARTESIAN_POINT ( 'NONE',  ( 21.70312500061451644, 0.000000000000000000, 5.243569643749999010 ) ) ;
#28315 = CARTESIAN_POINT ( 'NONE',  ( 8.259375000614518569, 0.000000000000000000, 5.243569643749999010 ) ) ;
#28316 = CARTESIAN_POINT ( 'NONE',  ( 8.062500001229034652, 0.000000000000000000, 4.999999999999998224 ) ) ;
#28317 = CARTESIAN_POINT ( 'NONE',  ( 17.32500000122903216, 2.886751345948129099, -4.999999999999998224 ) ) ;
#28318 = CARTESIAN_POINT ( 'NONE',  ( 13.07812500061451821, 4.541064518000418104, 2.621784821874999949 ) ) ;
#28319 =( BOUNDED_CURVE ( )  B_SPLINE_CURVE ( 2, ( #11420, #21762, #39869, #33219, #17661, #44323, #67935, #61650, #33577 ),
 .UNSPECIFIED., .F., .F. ) 
 B_SPLINE_CURVE_WITH_KNOTS ( ( 3, 2, 2, 2, 3 ),
 ( 0.9027777777777777901, 0.9074074074074074403, 0.9166666666666666297, 0.9259259259259259300, 0.9305555555555555802 ),
 .UNSPECIFIED. ) 
 CURVE ( )  GEOMETRIC_REPRESENTATION_ITEM ( )  RATIONAL_B_SPLINE_CURVE ( ( 0.9330127018922194093, 0.9330127018922194093, 1.000000000000000000, 0.8660254037844387076, 1.000000000000000000, 0.8660254037844387076, 1.000000000000000000, 0.9330127018922194093, 0.9330127018922194093 ) ) 
 REPRESENTATION_ITEM ( '' )  );
#28320 = CARTESIAN_POINT ( 'NONE',  ( 16.86562500061451786, -6.054752690667223547, -1.112240025338166033E-15 ) ) ;
#28321 = CARTESIAN_POINT ( 'NONE',  ( 28.50000000122903288, -2.886751345948125991, -5.000000000000000000 ) ) ;
#28322 = CARTESIAN_POINT ( 'NONE',  ( 23.69999999999999929, 0.000000000000000000, 4.999999999999998224 ) ) ;
#28323 = CARTESIAN_POINT ( 'NONE',  ( 23.37187500061451573, 3.027376345333613106, -5.243569643749998122 ) ) ;
#28324 = CARTESIAN_POINT ( 'NONE',  ( 10.38750000122903572, -4.330127018922194537, 2.499999999999995559 ) ) ;
#28325 = CARTESIAN_POINT ( 'NONE',  ( 28.09687500061451360, -3.027376345333614438, 5.243569643749998122 ) ) ;
#28326 = CARTESIAN_POINT ( 'NONE',  ( 5.709375000614517859, -4.541064518000417216, -2.621784821875001281 ) ) ;
#28327 = CARTESIAN_POINT ( 'NONE',  ( 24.77812500061451217, 4.541064518000418104, 2.621784821874999949 ) ) ;
#28328 = CARTESIAN_POINT ( 'NONE',  ( 1.878215178124997609, 14.47812499938548214, 33.25316411605952993 ) ) ;
#28329 = CARTESIAN_POINT ( 'NONE',  ( 1.071796769724490339, 19.86740381056766225, -34.00000000000000000 ) ) ;
#28330 = CARTESIAN_POINT ( 'NONE',  ( 9.121875000614517504, 3.027376345333611329, 5.243569643749999010 ) ) ;
#28331 = PLANE ( 'NONE',  #31300 ) ;
#28332 = CARTESIAN_POINT ( 'NONE',  ( 3.684375000614518836, 4.541064518000418104, 2.621784821874999949 ) ) ;
#28333 = CARTESIAN_POINT ( 'NONE',  ( 5.634375000614519458, -4.541064518000419881, 2.621784821874995952 ) ) ;
#28334 = CARTESIAN_POINT ( 'NONE',  ( 4.898587196589412829E-16, 27.50000000000000000, 34.00000000000000000 ) ) ;
#28335 = CARTESIAN_POINT ( 'NONE',  ( 25.84687500061451360, -3.027376345333614438, 5.243569643749998122 ) ) ;
#28336 = EDGE_CURVE ( 'NONE', #54892, #33433, #12089, .T. ) ;
#28337 = CARTESIAN_POINT ( 'NONE',  ( 27.69375000122903074, 5.773502691896255534, 3.535250795749688401E-16 ) ) ;
#28338 = CARTESIAN_POINT ( 'NONE',  ( 18.67500000000000071, 4.330127018922191873, 2.499999999999999556 ) ) ;
#28339 = VERTEX_POINT ( 'NONE', #6550 ) ;
#28340 = CARTESIAN_POINT ( 'NONE',  ( 26.88749999999999574, -2.886751345948129988, 4.999999999999997335 ) ) ;
#28341 = CARTESIAN_POINT ( 'NONE',  ( 29.82187500061451502, 3.027376345333611329, 5.243569643749999010 ) ) ;
#28342 = ORIENTED_EDGE ( 'NONE', *, *, #16791, .F. ) ;
#28343 = CARTESIAN_POINT ( 'NONE',  ( 16.15312500061451573, 4.541064518000418104, -2.621784821874998173 ) ) ;
#28344 = CARTESIAN_POINT ( 'NONE',  ( 8.203125000614518214, 0.000000000000000000, 5.243569643749999010 ) ) ;
#28345 = CARTESIAN_POINT ( 'NONE',  ( 19.32187500061451857, 4.119189519843966529, 2.378215178124999607 ) ) ;
#28346 = CARTESIAN_POINT ( 'NONE',  ( 5.296875000614518214, -3.027376345333610441, -5.243569643749999898 ) ) ;
#28347 = CARTESIAN_POINT ( 'NONE',  ( 17.21250000122903145, -4.330127018922190985, -2.500000000000001332 ) ) ;
#28348 = CARTESIAN_POINT ( 'NONE',  ( 22.61250000000000071, 2.886751345948129099, -4.999999999999998224 ) ) ;
#28349 = CARTESIAN_POINT ( 'NONE',  ( 34.99999999999999289, -2.499999999999999556, -3.499999999999999556 ) ) ;
#28350 = CARTESIAN_POINT ( 'NONE',  ( 6.421875000614519102, 3.027376345333611329, 5.243569643749999010 ) ) ;
#28351 = CARTESIAN_POINT ( 'NONE',  ( 12.57187500061451857, 3.027376345333613106, -5.243569643749998122 ) ) ;
#28352 = CARTESIAN_POINT ( 'NONE',  ( 21.68437500061451573, 4.541064518000418104, 2.621784821874999949 ) ) ;
#28353 = CARTESIAN_POINT ( 'NONE',  ( -1.071796769724491005, 14.50759618943233420, -34.00000000000000000 ) ) ;
#28354 = ORIENTED_EDGE ( 'NONE', *, *, #60834, .F. ) ;
#28355 = CARTESIAN_POINT ( 'NONE',  ( 3.309375000614518836, 0.000000000000000000, 5.243569643749999010 ) ) ;
#28356 =( BOUNDED_CURVE ( )  B_SPLINE_CURVE ( 2, ( #14314, #20575, #64190, #59366, #58642, #42765, #65285 ),
 .UNSPECIFIED., .F., .F. ) 
 B_SPLINE_CURVE_WITH_KNOTS ( ( 3, 2, 2, 3 ),
 ( 0.05833333333333334120, 0.06111111111111110911, 0.06388888888888888395, 0.06666666666666665186 ),
 .UNSPECIFIED. ) 
 CURVE ( )  GEOMETRIC_REPRESENTATION_ITEM ( )  RATIONAL_B_SPLINE_CURVE ( ( 0.9999999999999995559, 0.8660254037844390407, 1.000000000000000000, 0.8660254037844387076, 1.000000000000000000, 0.8660254037844393737, 0.9999999999999993339 ) ) 
 REPRESENTATION_ITEM ( '' )  );
#28357 = CARTESIAN_POINT ( 'NONE',  ( 5.934375000614517504, 4.541064518000418104, 2.621784821874999949 ) ) ;
#28358 = CARTESIAN_POINT ( 'NONE',  ( 18.00000000000000355, -4.330127018922190985, -2.500000000000001332 ) ) ;
#28359 = CARTESIAN_POINT ( 'NONE',  ( 15.47812500061451679, -4.541064518000419881, 2.621784821874995952 ) ) ;
#28360 = CARTESIAN_POINT ( 'NONE',  ( 4.000000000000000000, 17.44999999999999929, 30.00000000000000000 ) ) ;
#28361 = CARTESIAN_POINT ( 'NONE',  ( 18.30000000000000071, 0.000000000000000000, 4.999999999999998224 ) ) ;
#28362 = CARTESIAN_POINT ( 'NONE',  ( 20.70937500061451786, 4.119189519843966529, -2.378215178124998275 ) ) ;
#28363 = CARTESIAN_POINT ( 'NONE',  ( 11.05312500061451608, -4.541064518000417216, -2.621784821875001281 ) ) ;
#28364 = CARTESIAN_POINT ( 'NONE',  ( 26.03437500061451715, 6.421520780324663323E-16, -5.243569643749999010 ) ) ;
#28365 =( NAMED_UNIT ( * ) SI_UNIT ( $, .STERADIAN. ) SOLID_ANGLE_UNIT ( ) );
#28366 = CARTESIAN_POINT ( 'NONE',  ( 29.48437500061451644, -4.541064518000419881, 2.621784821874995952 ) ) ;
#28367 = CARTESIAN_POINT ( 'NONE',  ( 9.937500000000001776, -2.886751345948125991, -5.000000000000000000 ) ) ;
#28368 = CARTESIAN_POINT ( 'NONE',  ( 3.999999999999999112, 14.48750000122903536, 30.00000000000000000 ) ) ;
#28369 = CARTESIAN_POINT ( 'NONE',  ( 8.512500001229033941, 0.000000000000000000, 4.999999999999998224 ) ) ;
#28370 = CARTESIAN_POINT ( 'NONE',  ( 20.52187500061451786, -6.054752690667223547, -1.112240025338166033E-15 ) ) ;
#28371 = CARTESIAN_POINT ( 'NONE',  ( 13.20937500061451786, 0.000000000000000000, 5.243569643749999010 ) ) ;
#28372 = CARTESIAN_POINT ( 'NONE',  ( 23.36250000122903359, 0.000000000000000000, 4.999999999999998224 ) ) ;
#28373 = ORIENTED_EDGE ( 'NONE', *, *, #70404, .F. ) ;
#28374 = CARTESIAN_POINT ( 'NONE',  ( 15.47812500061451679, -4.541064518000419881, 2.621784821874995952 ) ) ;
#28375 = CARTESIAN_POINT ( 'NONE',  ( 26.73750000122903003, 6.123233995736764310E-16, -4.999999999999998224 ) ) ;
#28376 = CARTESIAN_POINT ( 'NONE',  ( 14.78437500061451715, 6.421520780324663323E-16, -5.243569643749999010 ) ) ;
#28377 = CARTESIAN_POINT ( 'NONE',  ( 3.685019977366421173, 9.302529035819388170, -25.24908463647652823 ) ) ;
#28378 = CARTESIAN_POINT ( 'NONE',  ( 17.61562500061451786, 3.027376345333611329, 5.243569643749999010 ) ) ;
#28379 = CARTESIAN_POINT ( 'NONE',  ( 30.00000000000000000, 0.000000000000000000, 4.999999999999998224 ) ) ;
#28380 = CARTESIAN_POINT ( 'NONE',  ( 26.44687500061451502, -3.027376345333610441, -5.243569643749999898 ) ) ;
#28381 = CARTESIAN_POINT ( 'NONE',  ( 2.121784821874999061, 10.65312500061451750, 26.32496088578401583 ) ) ;
#28382 = CARTESIAN_POINT ( 'NONE',  ( 15.15937500061451715, -4.541064518000417216, -2.621784821875001281 ) ) ;
#28383 = CARTESIAN_POINT ( 'NONE',  ( 13.12500000122903288, -5.773502691896255534, -1.060575238724906372E-15 ) ) ;
#28384 = CARTESIAN_POINT ( 'NONE',  ( 0.000000000000000000, 20.00000000000000000, -30.00000000000000000 ) ) ;
#28385 = CARTESIAN_POINT ( 'NONE',  ( -3.000416591977282496E-16, 19.74687500061451928, -34.90005215228797653 ) ) ;
#28386 = CARTESIAN_POINT ( 'NONE',  ( 19.17187500061451999, -6.054752690667223547, -1.112240025338166033E-15 ) ) ;
#28387 = CARTESIAN_POINT ( 'NONE',  ( 19.38750000122903216, -4.330127018922194537, 2.499999999999995559 ) ) ;
#28388 =( BOUNDED_CURVE ( )  B_SPLINE_CURVE ( 2, ( #12837, #57894, #59345, #58984, #8389, #29833, #2850 ),
 .UNSPECIFIED., .F., .F. ) 
 B_SPLINE_CURVE_WITH_KNOTS ( ( 3, 2, 2, 3 ),
 ( 0.9346169692731971512, 0.9361111111111111160, 0.9388888888888888840, 0.9402232515920995182 ),
 .UNSPECIFIED. ) 
 CURVE ( )  GEOMETRIC_REPRESENTATION_ITEM ( )  RATIONAL_B_SPLINE_CURVE ( ( 0.9333974052703135627, 0.9279362622076117173, 1.000000000000000000, 0.8660254037844387076, 1.000000000000000000, 0.9356425464276099113, 0.9331159465740572756 ) ) 
 REPRESENTATION_ITEM ( '' )  );
#28389 = CARTESIAN_POINT ( 'NONE',  ( 15.68437500061451573, 6.421520780324663323E-16, -5.243569643749999010 ) ) ;
#28390 = CARTESIAN_POINT ( 'NONE',  ( 9.001249775931846008E-16, 11.87187500061451750, 34.90005215228797653 ) ) ;
#28391 = CARTESIAN_POINT ( 'NONE',  ( 21.41250000122903074, 4.330127018922192761, -2.499999999999997780 ) ) ;
#28392 = CARTESIAN_POINT ( 'NONE',  ( 14.76562500061451821, 3.027376345333613106, -5.243569643749998122 ) ) ;
#28393 = CARTESIAN_POINT ( 'NONE',  ( 28.94062500061452070, -3.027376345333614438, 5.243569643749998122 ) ) ;
#28394 = ORIENTED_EDGE ( 'NONE', *, *, #38051, .F. ) ;
#28395 = ORIENTED_EDGE ( 'NONE', *, *, #15666, .F. ) ;
#28396 = CARTESIAN_POINT ( 'NONE',  ( 20.43749999999999645, 5.773502691896255534, 3.535250795749688894E-16 ) ) ;
#28397 = CARTESIAN_POINT ( 'NONE',  ( 17.68125000122903501, 6.123233995736764310E-16, -4.999999999999998224 ) ) ;
#28398 = CARTESIAN_POINT ( 'NONE',  ( 3.365625000614516082, -6.054752690667223547, -1.112240025338166033E-15 ) ) ;
#28399 = CARTESIAN_POINT ( 'NONE',  ( 16.01250000122903216, 4.330127018922192761, -2.499999999999997780 ) ) ;
#28400 = CARTESIAN_POINT ( 'NONE',  ( 19.82812500061451644, 4.541064518000418104, 2.621784821874999949 ) ) ;
#28401 = EDGE_CURVE ( 'NONE', #20653, #66446, #16494, .T. ) ;
#28402 = CARTESIAN_POINT ( 'NONE',  ( 24.96562500061451573, -6.054752690667223547, -1.112240025338166033E-15 ) ) ;
#28403 = CARTESIAN_POINT ( 'NONE',  ( 6.103125000614515905, -4.541064518000417216, -2.621784821875001281 ) ) ;
#28404 = CARTESIAN_POINT ( 'NONE',  ( 29.58749999999999858, -2.886751345948129988, 4.999999999999997335 ) ) ;
#28405 = CARTESIAN_POINT ( 'NONE',  ( 17.83125000122903003, 4.330127018922191873, 2.499999999999999556 ) ) ;
#28406 =( BOUNDED_CURVE ( )  B_SPLINE_CURVE ( 2, ( #3868, #49298, #14933, #38196, #70359, #20463, #37834 ),
 .UNSPECIFIED., .F., .F. ) 
 B_SPLINE_CURVE_WITH_KNOTS ( ( 3, 2, 2, 3 ),
 ( 0.6666666666666666297, 0.6694444444444443976, 0.6722222222222222765, 0.6750000000000000444 ),
 .UNSPECIFIED. ) 
 CURVE ( )  GEOMETRIC_REPRESENTATION_ITEM ( )  RATIONAL_B_SPLINE_CURVE ( ( 1.000000000000000000, 0.8660254037844387076, 1.000000000000000000, 0.8660254037844387076, 1.000000000000000000, 0.8660254037844387076, 1.000000000000000000 ) ) 
 REPRESENTATION_ITEM ( '' )  );
#28407 = CARTESIAN_POINT ( 'NONE',  ( 9.646875000614516082, -2.746126346562646425, 4.756430356249996549 ) ) ;
#28408 = CARTESIAN_POINT ( 'NONE',  ( 11.17500000122903536, 2.886751345948126879, 4.999999999999998224 ) ) ;
#28409 = CARTESIAN_POINT ( 'NONE',  ( 4.000000000000000000, 11.75000000122903643, -27.69059892324149530 ) ) ;
#28410 = CARTESIAN_POINT ( 'NONE',  ( 9.001249775931846008E-16, 19.07187500061451502, -25.09994784771203058 ) ) ;
#28411 = CARTESIAN_POINT ( 'NONE',  ( 6.600000001229032520, 5.773502691896255534, 3.535250795749688894E-16 ) ) ;
#28412 = CARTESIAN_POINT ( 'NONE',  ( 8.137500000000002842, -2.886751345948125991, -5.000000000000000000 ) ) ;
#28413 = CARTESIAN_POINT ( 'NONE',  ( 3.750000001229034652, -2.886751345948125991, -5.000000000000000000 ) ) ;
#28414 = CARTESIAN_POINT ( 'NONE',  ( 12.15937500061451892, 4.541064518000418104, -2.621784821874998173 ) ) ;
#28415 = CARTESIAN_POINT ( 'NONE',  ( 29.80312500061451431, 0.000000000000000000, 5.243569643749999010 ) ) ;
#28416 = CARTESIAN_POINT ( 'NONE',  ( 3.543100117577441033, 4.136409934384715825, -3.322667120213021796 ) ) ;
#28417 = CARTESIAN_POINT ( 'NONE',  ( 12.22499999999999964, 6.123233995736764310E-16, -4.999999999999998224 ) ) ;
#28418 = CARTESIAN_POINT ( 'NONE',  ( -3.999999999999999112, 19.62500000122903288, -32.30940107675850470 ) ) ;
#28419 = CARTESIAN_POINT ( 'NONE',  ( 9.496875000614517504, 6.054752690667223547, 3.707466751127219781E-16 ) ) ;
#28420 = CARTESIAN_POINT ( 'NONE',  ( 3.619842856578028734, -3.449164782042274169, -3.619842856578066481 ) ) ;
#28421 = CARTESIAN_POINT ( 'NONE',  ( 25.10625000122903216, 0.000000000000000000, 4.999999999999998224 ) ) ;
#28422 = CARTESIAN_POINT ( 'NONE',  ( -3.000416591977282496E-16, 16.54062500061459673, 25.09994784771203058 ) ) ;
#28423 = CARTESIAN_POINT ( 'NONE',  ( 21.19687500061451502, 6.054752690667223547, 3.707466751127219781E-16 ) ) ;
#28424 = AXIS2_PLACEMENT_3D ( 'NONE', #25803, #71602, #48341 ) ;
#28425 = CARTESIAN_POINT ( 'NONE',  ( 2.791126035847173448, -4.148447354374293461, 2.973833421074890904 ) ) ;
#28426 = CARTESIAN_POINT ( 'NONE',  ( 29.66250000122903074, 0.000000000000000000, 4.999999999999998224 ) ) ;
#28427 = CARTESIAN_POINT ( 'NONE',  ( 17.29687500061451644, -4.119189519843965641, -2.378215178125001383 ) ) ;
#28428 = CARTESIAN_POINT ( 'NONE',  ( 22.71562500061451573, -6.054752690667223547, -1.112240025338166033E-15 ) ) ;
#28429 = CARTESIAN_POINT ( 'NONE',  ( 15.55312500061451608, -4.541064518000417216, -2.621784821875001281 ) ) ;
#28430 = CARTESIAN_POINT ( 'NONE',  ( 26.44687500061451502, 4.119189519843966529, -2.378215178124998275 ) ) ;
#28431 = CARTESIAN_POINT ( 'NONE',  ( 11.40937500061451892, 0.000000000000000000, 5.243569643749999010 ) ) ;
#28432 = CARTESIAN_POINT ( 'NONE',  ( 28.91250000000000497, 2.886751345948129099, -4.999999999999998224 ) ) ;
#28433 = CARTESIAN_POINT ( 'NONE',  ( 24.93750000122903288, 6.123233995736764310E-16, -4.999999999999998224 ) ) ;
#28434 = CARTESIAN_POINT ( 'NONE',  ( 4.734375000614518214, -4.541064518000419881, 2.621784821874995952 ) ) ;
#28435 = CARTESIAN_POINT ( 'NONE',  ( 14.67187500061451821, -6.054752690667223547, -1.112240025338166033E-15 ) ) ;
#28436 = CARTESIAN_POINT ( 'NONE',  ( 29.85937500061451644, 0.000000000000000000, 5.243569643749999010 ) ) ;
#28437 = DIRECTION ( 'NONE',  ( 0.000000000000000000, 0.000000000000000000, 1.000000000000000000 ) ) ;
#28438 = ADVANCED_FACE ( 'NONE', ( #51253 ), #68610, .F. ) ;
#28439 = CARTESIAN_POINT ( 'NONE',  ( 15.69375000122903074, -2.886751345948130876, 4.999999999999996447 ) ) ;
#28440 = CARTESIAN_POINT ( 'NONE',  ( 23.29687500061451644, -3.027376345333610441, -5.243569643749999898 ) ) ;
#28441 = CARTESIAN_POINT ( 'NONE',  ( 13.80937500061451750, -4.541064518000417216, -2.621784821875001281 ) ) ;
#28442 = CARTESIAN_POINT ( 'NONE',  ( 3.756430356249998770, 15.86562499938548321, 32.16877607737302469 ) ) ;
#28443 = CARTESIAN_POINT ( 'NONE',  ( 25.80000000000000071, 4.330127018922192761, -2.499999999999997780 ) ) ;
#28444 = DIRECTION ( 'NONE',  ( 0.000000000000000000, 0.000000000000000000, -1.000000000000000000 ) ) ;
#28445 = CARTESIAN_POINT ( 'NONE',  ( 28.77187500061451431, 2.746126346562645981, -4.756430356249997438 ) ) ;
#28446 = CARTESIAN_POINT ( 'NONE',  ( 16.41562500061451857, -6.054752690667223547, -1.112240025338166033E-15 ) ) ;
#28447 = CARTESIAN_POINT ( 'NONE',  ( 6.262500000000000178, -5.773502691896255534, -1.060575238724906372E-15 ) ) ;
#28448 = CARTESIAN_POINT ( 'NONE',  ( 2.915625000614516793, -6.054752690667223547, -1.112240025338166033E-15 ) ) ;
#28449 = CARTESIAN_POINT ( 'NONE',  ( 16.42500000000000071, 4.330127018922191873, 2.499999999999999556 ) ) ;
#28450 = CARTESIAN_POINT ( 'NONE',  ( -3.000416591977282496E-16, 13.84062500061451928, 25.09994784771203058 ) ) ;
#28451 = LINE ( 'NONE', #16988, #44330 ) ;
#28452 = CARTESIAN_POINT ( 'NONE',  ( 21.71250000122903501, -4.330127018922190985, -2.500000000000001332 ) ) ;
#28453 = CARTESIAN_POINT ( 'NONE',  ( 11.19375000122903074, -2.886751345948074920, 5.000000000000092371 ) ) ;
#28454 = CARTESIAN_POINT ( 'NONE',  ( 26.25937500061451857, 0.000000000000000000, 5.243569643749999010 ) ) ;
#28455 = ORIENTED_EDGE ( 'NONE', *, *, #33822, .F. ) ;
#28456 = CARTESIAN_POINT ( 'NONE',  ( 21.44062500061452070, -3.027376345333610441, -5.243569643749999898 ) ) ;
#28457 = CARTESIAN_POINT ( 'NONE',  ( 21.42187500061451644, -6.054752690667223547, -1.112240025338166033E-15 ) ) ;
#28458 = CARTESIAN_POINT ( 'NONE',  ( 7.724999999999999645, 6.123233995736764310E-16, -4.999999999999998224 ) ) ;
#28459 = CARTESIAN_POINT ( 'NONE',  ( 9.028125000614517504, 4.541064518000418104, 2.621784821874999949 ) ) ;
#28460 = CARTESIAN_POINT ( 'NONE',  ( 23.95312500061451289, 0.000000000000000000, 5.243569643749999010 ) ) ;
#28461 = CARTESIAN_POINT ( 'NONE',  ( 12.45937500061451786, -4.541064518000417216, -2.621784821875001281 ) ) ;
#28462 = CARTESIAN_POINT ( 'NONE',  ( 16.09687500061452070, -3.027376345333610441, -5.243569643749999898 ) ) ;
#28463 = CARTESIAN_POINT ( 'NONE',  ( 4.411272977760241965, 2.353862934769528348, -4.685547128476531320 ) ) ;
#28464 = CARTESIAN_POINT ( 'NONE',  ( -2.121784821874996840, 18.52812500061451928, 33.67503911421598417 ) ) ;
#28465 = CARTESIAN_POINT ( 'NONE',  ( 22.05000000122903714, -2.886751345948129988, 4.999999999999997335 ) ) ;
#28466 = CARTESIAN_POINT ( 'NONE',  ( 14.44687500061451679, 5.492252693125287522, 3.363034840372157021E-16 ) ) ;
#28467 = CARTESIAN_POINT ( 'NONE',  ( 11.57812500061451644, 6.421520780324663323E-16, -5.243569643749999010 ) ) ;
#28468 = CARTESIAN_POINT ( 'NONE',  ( 5.034375000614519813, 4.541064518000418104, 2.621784821874999949 ) ) ;
#28469 = CARTESIAN_POINT ( 'NONE',  ( 4.171875000614517326, 3.027376345333611329, 5.243569643749999010 ) ) ;
#28470 = VERTEX_POINT ( 'NONE', #63048 ) ;
#28471 = CARTESIAN_POINT ( 'NONE',  ( 24.75937500061451502, 4.541064518000418104, -2.621784821874998173 ) ) ;
#28472 = CARTESIAN_POINT ( 'NONE',  ( 17.35312500061451502, -4.541064518000417216, -2.621784821875001281 ) ) ;
#28473 = CARTESIAN_POINT ( 'NONE',  ( 28.27500000122903145, 2.886751345948126879, 4.999999999999999112 ) ) ;
#28474 = CARTESIAN_POINT ( 'NONE',  ( 26.76562500061451644, -6.054752690667223547, -1.112240025338166033E-15 ) ) ;
#28475 = CARTESIAN_POINT ( 'NONE',  ( 22.43437500061451573, 6.421520780324663323E-16, -5.243569643749999010 ) ) ;
#28476 = CARTESIAN_POINT ( 'NONE',  ( 16.30312500061451786, 0.000000000000000000, 5.243569643749999010 ) ) ;
#28477 = CARTESIAN_POINT ( 'NONE',  ( 9.001249775931846008E-16, 19.52187500061451786, 34.90005215228797653 ) ) ;
#28478 = CARTESIAN_POINT ( 'NONE',  ( 22.86562500061451431, 3.027376345333613106, -5.243569643749998122 ) ) ;
#28479 = CARTESIAN_POINT ( 'NONE',  ( 5.212500001229032343, 4.330127018922192761, -2.499999999999997780 ) ) ;
#28480 = ORIENTED_EDGE ( 'NONE', *, *, #60445, .T. ) ;
#28481 = CARTESIAN_POINT ( 'NONE',  ( 27.15000000000000213, 4.330127018922192761, -2.499999999999997780 ) ) ;
#28482 = CARTESIAN_POINT ( 'NONE',  ( 3.999999999999999112, 12.57500000000000107, -30.00000000000000000 ) ) ;
#28483 = CARTESIAN_POINT ( 'NONE',  ( -3.756430356250000102, 17.47812499938548214, 30.00000000000000000 ) ) ;
#28484 = CARTESIAN_POINT ( 'NONE',  ( 28.45312500061451289, 0.000000000000000000, 5.243569643749999010 ) ) ;
#28485 = CARTESIAN_POINT ( 'NONE',  ( 11.39062500061451644, -3.027376345333614438, 5.243569643749998122 ) ) ;
#28486 = CARTESIAN_POINT ( 'NONE',  ( 21.45000000122903216, 5.773502691896255534, 3.535250795749688894E-16 ) ) ;
#28487 = CARTESIAN_POINT ( 'NONE',  ( 13.13437500061451857, 4.541064518000418104, 2.621784821874999949 ) ) ;
#28488 = CARTESIAN_POINT ( 'NONE',  ( 27.32812500061451644, 6.421520780324663323E-16, -5.243569643749999010 ) ) ;
#28490 = CARTESIAN_POINT ( 'NONE',  ( 28.46249999999999858, 2.886751345948129099, -4.999999999999998224 ) ) ;
#28489 = MECHANICAL_DESIGN_GEOMETRIC_PRESENTATION_REPRESENTATION (  '', ( #39139 ), #63903 ) ;
#28491 = EDGE_CURVE ( 'NONE', #46707, #47914, #49954, .T. ) ;
#28492 = CARTESIAN_POINT ( 'NONE',  ( -3.999999999999997335, 19.25000000122903288, -27.69059892324149175 ) ) ;
#28493 = CARTESIAN_POINT ( 'NONE',  ( 14.58750000122903323, 6.123233995736764310E-16, -4.999999999999998224 ) ) ;
#28494 = CARTESIAN_POINT ( 'NONE',  ( 12.29062500061451857, -3.027376345333614438, 5.243569643749998122 ) ) ;
#28495 = ORIENTED_EDGE ( 'NONE', *, *, #22734, .T. ) ;
#28496 = CARTESIAN_POINT ( 'NONE',  ( 9.028125000614517504, 4.541064518000418104, 2.621784821874999949 ) ) ;
#28497 = CARTESIAN_POINT ( 'NONE',  ( 6.553125000614518747, -4.541064518000417216, -2.621784821875001281 ) ) ;
#28498 = CARTESIAN_POINT ( 'NONE',  ( 16.62187500061451573, 2.746126346562645981, -4.756430356249997438 ) ) ;
#28499 = CARTESIAN_POINT ( 'NONE',  ( 14.96250000000000036, 2.886751345948129099, -4.999999999999998224 ) ) ;
#28500 = CARTESIAN_POINT ( 'NONE',  ( 16.73437500061451644, 4.541064518000418104, 2.621784821874999949 ) ) ;
#28501 = CARTESIAN_POINT ( 'NONE',  ( 11.02500000122903501, 2.886751345948129099, -4.999999999999998224 ) ) ;
#28502 = CARTESIAN_POINT ( 'NONE',  ( 19.84687500061451360, 6.054752690667223547, 3.707466751127219781E-16 ) ) ;
#28503 = CARTESIAN_POINT ( 'NONE',  ( 20.24999999999999645, -4.330127018922190985, -2.500000000000001332 ) ) ;
#28504 = CARTESIAN_POINT ( 'NONE',  ( 19.80937500061451573, 4.541064518000418104, -2.621784821874998173 ) ) ;
#28505 = CARTESIAN_POINT ( 'NONE',  ( -2.121784821874996840, 13.57812500061451644, -26.32496088578401583 ) ) ;
#28506 = FACE_OUTER_BOUND ( 'NONE', #14416, .T. ) ;
#28507 = CARTESIAN_POINT ( 'NONE',  ( 25.43437500061451573, -2.746126346562641984, -4.756430356249999214 ) ) ;
#28508 = DIRECTION ( 'NONE',  ( -1.000000000000000000, -0.000000000000000000, -0.000000000000000000 ) ) ;
#28509 = CARTESIAN_POINT ( 'NONE',  ( 27.40312500061451573, 4.541064518000418104, -2.621784821874998173 ) ) ;
#28510 = CARTESIAN_POINT ( 'NONE',  ( 30.00000000000000000, 0.000000000000000000, 0.000000000000000000 ) ) ;
#28511 = CARTESIAN_POINT ( 'NONE',  ( 27.64687500061452141, -3.027376345333614438, 5.243569643749998122 ) ) ;
#28512 = CARTESIAN_POINT ( 'NONE',  ( 24.44999999999999929, 4.330127018922192761, -2.499999999999997780 ) ) ;
#28513 = CARTESIAN_POINT ( 'NONE',  ( 8.128125000614515372, 4.541064518000418104, 2.621784821874999949 ) ) ;
#28514 = CARTESIAN_POINT ( 'NONE',  ( 23.93437500061451573, -2.746126346562646425, 4.756430356249996549 ) ) ;
#28515 = CARTESIAN_POINT ( 'NONE',  ( 17.93437500061451928, 6.421520780324663323E-16, -5.243569643749999010 ) ) ;
#28516 = CARTESIAN_POINT ( 'NONE',  ( 11.33437500061451608, -2.746126346562646425, 4.756430356249996549 ) ) ;
#28517 = CARTESIAN_POINT ( 'NONE',  ( 6.065625000614516260, -6.054752690667223547, -1.112240025338166033E-15 ) ) ;
#28518 = CARTESIAN_POINT ( 'NONE',  ( 11.48437500061451644, -4.541064518000419881, 2.621784821874995952 ) ) ;
#28519 = ORIENTED_EDGE ( 'NONE', *, *, #60253, .F. ) ;
#28520 = CARTESIAN_POINT ( 'NONE',  ( 22.24687500061451217, -3.027376345333614438, 5.243569643749998122 ) ) ;
#28521 = CARTESIAN_POINT ( 'NONE',  ( 30.00000000000000000, 6.123233995736764310E-16, -4.999999999999998224 ) ) ;
#28522 = CARTESIAN_POINT ( 'NONE',  ( 29.17500000000000071, -4.330127018922194537, 2.499999999999995559 ) ) ;
#28523 = CARTESIAN_POINT ( 'NONE',  ( 3.112500000000000711, -5.773502691896255534, -1.060575238724906372E-15 ) ) ;
#28524 = CARTESIAN_POINT ( 'NONE',  ( 14.17500000122903536, 2.886751345948129099, -4.999999999999998224 ) ) ;
#28525 = CARTESIAN_POINT ( 'NONE',  ( 2.000000000000001332, 12.16250000122903430, 33.46410161513774995 ) ) ;
#28526 = CARTESIAN_POINT ( 'NONE',  ( 22.01250000122903216, 0.000000000000000000, 4.999999999999998224 ) ) ;
#28527 = CARTESIAN_POINT ( 'NONE',  ( 3.309375000614518836, 0.000000000000000000, 5.243569643749999010 ) ) ;
#28528 = ORIENTED_EDGE ( 'NONE', *, *, #64115, .F. ) ;
#28529 = CARTESIAN_POINT ( 'NONE',  ( 13.42499999999999893, -4.330127018922194537, 2.499999999999995559 ) ) ;
#28530 = CARTESIAN_POINT ( 'NONE',  ( 24.32812500061451289, 4.541064518000418104, 2.621784821874999949 ) ) ;
#28531 = CARTESIAN_POINT ( 'NONE',  ( 15.18750000000000000, -2.886751345948129988, 4.999999999999997335 ) ) ;
#28532 =( BOUNDED_CURVE ( )  B_SPLINE_CURVE ( 2, ( #72761, #5886, #67591, #352, #11432, #22859, #45413 ),
 .UNSPECIFIED., .F., .F. ) 
 B_SPLINE_CURVE_WITH_KNOTS ( ( 3, 2, 2, 3 ),
 ( 0.6166666666666666963, 0.6194444444444444642, 0.6222222222222222321, 0.6250000000000000000 ),
 .UNSPECIFIED. ) 
 CURVE ( )  GEOMETRIC_REPRESENTATION_ITEM ( )  RATIONAL_B_SPLINE_CURVE ( ( 1.000000000000000000, 0.8660254037844387076, 1.000000000000000000, 0.8660254037844387076, 1.000000000000000000, 0.8660254037844387076, 1.000000000000000000 ) ) 
 REPRESENTATION_ITEM ( '' )  );
#28533 = EDGE_CURVE ( 'NONE', #43273, #51781, #67437, .T. ) ;
#28534 = CARTESIAN_POINT ( 'NONE',  ( 9.450000001229033941, -2.886751345948129988, 4.999999999999997335 ) ) ;
#28535 = CARTESIAN_POINT ( 'NONE',  ( 8.840625000614515727, -3.027376345333610441, -5.243569643749999898 ) ) ;
#28536 = CARTESIAN_POINT ( 'NONE',  ( 8.324999999999999289, 4.330127018922191873, 2.499999999999999556 ) ) ;
#28537 = CARTESIAN_POINT ( 'NONE',  ( 16.01250000122903216, 4.330127018922192761, -2.499999999999997780 ) ) ;
#28539 = CARTESIAN_POINT ( 'NONE',  ( -2.121784821874996840, 13.63437500061451857, -26.32496088578401583 ) ) ;
#28538 = VECTOR ( 'NONE', #18191, 1000.000000000000000 ) ;
#28540 = CARTESIAN_POINT ( 'NONE',  ( 28.35000000122903430, -2.886751345948129988, 4.999999999999997335 ) ) ;
#28541 = CARTESIAN_POINT ( 'NONE',  ( -3.756430356250000990, 16.95312499938548356, 32.16877607737301048 ) ) ;
#28542 = CARTESIAN_POINT ( 'NONE',  ( 6.975000000000002309, 4.330127018922191873, 2.499999999999999556 ) ) ;
#28543 = CARTESIAN_POINT ( 'NONE',  ( 30.00000000000000000, 0.000000000000000000, 4.999999999999998224 ) ) ;
#28544 = ORIENTED_EDGE ( 'NONE', *, *, #40932, .T. ) ;
#28545 = CARTESIAN_POINT ( 'NONE',  ( 20.72812500061451502, 4.541064518000418104, 2.621784821874999949 ) ) ;
#28546 = CARTESIAN_POINT ( 'NONE',  ( 13.12500000122903288, -5.773502691896255534, -1.060575238724906372E-15 ) ) ;
#28547 = CARTESIAN_POINT ( 'NONE',  ( 28.49062500061451431, -3.027376345333614438, 5.243569643749998122 ) ) ;
#28548 = FACE_OUTER_BOUND ( 'NONE', #6100, .T. ) ;
#28549 = CARTESIAN_POINT ( 'NONE',  ( 20.07187500061451857, -6.054752690667223547, -1.112240025338166033E-15 ) ) ;
#28550 = CARTESIAN_POINT ( 'NONE',  ( 17.50312500061451715, 4.541064518000418104, -2.621784821874998173 ) ) ;
#28551 = CARTESIAN_POINT ( 'NONE',  ( -2.121784821874999949, 12.52812500061459211, -33.67503911421598417 ) ) ;
#28552 = CARTESIAN_POINT ( 'NONE',  ( 5.803125000614517859, 4.541064518000418104, -2.621784821874998173 ) ) ;
#28553 = CARTESIAN_POINT ( 'NONE',  ( 29.02500000122903145, 2.886751345948129099, -4.999999999999998224 ) ) ;
#28554 = CARTESIAN_POINT ( 'NONE',  ( 22.65937500061451715, 0.000000000000000000, 4.756430356249998326 ) ) ;
#28555 = CARTESIAN_POINT ( 'NONE',  ( 19.30312500061451786, 4.541064518000418104, -2.621784821874998173 ) ) ;
#28556 = CARTESIAN_POINT ( 'NONE',  ( 1.999999999999998668, 14.00000000000000178, 26.53589838486224650 ) ) ;
#28557 = CARTESIAN_POINT ( 'NONE',  ( 3.562500001229033764, 0.000000000000000000, 4.999999999999998224 ) ) ;
#28558 = CARTESIAN_POINT ( 'NONE',  ( 12.53437500061451537, 6.421520780324663323E-16, -5.243569643749999010 ) ) ;
#28559 = CARTESIAN_POINT ( 'NONE',  ( 11.48437500061451644, -4.541064518000419881, 2.621784821874995952 ) ) ;
#28560 = CARTESIAN_POINT ( 'NONE',  ( 19.43437500061451928, 4.541064518000418104, 2.621784821874999949 ) ) ;
#28561 = ORIENTED_EDGE ( 'NONE', *, *, #32854, .F. ) ;
#28562 = CARTESIAN_POINT ( 'NONE',  ( 27.29999999999999716, 0.000000000000000000, 4.999999999999998224 ) ) ;
#28563 = CARTESIAN_POINT ( 'NONE',  ( 24.70312500061451644, 4.541064518000418104, -2.621784821874998173 ) ) ;
#28564 = CARTESIAN_POINT ( 'NONE',  ( 19.02187500061451786, 3.027376345333611329, 5.243569643749999010 ) ) ;
#28565 = CARTESIAN_POINT ( 'NONE',  ( 25.07812500061451644, 6.421520780324663323E-16, -5.243569643749999010 ) ) ;
#28566 = CARTESIAN_POINT ( 'NONE',  ( -2.498395430326213790E-14, 17.05624999877096926, 26.00000000000000000 ) ) ;
#28567 = CARTESIAN_POINT ( 'NONE',  ( -3.999999999999999112, 16.40000000000000213, 30.00000000000000000 ) ) ;
#28568 = CARTESIAN_POINT ( 'NONE',  ( 4.471875000614518925, 3.027376345333613106, -5.243569643749998122 ) ) ;
#28569 = CARTESIAN_POINT ( 'NONE',  ( 12.37500000122903465, 2.886751345948129099, -4.999999999999998224 ) ) ;
#28570 = CARTESIAN_POINT ( 'NONE',  ( 7.725000001229034297, -5.773502691896255534, -1.060575238724906372E-15 ) ) ;
#28571 = CARTESIAN_POINT ( 'NONE',  ( 27.11250000122903359, -4.330127018922190985, -2.500000000000001332 ) ) ;
#28572 = CARTESIAN_POINT ( 'NONE',  ( -8.484601909799255319E-16, 17.73124999877096641, 34.61880215351700940 ) ) ;
#28573 = CARTESIAN_POINT ( 'NONE',  ( 16.33125000122903359, 6.123233995736764310E-16, -4.999999999999998224 ) ) ;
#28574 = CARTESIAN_POINT ( 'NONE',  ( 13.02187500061451608, 3.027376345333613106, -5.243569643749998122 ) ) ;
#28575 = FACE_OUTER_BOUND ( 'NONE', #38523, .T. ) ;
#28576 = CARTESIAN_POINT ( 'NONE',  ( 16.45312500061451289, -4.541064518000417216, -2.621784821875001281 ) ) ;
#28577 = CARTESIAN_POINT ( 'NONE',  ( 13.47187500061451537, 3.027376345333613106, -5.243569643749998122 ) ) ;
#28578 = CARTESIAN_POINT ( 'NONE',  ( 5.128125000614516260, -4.541064518000419881, 2.621784821874995952 ) ) ;
#28579 = CARTESIAN_POINT ( 'NONE',  ( 20.22187500061451715, 3.027376345333612662, -5.243569643749998122 ) ) ;
#28580 = CARTESIAN_POINT ( 'NONE',  ( 9.346875000614517148, -3.027376345333610441, -5.243569643749999898 ) ) ;
#28581 = CARTESIAN_POINT ( 'NONE',  ( 14.85000000122903252, -2.886751345948130876, 4.999999999999996447 ) ) ;
#28582 = CARTESIAN_POINT ( 'NONE',  ( -3.999999999999999112, 17.71249999999999858, 27.69059892324149885 ) ) ;
#28583 = CARTESIAN_POINT ( 'NONE',  ( 6.225000001229036073, 2.886751345948126879, 4.999999999999999112 ) ) ;
#28584 = CARTESIAN_POINT ( 'NONE',  ( 19.75312500061451360, 4.541064518000418104, -2.621784821874998173 ) ) ;
#28585 = ADVANCED_FACE ( 'NONE', ( #7271 ), #57140, .F. ) ;
#28586 = CARTESIAN_POINT ( 'NONE',  ( 8.212500001229035007, -4.330127018922190985, -2.500000000000001332 ) ) ;
#28587 = CARTESIAN_POINT ( 'NONE',  ( 17.01562500061451644, 3.027376345333613106, -5.243569643749998122 ) ) ;
#28588 = CARTESIAN_POINT ( 'NONE',  ( 14.16562500061451679, -6.054752690667223547, -1.112240025338166033E-15 ) ) ;
#28589 = CARTESIAN_POINT ( 'NONE',  ( 25.80937500061451928, 0.000000000000000000, 4.756430356249998326 ) ) ;
#28590 = CARTESIAN_POINT ( 'NONE',  ( 13.19999999999999929, 4.330127018922192761, -2.499999999999997780 ) ) ;
#28591 = CARTESIAN_POINT ( 'NONE',  ( 10.12500000122903465, 2.886751345948129099, -4.999999999999998224 ) ) ;
#28592 = CARTESIAN_POINT ( 'NONE',  ( 6.028125000614517504, -4.541064518000419881, 2.621784821874995952 ) ) ;
#28593 =( BOUNDED_CURVE ( )  B_SPLINE_CURVE ( 2, ( #46137, #47223, #6974, #36134, #8060, #41324, #69754 ),
 .UNSPECIFIED., .F., .F. ) 
 B_SPLINE_CURVE_WITH_KNOTS ( ( 3, 2, 2, 3 ),
 ( 0.6199999999999999956, 0.6233333333333332948, 0.6266666666666667052, 0.6300000000000000044 ),
 .UNSPECIFIED. ) 
 CURVE ( )  GEOMETRIC_REPRESENTATION_ITEM ( )  RATIONAL_B_SPLINE_CURVE ( ( 1.000000000000000000, 0.8660254037844387076, 1.000000000000000000, 0.8660254037844387076, 1.000000000000000000, 0.8660254037844387076, 1.000000000000000000 ) ) 
 REPRESENTATION_ITEM ( '' )  );
#28594 = CARTESIAN_POINT ( 'NONE',  ( 18.03750000122903430, -4.330127018922194537, 2.499999999999995559 ) ) ;
#28595 = CARTESIAN_POINT ( 'NONE',  ( 27.67499999999999716, 4.330127018922191873, 2.499999999999999556 ) ) ;
#28596 = CARTESIAN_POINT ( 'NONE',  ( -3.000416591977282496E-16, 10.29687500061451644, -34.90005215228797653 ) ) ;
#28597 = CARTESIAN_POINT ( 'NONE',  ( 4.530078317929211451, -2.116641477924516401, 4.600875075901697642 ) ) ;
#28598 = CARTESIAN_POINT ( 'NONE',  ( 30.00000000000000000, 0.000000000000000000, 0.000000000000000000 ) ) ;
#28599 = CARTESIAN_POINT ( 'NONE',  ( 2.859375000614519546, 0.000000000000000000, 5.243569643749999010 ) ) ;
#28600 = CARTESIAN_POINT ( 'NONE',  ( 21.04687500061451644, -3.027376345333610441, -5.243569643749999898 ) ) ;
#28601 = CARTESIAN_POINT ( 'NONE',  ( 10.68750000122903288, 4.330127018922191873, 2.499999999999999556 ) ) ;
#28602 = CARTESIAN_POINT ( 'NONE',  ( 17.05312500061451786, 4.541064518000418104, -2.621784821874998173 ) ) ;
#28603 = CARTESIAN_POINT ( 'NONE',  ( 11.60625000122903216, 0.000000000000000000, 4.999999999999998224 ) ) ;
#28604 = CARTESIAN_POINT ( 'NONE',  ( -3.999999999999999112, 15.46250000000000036, -32.30940107675850470 ) ) ;
#28605 = CARTESIAN_POINT ( 'NONE',  ( -1.999999999999997113, 15.57500000000000284, 33.46410161513775705 ) ) ;
#28606 = CARTESIAN_POINT ( 'NONE',  ( 27.45937500061451786, 4.541064518000418104, -2.621784821874998173 ) ) ;
#28607 = CARTESIAN_POINT ( 'NONE',  ( 17.78437500061451360, -2.746126346562641984, -4.756430356249999214 ) ) ;
#28608 = CARTESIAN_POINT ( 'NONE',  ( 12.25312500061451537, 0.000000000000000000, 5.243569643749999010 ) ) ;
#28609 = CARTESIAN_POINT ( 'NONE',  ( 11.44687500061451857, -3.027376345333614438, 5.243569643749998122 ) ) ;
#28610 = ORIENTED_EDGE ( 'NONE', *, *, #40314, .F. ) ;
#28611 = CARTESIAN_POINT ( 'NONE',  ( 19.26562500061451644, 3.027376345333613106, -5.243569643749998122 ) ) ;
#28612 = CARTESIAN_POINT ( 'NONE',  ( 3.242103837493086330E-14, 11.00000000122903288, -34.00000000000000000 ) ) ;
#28613 = CARTESIAN_POINT ( 'NONE',  ( 20.99999999999999645, 0.000000000000000000, 4.999999999999998224 ) ) ;
#28614 = CARTESIAN_POINT ( 'NONE',  ( 12.44999999999999929, 0.000000000000000000, 4.999999999999998224 ) ) ;
#28615 = CARTESIAN_POINT ( 'NONE',  ( 22.27500000122903145, 2.886751345948129099, -4.999999999999998224 ) ) ;
#28616 = CARTESIAN_POINT ( 'NONE',  ( 15.59062500061451573, -3.027376345333610441, -5.243569643749999898 ) ) ;
#28617 = CARTESIAN_POINT ( 'NONE',  ( 13.47187500061451715, 4.119189519843966529, 2.378215178124999607 ) ) ;
#28618 = ORIENTED_EDGE ( 'NONE', *, *, #24132, .T. ) ;
#28619 = CARTESIAN_POINT ( 'NONE',  ( 20.32499999999999929, 6.123233995736764310E-16, -4.999999999999998224 ) ) ;
#28620 = CARTESIAN_POINT ( 'NONE',  ( 23.47499999999999787, 6.123233995736764310E-16, -4.999999999999998224 ) ) ;
#28621 = CARTESIAN_POINT ( 'NONE',  ( 20.52187500061451786, -6.054752690667223547, -1.112240025338166033E-15 ) ) ;
#28622 = CARTESIAN_POINT ( 'NONE',  ( 25.97812500061451502, 6.421520780324663323E-16, -5.243569643749999010 ) ) ;
#28623 = ORIENTED_EDGE ( 'NONE', *, *, #40237, .T. ) ;
#28624 = CARTESIAN_POINT ( 'NONE',  ( 13.79999999999999893, 0.000000000000000000, 4.999999999999998224 ) ) ;
#28625 = CARTESIAN_POINT ( 'NONE',  ( 9.290625000614515017, -3.027376345333610441, -5.243569643749999898 ) ) ;
#28626 = CARTESIAN_POINT ( 'NONE',  ( 12.22499999999999964, 6.123233995736764310E-16, -4.999999999999998224 ) ) ;
#28627 = CARTESIAN_POINT ( 'NONE',  ( 15.63749999999999751, -2.886751345948129988, 4.999999999999997335 ) ) ;
#28628 = CARTESIAN_POINT ( 'NONE',  ( -2.121784821874996840, 18.07812500061451644, 33.67503911421598417 ) ) ;
#28629 = CARTESIAN_POINT ( 'NONE',  ( 29.24062500061451431, 6.054752690667223547, 3.707466751127219781E-16 ) ) ;
#28630 = CARTESIAN_POINT ( 'NONE',  ( 26.44687500061451502, -3.027376345333610441, -5.243569643749999898 ) ) ;
#28631 = VERTEX_POINT ( 'NONE', #17971 ) ;
#28632 = CARTESIAN_POINT ( 'NONE',  ( 22.94062500061451715, 6.054752690667223547, 3.707466751127219781E-16 ) ) ;
#28633 = CARTESIAN_POINT ( 'NONE',  ( 24.83437500061451431, 4.541064518000418104, 2.621784821874999949 ) ) ;
#28634 = CARTESIAN_POINT ( 'NONE',  ( -2.121784821874999949, 18.37812500061459531, -33.67503911421598417 ) ) ;
#28635 = CARTESIAN_POINT ( 'NONE',  ( 12.41249999999999964, 2.886751345948126879, 4.999999999999999112 ) ) ;
#28636 = CARTESIAN_POINT ( 'NONE',  ( 8.953125000614518214, 4.541064518000418104, -2.621784821874998173 ) ) ;
#28637 = CARTESIAN_POINT ( 'NONE',  ( 3.739591918817028127, 3.929519787406462239, -3.193872078864750996 ) ) ;
#28638 = CARTESIAN_POINT ( 'NONE',  ( 3.999999999999999112, 11.22500000000000142, 30.00000000000000000 ) ) ;
#28639 = CARTESIAN_POINT ( 'NONE',  ( 26.39062500061451644, -3.027376345333610441, -5.243569643749999898 ) ) ;
#28640 = CARTESIAN_POINT ( 'NONE',  ( 22.48125000122903216, -4.330127018922194537, 2.499999999999995559 ) ) ;
#28641 = CARTESIAN_POINT ( 'NONE',  ( 12.94687500061451857, -2.746126346562642428, -4.756430356249999214 ) ) ;
#28642 = CARTESIAN_POINT ( 'NONE',  ( 18.49687500061452283, 6.054752690667223547, 3.707466751127219781E-16 ) ) ;
#28643 = CARTESIAN_POINT ( 'NONE',  ( 4.243569643749999898, 14.23437500061451821, 30.00000000000000000 ) ) ;
#28644 = CARTESIAN_POINT ( 'NONE',  ( 18.87187500061451573, 3.027376345333613106, -5.243569643749998122 ) ) ;
#28645 = CARTESIAN_POINT ( 'NONE',  ( 28.24687500061451573, -3.027376345333610441, -5.243569643749999898 ) ) ;
#28646 = CARTESIAN_POINT ( 'NONE',  ( 2.121784821875001281, 17.75937500061451502, 33.67503911421598417 ) ) ;
#28647 = CARTESIAN_POINT ( 'NONE',  ( 9.290625000614515017, -3.027376345333610441, -5.243569643749999898 ) ) ;
#28648 = CARTESIAN_POINT ( 'NONE',  ( 4.000000000000000000, 17.15000000122903145, 32.30940107675849760 ) ) ;
#28649 = CARTESIAN_POINT ( 'NONE',  ( 4.396875000614516971, -3.027376345333610441, -5.243569643749999898 ) ) ;
#28650 = LINE ( 'NONE', #62982, #14764 ) ;
#28651 = CARTESIAN_POINT ( 'NONE',  ( 7.903125000614515727, -4.541064518000417216, -2.621784821875001281 ) ) ;
#28652 = CARTESIAN_POINT ( 'NONE',  ( 11.33437500061451608, 4.541064518000418104, 2.621784821874999949 ) ) ;
#28653 =( NAMED_UNIT ( * ) PLANE_ANGLE_UNIT ( ) SI_UNIT ( $, .RADIAN. ) );
#28654 = CARTESIAN_POINT ( 'NONE',  ( 20.13750000122903216, 4.330127018922191873, 2.499999999999999556 ) ) ;
#28655 = CARTESIAN_POINT ( 'NONE',  ( 5.934375000614517504, 4.541064518000418104, 2.621784821874999949 ) ) ;
#28656 = CARTESIAN_POINT ( 'NONE',  ( 7.378125000614518036, -4.541064518000419881, 2.621784821874995952 ) ) ;
#28657 = CARTESIAN_POINT ( 'NONE',  ( 5.653125000614517504, -4.541064518000417216, -2.621784821875001281 ) ) ;
#28658 = CARTESIAN_POINT ( 'NONE',  ( 22.44375000122903074, -2.886751345948129988, 4.999999999999997335 ) ) ;
#28659 = CARTESIAN_POINT ( 'NONE',  ( 17.97187500061451715, 3.027376345333613106, -5.243569643749998122 ) ) ;
#28660 = CARTESIAN_POINT ( 'NONE',  ( 8.962500001229033231, 0.000000000000000000, 4.999999999999998224 ) ) ;
#28661 = ORIENTED_EDGE ( 'NONE', *, *, #65329, .F. ) ;
#28662 = CARTESIAN_POINT ( 'NONE',  ( 25.56562500061452070, 3.027376345333613106, -5.243569643749998122 ) ) ;
#28663 = CARTESIAN_POINT ( 'NONE',  ( 12.10312500061451857, 4.541064518000418104, -2.621784821874998173 ) ) ;
#28664 = CARTESIAN_POINT ( 'NONE',  ( 29.52187500061451431, -6.054752690667223547, -1.112240025338166033E-15 ) ) ;
#28665 = CARTESIAN_POINT ( 'NONE',  ( 12.06562500061451537, 3.027376345333613106, -5.243569643749998122 ) ) ;
#28666 = DIRECTION ( 'NONE',  ( 0.000000000000000000, 0.000000000000000000, -1.000000000000000000 ) ) ;
#28667 = CARTESIAN_POINT ( 'NONE',  ( 11.85000000122903430, -2.886751345948125991, -5.000000000000000000 ) ) ;
#28668 = CARTESIAN_POINT ( 'NONE',  ( 27.51562500061451644, 3.027376345333611329, 5.243569643749999010 ) ) ;
#28669 = EDGE_CURVE ( 'NONE', #23627, #11718, #50048, .T. ) ;
#28670 = CARTESIAN_POINT ( 'NONE',  ( -4.243569643749999898, 12.15312500061451573, -30.00000000000000000 ) ) ;
#28671 = CARTESIAN_POINT ( 'NONE',  ( 15.90000000122903501, -2.886751345948125991, -5.000000000000000000 ) ) ;
#28672 = CARTESIAN_POINT ( 'NONE',  ( 11.92500000000000071, 4.330127018922191873, 2.499999999999999556 ) ) ;
#28673 = CARTESIAN_POINT ( 'NONE',  ( 19.86562500061451786, 3.027376345333611329, 5.243569643749999010 ) ) ;
#28674 = CARTESIAN_POINT ( 'NONE',  ( 8.859375000614518214, -4.541064518000417216, -2.621784821875001281 ) ) ;
#28675 = CARTESIAN_POINT ( 'NONE',  ( 8.325000001229033941, 2.886751345948129099, -4.999999999999998224 ) ) ;
#28676 = CARTESIAN_POINT ( 'NONE',  ( 17.36250000122903359, 4.330127018922192761, -2.499999999999997780 ) ) ;
#28677 = CARTESIAN_POINT ( 'NONE',  ( 12.55312500061451786, 4.541064518000418104, -2.621784821874998173 ) ) ;
#28678 = CARTESIAN_POINT ( 'NONE',  ( 15.89062500061451289, -3.027376345333614438, 5.243569643749998122 ) ) ;
#28679 = CARTESIAN_POINT ( 'NONE',  ( 26.77500000122903145, 2.886751345948129099, -4.999999999999998224 ) ) ;
#28680 = CARTESIAN_POINT ( 'NONE',  ( 23.51249999999999574, 2.886751345948129099, -4.999999999999998224 ) ) ;
#28681 = CARTESIAN_POINT ( 'NONE',  ( 24.38437500061451502, 4.541064518000418104, 2.621784821874999949 ) ) ;
#28682 = CARTESIAN_POINT ( 'NONE',  ( 3.999999999999998668, 13.81250000000000000, 32.30940107675850470 ) ) ;
#28683 = PRODUCT_RELATED_PRODUCT_CATEGORY ( 'part', '', ( #23145 ) ) ;
#28684 = CARTESIAN_POINT ( 'NONE',  ( 10.65000000122903323, 5.773502691896255534, 3.535250795749688894E-16 ) ) ;
#28685 = CARTESIAN_POINT ( 'NONE',  ( 27.90937500061451715, 4.541064518000418104, -2.621784821874998173 ) ) ;
#28686 = CARTESIAN_POINT ( 'NONE',  ( 3.271875000614519635, 3.027376345333611329, 5.243569643749999010 ) ) ;
#28687 = CARTESIAN_POINT ( 'NONE',  ( 23.31562500061451715, 3.027376345333613106, -5.243569643749998122 ) ) ;
#28688 = CARTESIAN_POINT ( 'NONE',  ( 1.878215178125000495, 13.72812499938548392, 26.74683588394047007 ) ) ;
#28689 = CARTESIAN_POINT ( 'NONE',  ( 4.411272977760241965, 2.353862934769528348, -4.685547128476531320 ) ) ;
#28690 = CARTESIAN_POINT ( 'NONE',  ( 6.984375000614516438, -4.541064518000419881, 2.621784821874995952 ) ) ;
#28691 = CARTESIAN_POINT ( 'NONE',  ( -5.810221930991193690E-16, 10.43750000000000000, 26.00000000000000355 ) ) ;
#28692 = CARTESIAN_POINT ( 'NONE',  ( 26.42812500061451431, 6.421520780324663323E-16, -5.243569643749999010 ) ) ;
#28693 = CARTESIAN_POINT ( 'NONE',  ( 6.346875000614517148, 6.054752690667223547, 3.707466751127219781E-16 ) ) ;
#28694 = CARTESIAN_POINT ( 'NONE',  ( 50.00000000000000000, 7.332543590861156702, 5.218601775200032655 ) ) ;
#28695 = CARTESIAN_POINT ( 'NONE',  ( 25.58437500061451431, 6.421520780324663323E-16, -5.243569643749999010 ) ) ;
#28696 = CARTESIAN_POINT ( 'NONE',  ( -0.7368881354385758975, 9.803648613939513368, 25.82089971438751519 ) ) ;
#28697 = CARTESIAN_POINT ( 'NONE',  ( 20.02500000000000213, 4.330127018922191873, 2.499999999999999556 ) ) ;
#28698 = VERTEX_POINT ( 'NONE', #7626 ) ;
#28699 = CARTESIAN_POINT ( 'NONE',  ( 27.18750000000000000, 5.773502691896255534, 3.535250795749688894E-16 ) ) ;
#28700 = CARTESIAN_POINT ( 'NONE',  ( 28.13437500061451502, -4.541064518000419881, 2.621784821874995952 ) ) ;
#28701 = ADVANCED_FACE ( 'NONE', ( #40532 ), #34981, .T. ) ;
#28702 = EDGE_LOOP ( 'NONE', ( #47065, #53365, #32443, #43587 ) ) ;
#28703 = CARTESIAN_POINT ( 'NONE',  ( 15.51562500061451644, -6.054752690667223547, -1.112240025338166033E-15 ) ) ;
#28704 = CARTESIAN_POINT ( 'NONE',  ( 7.528125000614515727, 6.421520780324663323E-16, -5.243569643749999010 ) ) ;
#28705 = CARTESIAN_POINT ( 'NONE',  ( 18.60937500061451289, -5.492252693125287522, -1.008910452111647106E-15 ) ) ;
#28706 = CARTESIAN_POINT ( 'NONE',  ( 5.671875000614519102, -6.054752690667223547, -1.112240025338166033E-15 ) ) ;
#28707 = CARTESIAN_POINT ( 'NONE',  ( 16.80000000122903359, -2.886751345948125991, -5.000000000000000000 ) ) ;
#28708 = CARTESIAN_POINT ( 'NONE',  ( 21.93750000000000000, -2.886751345948129988, 4.999999999999997335 ) ) ;
#28709 = CARTESIAN_POINT ( 'NONE',  ( 29.47499999999999787, 4.330127018922191873, 2.499999999999999556 ) ) ;
#28710 = CARTESIAN_POINT ( 'NONE',  ( 5.709375000614517859, -4.541064518000417216, -2.621784821875001281 ) ) ;
#28711 = CARTESIAN_POINT ( 'NONE',  ( 10.58437500061451964, -4.541064518000419881, 2.621784821874995952 ) ) ;
#28712 = CARTESIAN_POINT ( 'NONE',  ( 21.15937500061451715, 4.541064518000418104, -2.621784821874998173 ) ) ;
#28713 = CARTESIAN_POINT ( 'NONE',  ( 1.592000809091587073E-14, 15.05000000122903714, -34.00000000000000000 ) ) ;
#28714 = EDGE_LOOP ( 'NONE', ( #15353, #43314, #10766, #57691 ) ) ;
#28715 = CARTESIAN_POINT ( 'NONE',  ( 4.434375000614519280, 6.421520780324663323E-16, -5.243569643749999010 ) ) ;
#28716 = CARTESIAN_POINT ( 'NONE',  ( 8.109375000614518214, 4.541064518000418104, -2.621784821874998173 ) ) ;
#28717 = CARTESIAN_POINT ( 'NONE',  ( 17.84999999999999787, 0.000000000000000000, 4.999999999999998224 ) ) ;
#28718 = CARTESIAN_POINT ( 'NONE',  ( 15.21562500061451750, 3.027376345333613106, -5.243569643749998122 ) ) ;
#28719 = CARTESIAN_POINT ( 'NONE',  ( -8.484601909799255319E-16, 19.13750000000000284, 34.61880215351700940 ) ) ;
#28720 = CARTESIAN_POINT ( 'NONE',  ( 20.10937500061451289, -4.119189519843965641, -2.378215178125001383 ) ) ;
#28721 = CARTESIAN_POINT ( 'NONE',  ( 10.86562500061451431, 3.027376345333611329, 5.243569643749999010 ) ) ;
#28722 = CARTESIAN_POINT ( 'NONE',  ( 25.69687500061451502, 6.054752690667223547, 3.707466751127219781E-16 ) ) ;
#28723 = CARTESIAN_POINT ( 'NONE',  ( 28.40625000122903288, -4.330127018922190985, -2.500000000000001332 ) ) ;
#28724 = CARTESIAN_POINT ( 'NONE',  ( 26.18437500061451573, 4.541064518000418104, 2.621784821874999949 ) ) ;
#28725 = CARTESIAN_POINT ( 'NONE',  ( 8.925000000000002487, -4.330127018922194537, 2.499999999999995559 ) ) ;
#28726 = CARTESIAN_POINT ( 'NONE',  ( -3.999999999999997335, 16.10000000122903430, 32.30940107675850470 ) ) ;
#28727 = CARTESIAN_POINT ( 'NONE',  ( 8.100000001229034297, -2.886751345948129988, 4.999999999999997335 ) ) ;
#28728 = CARTESIAN_POINT ( 'NONE',  ( 19.47187500061451360, 3.027376345333611329, 5.243569643749999010 ) ) ;
#28729 = CARTESIAN_POINT ( 'NONE',  ( 13.95937500061451786, 4.541064518000418104, -2.621784821874998173 ) ) ;
#28730 = CARTESIAN_POINT ( 'NONE',  ( -0.2805529113108836126, 4.994030452822313393, -33.99254504240288099 ) ) ;
#28731 = VERTEX_POINT ( 'NONE', #46800 ) ;
#28732 = CARTESIAN_POINT ( 'NONE',  ( 15.81562500061451537, 3.027376345333611329, 5.243569643749999010 ) ) ;
#28733 = CARTESIAN_POINT ( 'NONE',  ( 25.95000000122903216, 5.773502691896255534, 3.535250795749688894E-16 ) ) ;
#28734 = CARTESIAN_POINT ( 'NONE',  ( 12.83437500061451786, -4.541064518000419881, 2.621784821874995952 ) ) ;
#28735 = CARTESIAN_POINT ( 'NONE',  ( 0.000000000000000000, 10.00000000000000000, -36.00000000000000000 ) ) ;
#28736 = CARTESIAN_POINT ( 'NONE',  ( 16.34062500061451573, -3.027376345333614438, 5.243569643749998122 ) ) ;
#28737 = EDGE_CURVE ( 'NONE', #45391, #52475, #54686, .T. ) ;
#28738 = CARTESIAN_POINT ( 'NONE',  ( 45.00000000000000000, 6.123233995736764310E-16, -4.999999999999998224 ) ) ;
#28739 = CARTESIAN_POINT ( 'NONE',  ( 25.17187500061451644, 3.027376345333613106, -5.243569643749998122 ) ) ;
#28740 = CARTESIAN_POINT ( 'NONE',  ( 4.243569643749999898, 11.02812500061451750, 30.00000000000000000 ) ) ;
#28741 = CARTESIAN_POINT ( 'NONE',  ( 16.17187500061451644, 3.027376345333613106, -5.243569643749998122 ) ) ;
#28742 = CARTESIAN_POINT ( 'NONE',  ( 12.86250000122903359, 4.330127018922192761, -2.499999999999997780 ) ) ;
#28743 = CYLINDRICAL_SURFACE ( 'NONE', #55157, 4.999999999999998224 ) ;
#28744 = CARTESIAN_POINT ( 'NONE',  ( -3.000416591977282496E-16, 17.94687500061451502, -34.90005215228797653 ) ) ;
#28745 =( BOUNDED_CURVE ( )  B_SPLINE_CURVE ( 2, ( #30681, #65763, #37682, #60205, #9617, #14783, #32149, #3357, #59848 ),
 .UNSPECIFIED., .F., .F. ) 
 B_SPLINE_CURVE_WITH_KNOTS ( ( 3, 2, 2, 2, 3 ),
 ( 0.7934782608695651884, 0.7971014492753623060, 0.8043478260869565410, 0.8115942028985507761, 0.8152173913043478937 ),
 .UNSPECIFIED. ) 
 CURVE ( )  GEOMETRIC_REPRESENTATION_ITEM ( )  RATIONAL_B_SPLINE_CURVE ( ( 0.9330127018922194093, 0.9330127018922194093, 1.000000000000000000, 0.8660254037844387076, 1.000000000000000000, 0.8660254037844387076, 1.000000000000000000, 0.9330127018922182991, 0.9330127018922192983 ) ) 
 REPRESENTATION_ITEM ( '' )  );
#28746 = CARTESIAN_POINT ( 'NONE',  ( 17.48437500061451999, 6.421520780324663323E-16, -5.243569643749999010 ) ) ;
#28747 = CARTESIAN_POINT ( 'NONE',  ( 20.85000000122903430, -2.886751345948125991, -5.000000000000000000 ) ) ;
#28748 = CARTESIAN_POINT ( 'NONE',  ( 14.78437500061451715, 6.421520780324663323E-16, -5.243569643749999010 ) ) ;
#28749 = CARTESIAN_POINT ( 'NONE',  ( 4.243569643749999010, 12.02187500061451786, 27.54997392385601174 ) ) ;
#28750 = CARTESIAN_POINT ( 'NONE',  ( 21.48750000122903003, 4.330127018922191873, 2.499999999999999556 ) ) ;
#28751 = CARTESIAN_POINT ( 'NONE',  ( 14.27812500061451573, 6.421520780324663323E-16, -5.243569643749999010 ) ) ;
#28752 = CARTESIAN_POINT ( 'NONE',  ( 29.69062500061451715, 6.054752690667223547, 3.707466751127219781E-16 ) ) ;
#28753 = VERTEX_POINT ( 'NONE', #1738 ) ;
#28754 = ORIENTED_EDGE ( 'NONE', *, *, #23389, .T. ) ;
#28755 = CARTESIAN_POINT ( 'NONE',  ( 21.15000000000000213, -4.330127018922190985, -2.500000000000001332 ) ) ;
#28756 = DIRECTION ( 'NONE',  ( -1.000000000000000000, -0.000000000000000000, -0.000000000000000000 ) ) ;
#28757 = CARTESIAN_POINT ( 'NONE',  ( 3.665625000614517681, 3.027376345333611329, 5.243569643749999010 ) ) ;
#28758 = CARTESIAN_POINT ( 'NONE',  ( 13.87500000122903465, 2.886751345948126879, 4.999999999999999112 ) ) ;
#28759 = CARTESIAN_POINT ( 'NONE',  ( 20.35312500061451502, 0.000000000000000000, 5.243569643749999010 ) ) ;
#28760 = CARTESIAN_POINT ( 'NONE',  ( 23.65312500061451573, -4.541064518000417216, -2.621784821875001281 ) ) ;
#28761 = EDGE_CURVE ( 'NONE', #53784, #58713, #24252, .T. ) ;
#28762 = CARTESIAN_POINT ( 'NONE',  ( 4.490625000614516971, 6.054752690667223547, 3.707466751127219781E-16 ) ) ;
#28763 = CARTESIAN_POINT ( 'NONE',  ( 28.98750000000000071, 5.773502691896255534, 3.535250795749688894E-16 ) ) ;
#28764 = CARTESIAN_POINT ( 'NONE',  ( 4.779258346327469376, 1.469247991000700582, 4.779258346327429408 ) ) ;
#28765 = CARTESIAN_POINT ( 'NONE',  ( 9.421875000614519990, 2.746126346562645981, -4.756430356249997438 ) ) ;
#28766 = CARTESIAN_POINT ( 'NONE',  ( 29.55937500061451573, -4.541064518000417216, -2.621784821875001281 ) ) ;
#28767 = CARTESIAN_POINT ( 'NONE',  ( -3.999999999999997335, 11.60000000122903430, -27.69059892324149175 ) ) ;
#28768 = CARTESIAN_POINT ( 'NONE',  ( 4.243569643749999898, 18.28437500061451715, -30.00000000000000000 ) ) ;
#28769 = CARTESIAN_POINT ( 'NONE',  ( 5.775000001229033231, 2.886751345948126879, 4.999999999999999112 ) ) ;
#28770 = CARTESIAN_POINT ( 'NONE',  ( 7.650000000000000355, -4.330127018922190985, -2.500000000000001332 ) ) ;
#28771 = CARTESIAN_POINT ( 'NONE',  ( 5.175000001229033586, 2.886751345948129099, -4.999999999999998224 ) ) ;
#28772 = CARTESIAN_POINT ( 'NONE',  ( 11.10937500061451644, -4.541064518000417216, -2.621784821875001281 ) ) ;
#28773 = DIRECTION ( 'NONE',  ( 1.000000000000000000, -0.000000000000000000, -0.000000000000000000 ) ) ;
#28774 = CARTESIAN_POINT ( 'NONE',  ( 4.659375000614518925, 0.000000000000000000, 5.243569643749999010 ) ) ;
#28775 = CARTESIAN_POINT ( 'NONE',  ( 1.071796769724490783, 19.07990381179670081, 26.00000000000000355 ) ) ;
#28776 = CARTESIAN_POINT ( 'NONE',  ( 29.66250000122903074, 0.000000000000000000, 4.999999999999998224 ) ) ;
#28777 = CARTESIAN_POINT ( 'NONE',  ( 11.07187500061451679, -6.054752690667223547, -1.112240025338166033E-15 ) ) ;
#28778 = CARTESIAN_POINT ( 'NONE',  ( 14.78437500061451715, 6.421520780324663323E-16, -5.243569643749999010 ) ) ;
#28779 = CARTESIAN_POINT ( 'NONE',  ( -2.000000000000000000, 18.57500000000000284, -33.46410161513775705 ) ) ;
#28780 = CARTESIAN_POINT ( 'NONE',  ( 7.724999999999999645, 6.123233995736764310E-16, -4.999999999999998224 ) ) ;
#28781 =( BOUNDED_CURVE ( )  B_SPLINE_CURVE ( 2, ( #39882, #68315, #45780, #56843, #40968, #353, #69039, #22860, #17675 ),
 .UNSPECIFIED., .F., .F. ) 
 B_SPLINE_CURVE_WITH_KNOTS ( ( 3, 2, 2, 2, 3 ),
 ( 0.01086956521739130578, 0.01449275362318840597, 0.02173913043478260809, 0.02898550724637680848, 0.03260869565217391908 ),
 .UNSPECIFIED. ) 
 CURVE ( )  GEOMETRIC_REPRESENTATION_ITEM ( )  RATIONAL_B_SPLINE_CURVE ( ( 0.9330127018922194093, 0.9330127018922194093, 1.000000000000000000, 0.8660254037844387076, 1.000000000000000000, 0.8660254037844387076, 1.000000000000000000, 0.9330127018922191873, 0.9330127018922192983 ) ) 
 REPRESENTATION_ITEM ( '' )  );
#28782 = CARTESIAN_POINT ( 'NONE',  ( -3.000416591977282496E-16, 17.44062500061459176, 25.09994784771203058 ) ) ;
#28783 = CARTESIAN_POINT ( 'NONE',  ( 21.75937500061451502, 0.000000000000000000, 5.243569643749999010 ) ) ;
#28784 = CARTESIAN_POINT ( 'NONE',  ( 0.000000000000000000, 20.00000000000000000, -30.00000000000000000 ) ) ;
#28785 = CARTESIAN_POINT ( 'NONE',  ( 26.13750000122903216, -4.330127018922194537, 2.499999999999995559 ) ) ;
#28786 = CARTESIAN_POINT ( 'NONE',  ( 18.53437500061451360, -2.746126346562646425, 4.756430356249996549 ) ) ;
#28787 = CARTESIAN_POINT ( 'NONE',  ( 22.79062500061451502, -3.027376345333610441, -5.243569643749999898 ) ) ;
#28788 = CARTESIAN_POINT ( 'NONE',  ( 15.29062500061451679, 6.054752690667223547, 3.707466751127219781E-16 ) ) ;
#28789 = CARTESIAN_POINT ( 'NONE',  ( 26.63437500061451146, -2.746126346562646425, 4.756430356249996549 ) ) ;
#28790 = CARTESIAN_POINT ( 'NONE',  ( 12.12187500061451573, 3.027376345333613106, -5.243569643749998122 ) ) ;
#28791 = CARTESIAN_POINT ( 'NONE',  ( 28.23750000000000426, -2.886751345948129988, 4.999999999999997335 ) ) ;
#28792 = CARTESIAN_POINT ( 'NONE',  ( 24.60000000122903430, 5.773502691896255534, 3.535250795749688894E-16 ) ) ;
#28793 = CARTESIAN_POINT ( 'NONE',  ( 3.834375000614519635, -4.541064518000419881, 2.621784821874995952 ) ) ;
#28794 = CARTESIAN_POINT ( 'NONE',  ( 11.37187500061451750, 3.027376345333611329, 5.243569643749999010 ) ) ;
#28795 = CARTESIAN_POINT ( 'NONE',  ( 28.20937500061451786, -4.541064518000417216, -2.621784821875001281 ) ) ;
#28796 = CARTESIAN_POINT ( 'NONE',  ( 3.384375000614517237, -4.541064518000419881, 2.621784821874995952 ) ) ;
#28797 = LINE ( 'NONE', #16976, #38410 ) ;
#28798 = CARTESIAN_POINT ( 'NONE',  ( 21.94687500061451857, -3.027376345333610441, -5.243569643749999898 ) ) ;
#28799 = CARTESIAN_POINT ( 'NONE',  ( 13.32187500061451502, -6.054752690667223547, -1.112240025338166033E-15 ) ) ;
#28800 = CARTESIAN_POINT ( 'NONE',  ( -1.878215178124999163, 17.85312499938548214, 26.74683588394047007 ) ) ;
#28801 = CARTESIAN_POINT ( 'NONE',  ( 26.25000000000000000, 4.330127018922192761, -2.499999999999997780 ) ) ;
#28802 = CARTESIAN_POINT ( 'NONE',  ( 4.537500001229034297, -4.330127018922194537, 2.499999999999995559 ) ) ;
#28803 = CARTESIAN_POINT ( 'NONE',  ( 26.25937500061451857, 0.000000000000000000, 4.756430356249998326 ) ) ;
#28804 = CARTESIAN_POINT ( 'NONE',  ( 17.65312500061451573, 0.000000000000000000, 5.243569643749999010 ) ) ;
#28805 = CARTESIAN_POINT ( 'NONE',  ( 6.899999999999999467, 4.330127018922192761, -2.499999999999997780 ) ) ;
#28806 = EDGE_CURVE ( 'NONE', #41505, #27416, #3788, .T. ) ;
#28807 = CARTESIAN_POINT ( 'NONE',  ( 13.46250000122903323, 0.000000000000000000, 4.999999999999998224 ) ) ;
#28808 = CARTESIAN_POINT ( 'NONE',  ( 16.98750000000000426, -2.886751345948129988, 4.999999999999997335 ) ) ;
#28809 = CARTESIAN_POINT ( 'NONE',  ( 4.243569643749999898, 12.37812500061451715, 30.00000000000000000 ) ) ;
#28810 =( BOUNDED_CURVE ( )  B_SPLINE_CURVE ( 2, ( #35163, #28897, #57687, #34432, #28537, #5650, #68794 ),
 .UNSPECIFIED., .F., .F. ) 
 B_SPLINE_CURVE_WITH_KNOTS ( ( 3, 2, 2, 3 ),
 ( 0.5000000000000000000, 0.5027777777777777679, 0.5055555555555556468, 0.5083333333333334147 ),
 .UNSPECIFIED. ) 
 CURVE ( )  GEOMETRIC_REPRESENTATION_ITEM ( )  RATIONAL_B_SPLINE_CURVE ( ( 1.000000000000000000, 0.8660254037844387076, 1.000000000000000000, 0.8660254037844387076, 1.000000000000000000, 0.8660254037844333785, 1.000000000000005329 ) ) 
 REPRESENTATION_ITEM ( '' )  );
#28811 = CARTESIAN_POINT ( 'NONE',  ( -4.000000000000000888, 16.36250000000000071, 32.30940107675850470 ) ) ;
#28812 = CARTESIAN_POINT ( 'NONE',  ( 21.56250000122903288, 0.000000000000000000, 4.999999999999998224 ) ) ;
#28813 = CARTESIAN_POINT ( 'NONE',  ( 26.78437500061451360, -4.541064518000419881, 2.621784821874995952 ) ) ;
#28814 = ORIENTED_EDGE ( 'NONE', *, *, #15629, .F. ) ;
#28815 = CARTESIAN_POINT ( 'NONE',  ( 22.37812500061451360, 6.421520780324663323E-16, -5.243569643749999010 ) ) ;
#28816 = CARTESIAN_POINT ( 'NONE',  ( 22.20937500061451431, 0.000000000000000000, 5.243569643749999010 ) ) ;
#28817 = CARTESIAN_POINT ( 'NONE',  ( 4.650000000000001243, 4.330127018922192761, -2.499999999999997780 ) ) ;
#28818 = CARTESIAN_POINT ( 'NONE',  ( 6.628125000614517148, 6.421520780324663323E-16, -5.243569643749999010 ) ) ;
#28819 = CARTESIAN_POINT ( 'NONE',  ( 25.26562500061451289, 3.027376345333611329, 5.243569643749999010 ) ) ;
#28820 = CARTESIAN_POINT ( 'NONE',  ( 12.64687500061451608, 6.054752690667223547, 3.707466751127219781E-16 ) ) ;
#28821 = CARTESIAN_POINT ( 'NONE',  ( 15.68437500061451573, 6.421520780324663323E-16, -5.243569643749999010 ) ) ;
#28822 = CARTESIAN_POINT ( 'NONE',  ( 4.243569643749999010, 16.91562500061451502, 27.54997392385601174 ) ) ;
#28823 = CARTESIAN_POINT ( 'NONE',  ( 21.63750000122903572, -4.330127018922194537, 2.499999999999995559 ) ) ;
#28824 = CARTESIAN_POINT ( 'NONE',  ( 14.93437500061451750, 4.119189519843966529, 2.378215178124999607 ) ) ;
#28825 = CARTESIAN_POINT ( 'NONE',  ( 9.928125000614517859, 4.541064518000418104, 2.621784821874999949 ) ) ;
#28826 = CARTESIAN_POINT ( 'NONE',  ( 6.309375000614517504, 4.541064518000418104, -2.621784821874998173 ) ) ;
#28827 = CARTESIAN_POINT ( 'NONE',  ( 4.546875000614517326, 6.054752690667223547, 3.707466751127219781E-16 ) ) ;
#28828 = ORIENTED_EDGE ( 'NONE', *, *, #1636, .T. ) ;
#28829 = CARTESIAN_POINT ( 'NONE',  ( 26.40937500061451715, -4.541064518000417216, -2.621784821875001281 ) ) ;
#28830 = CARTESIAN_POINT ( 'NONE',  ( 17.54062500061451502, 6.054752690667223547, 3.707466751127219781E-16 ) ) ;
#28831 = CARTESIAN_POINT ( 'NONE',  ( 28.42500000122904069, -5.773502691896255534, -1.060575238724906372E-15 ) ) ;
#28832 = CARTESIAN_POINT ( 'NONE',  ( 28.07812500061451289, -4.541064518000419881, 2.621784821874995952 ) ) ;
#28833 = CARTESIAN_POINT ( 'NONE',  ( 20.78437500061451715, 4.541064518000418104, 2.621784821874999949 ) ) ;
#28834 = CARTESIAN_POINT ( 'NONE',  ( 16.71562500061451573, 3.027376345333611329, 5.243569643749999010 ) ) ;
#28835 = CARTESIAN_POINT ( 'NONE',  ( -2.121784821874999949, 18.88437500061451857, 26.32496088578401938 ) ) ;
#28836 =( BOUNDED_CURVE ( )  B_SPLINE_CURVE ( 2, ( #51922, #1319, #69992, #58164, #24556, #8301, #2396, #23828, #40477 ),
 .UNSPECIFIED., .F., .F. ) 
 B_SPLINE_CURVE_WITH_KNOTS ( ( 3, 2, 2, 2, 3 ),
 ( 0.9021739130434782705, 0.9057971014492753881, 0.9130434782608695121, 0.9202898550724637472, 0.9239130434782608647 ),
 .UNSPECIFIED. ) 
 CURVE ( )  GEOMETRIC_REPRESENTATION_ITEM ( )  RATIONAL_B_SPLINE_CURVE ( ( 0.9330127018922194093, 0.9330127018922194093, 1.000000000000000000, 0.8660254037844387076, 1.000000000000000000, 0.8660254037844387076, 1.000000000000000000, 0.9330127018922194093, 0.9330127018922194093 ) ) 
 REPRESENTATION_ITEM ( '' )  );
#28837 = CARTESIAN_POINT ( 'NONE',  ( 22.19062500061451715, -3.027376345333614438, 5.243569643749998122 ) ) ;
#28838 = CARTESIAN_POINT ( 'NONE',  ( 21.97500000000000142, -4.330127018922194537, 2.499999999999995559 ) ) ;
#28839 = ORIENTED_EDGE ( 'NONE', *, *, #28401, .F. ) ;
#28840 = CARTESIAN_POINT ( 'NONE',  ( 26.96249999999999858, -5.773502691896255534, -1.060575238724906372E-15 ) ) ;
#28841 = CARTESIAN_POINT ( 'NONE',  ( 1.999999999999998668, 13.10000000000000142, -33.46410161513775705 ) ) ;
#28842 = CARTESIAN_POINT ( 'NONE',  ( -7.967954043666661671E-16, 18.49062499938548143, 34.33755215474603517 ) ) ;
#28843 = CARTESIAN_POINT ( 'NONE',  ( 29.80312500061451431, 0.000000000000000000, 5.243569643749999010 ) ) ;
#28844 = CARTESIAN_POINT ( 'NONE',  ( 9.515625000614518214, 3.027376345333611329, 5.243569643749999010 ) ) ;
#28845 = CARTESIAN_POINT ( 'NONE',  ( 22.80000000122903359, 5.773502691896255534, 3.535250795749688894E-16 ) ) ;
#28846 = EDGE_CURVE ( 'NONE', #2372, #65643, #22119, .T. ) ;
#28847 = CARTESIAN_POINT ( 'NONE',  ( 27.74062500061451431, -3.027376345333610441, -5.243569643749999898 ) ) ;
#28848 = CARTESIAN_POINT ( 'NONE',  ( 26.69999999999999929, 4.330127018922192761, -2.499999999999997780 ) ) ;
#28849 = CARTESIAN_POINT ( 'NONE',  ( 4.000000000000000000, 18.05000000122903359, -27.69059892324149530 ) ) ;
#28850 = CARTESIAN_POINT ( 'NONE',  ( -0.7157356635157281488, 9.902086024390941432, -34.05916648805959568 ) ) ;
#28851 = CARTESIAN_POINT ( 'NONE',  ( 11.72812500061451857, 4.541064518000418104, 2.621784821874999949 ) ) ;
#28852 = ORIENTED_EDGE ( 'NONE', *, *, #58732, .T. ) ;
#28853 = CARTESIAN_POINT ( 'NONE',  ( 8.653125000614515727, 0.000000000000000000, 5.243569643749999010 ) ) ;
#28854 = CARTESIAN_POINT ( 'NONE',  ( 7.078125000614516438, 6.421520780324663323E-16, -5.243569643749999010 ) ) ;
#28855 = CARTESIAN_POINT ( 'NONE',  ( 15.38437500061451679, 4.119189519843966529, 2.378215178124999607 ) ) ;
#28856 = EDGE_CURVE ( 'NONE', #21346, #38296, #36764, .T. ) ;
#28857 = CYLINDRICAL_SURFACE ( 'NONE', #42037, 3.999999999999996447 ) ;
#28858 = CARTESIAN_POINT ( 'NONE',  ( 15.45000000000000107, 4.330127018922192761, -2.499999999999997780 ) ) ;
#28860 = CARTESIAN_POINT ( 'NONE',  ( 15.34687500061451537, 6.054752690667223547, 3.707466751127219781E-16 ) ) ;
#28859 = AXIS2_PLACEMENT_3D ( 'NONE', #7281, #24623, #7637 ) ;
#28861 = CARTESIAN_POINT ( 'NONE',  ( 10.31250000122903288, 0.000000000000000000, 4.999999999999998224 ) ) ;
#28862 = CARTESIAN_POINT ( 'NONE',  ( 18.38437500061451857, 6.421520780324663323E-16, -5.243569643749999010 ) ) ;
#28863 = CARTESIAN_POINT ( 'NONE',  ( 16.46249999999999503, 2.886751345948126879, 4.999999999999999112 ) ) ;
#28864 = CARTESIAN_POINT ( 'NONE',  ( 21.04687500061451644, -3.027376345333610441, -5.243569643749999898 ) ) ;
#28865 = CARTESIAN_POINT ( 'NONE',  ( 2.121784821875001281, 13.65312500061451750, -26.32496088578401938 ) ) ;
#28866 = CARTESIAN_POINT ( 'NONE',  ( 7.350000000000002309, 4.330127018922192761, -2.499999999999997780 ) ) ;
#28867 = CARTESIAN_POINT ( 'NONE',  ( 25.32187500061451502, -4.119189519843968306, 2.378215178124996054 ) ) ;
#28868 = CARTESIAN_POINT ( 'NONE',  ( 20.77500000000000213, 6.123233995736764310E-16, -4.999999999999998224 ) ) ;
#28869 = CARTESIAN_POINT ( 'NONE',  ( 27.17812500061451786, -4.541064518000419881, 2.621784821874995952 ) ) ;
#28870 = CARTESIAN_POINT ( 'NONE',  ( 5.175000001229032698, 2.886751345948062486, -5.000000000000113687 ) ) ;
#28871 = CARTESIAN_POINT ( 'NONE',  ( 29.18437500061451573, 6.421520780324663323E-16, -5.243569643749999010 ) ) ;
#28872 = ADVANCED_FACE ( 'NONE', ( #36068 ), #3560, .T. ) ;
#28873 = CARTESIAN_POINT ( 'NONE',  ( 23.96249999999999858, 2.886751345948129099, -4.999999999999998224 ) ) ;
#28874 = CARTESIAN_POINT ( 'NONE',  ( 6.740625000614516082, 6.054752690667223547, 3.707466751127219781E-16 ) ) ;
#28875 = CARTESIAN_POINT ( 'NONE',  ( 25.13437500061451857, 5.492252693125287522, 3.363034840372157021E-16 ) ) ;
#28876 = CARTESIAN_POINT ( 'NONE',  ( 18.79687500061451644, -3.027376345333610441, -5.243569643749999898 ) ) ;
#28877 = CARTESIAN_POINT ( 'NONE',  ( 12.19687500061451502, 0.000000000000000000, 4.756430356249998326 ) ) ;
#28878 = CARTESIAN_POINT ( 'NONE',  ( 5.053125000614517859, 0.000000000000000000, 5.243569643749999010 ) ) ;
#28879 = CARTESIAN_POINT ( 'NONE',  ( 10.43437500061451750, 4.541064518000418104, 2.621784821874999949 ) ) ;
#28880 = ORIENTED_EDGE ( 'NONE', *, *, #35886, .T. ) ;
#28881 = CARTESIAN_POINT ( 'NONE',  ( 21.12187500061451573, 3.027376345333613106, -5.243569643749998122 ) ) ;
#28882 = DIRECTION ( 'NONE',  ( -1.000000000000000000, -0.000000000000000000, -0.000000000000000000 ) ) ;
#28883 = CARTESIAN_POINT ( 'NONE',  ( 27.89999999999999858, -4.330127018922190985, -2.500000000000001332 ) ) ;
#28884 = ADVANCED_FACE ( 'NONE', ( #19422 ), #2452, .T. ) ;
#28885 = CARTESIAN_POINT ( 'NONE',  ( 3.262500000000001510, 2.886751345948129099, -4.999999999999998224 ) ) ;
#28886 = CARTESIAN_POINT ( 'NONE',  ( 45.00000000000000000, 6.123233995736764310E-16, -4.999999999999998224 ) ) ;
#28887 = CARTESIAN_POINT ( 'NONE',  ( 17.69999999999999929, 4.330127018922192761, -2.499999999999997780 ) ) ;
#28888 = ORIENTED_EDGE ( 'NONE', *, *, #34930, .T. ) ;
#28889 = CARTESIAN_POINT ( 'NONE',  ( 9.712500000000002132, 2.886751345948126879, 4.999999999999999112 ) ) ;
#28890 = CARTESIAN_POINT ( 'NONE',  ( 12.34687500061451537, -4.119189519843965641, -2.378215178125001383 ) ) ;
#28891 = CARTESIAN_POINT ( 'NONE',  ( 24.81562500061451715, 3.027376345333611329, 5.243569643749999010 ) ) ;
#28892 = CARTESIAN_POINT ( 'NONE',  ( 14.13750000000000107, 5.773502691896255534, 3.535250795749688894E-16 ) ) ;
#28893 = CARTESIAN_POINT ( 'NONE',  ( 11.10000000122903252, 5.773502691896255534, 3.535250795749688894E-16 ) ) ;
#28894 = CARTESIAN_POINT ( 'NONE',  ( 7.828125000614517326, -4.541064518000419881, 2.621784821874995952 ) ) ;
#28895 = CARTESIAN_POINT ( 'NONE',  ( 24.48749999999999716, 5.773502691896255534, 3.535250795749688894E-16 ) ) ;
#28896 = CARTESIAN_POINT ( 'NONE',  ( 20.99062500061451431, -3.027376345333610441, -5.243569643749999898 ) ) ;
#28897 = CARTESIAN_POINT ( 'NONE',  ( 16.12500000122903288, 2.886751345948126879, 4.999999999999998224 ) ) ;
#28898 = CARTESIAN_POINT ( 'NONE',  ( 28.38750000122903216, -4.330127018922194537, 2.499999999999995559 ) ) ;
#28899 = CARTESIAN_POINT ( 'NONE',  ( 2.655984681222220721E-16, 16.35312499938548569, 25.66244784525396483 ) ) ;
#28900 = CARTESIAN_POINT ( 'NONE',  ( 8.212500000000000355, 2.886751345948129099, -4.999999999999998224 ) ) ;
#28901 = VECTOR ( 'NONE', #29102, 1000.000000000000000 ) ;
#28902 = EDGE_LOOP ( 'NONE', ( #5516, #33510, #19325, #2947 ) ) ;
#28903 = CARTESIAN_POINT ( 'NONE',  ( 22.79062500061451502, -3.027376345333610441, -5.243569643749999898 ) ) ;
#28904 = CARTESIAN_POINT ( 'NONE',  ( 3.401703127296281881, -3.664590583214551778, -3.702615937477313768 ) ) ;
#28905 = CARTESIAN_POINT ( 'NONE',  ( 28.50937500061451502, 0.000000000000000000, 5.243569643749999010 ) ) ;
#28906 = CARTESIAN_POINT ( 'NONE',  ( 19.62187500061451573, -6.054752690667223547, -1.112240025338166033E-15 ) ) ;
#28907 = CARTESIAN_POINT ( 'NONE',  ( 16.34062500061451573, -3.027376345333614438, 5.243569643749998122 ) ) ;
#28908 = CARTESIAN_POINT ( 'NONE',  ( 4.243569643749999010, 10.16562500061459673, -32.45002607614398471 ) ) ;
#28909 = CARTESIAN_POINT ( 'NONE',  ( 5.015625000614518214, 3.027376345333611329, 5.243569643749999010 ) ) ;
#28910 = AXIS2_PLACEMENT_3D ( 'NONE', #48611, #36786, #8712 ) ;
#28911 = CARTESIAN_POINT ( 'NONE',  ( 27.63750000122903216, 6.123233995736764310E-16, -4.999999999999998224 ) ) ;
#28912 = CARTESIAN_POINT ( 'NONE',  ( 22.84687500061451715, -2.746126346562641984, -4.756430356249999214 ) ) ;
#28913 = CARTESIAN_POINT ( 'NONE',  ( 18.02812500061451573, 4.541064518000418104, 2.621784821874999949 ) ) ;
#28914 = CYLINDRICAL_SURFACE ( 'NONE', #2062, 4.999999999999998224 ) ;
#28915 = CARTESIAN_POINT ( 'NONE',  ( 3.637500001229036162, -4.330127018922194537, 2.499999999999995559 ) ) ;
#28916 = CARTESIAN_POINT ( 'NONE',  ( 12.08437500061451608, 6.421520780324663323E-16, -5.243569643749999010 ) ) ;
#28917 = CARTESIAN_POINT ( 'NONE',  ( 13.20937500061451786, 0.000000000000000000, 5.243569643749999010 ) ) ;
#28918 = CARTESIAN_POINT ( 'NONE',  ( 21.12187500061451573, 3.027376345333613106, -5.243569643749998122 ) ) ;
#28919 = VERTEX_POINT ( 'NONE', #70420 ) ;
#28920 = CARTESIAN_POINT ( 'NONE',  ( -5.605356288733176484, 8.281802244057956841, 32.14897154774516252 ) ) ;
#28921 = CARTESIAN_POINT ( 'NONE',  ( 24.77812500061451217, 4.541064518000418104, 2.621784821874999949 ) ) ;
#28922 = VECTOR ( 'NONE', #34330, 1000.000000000000000 ) ;
#28923 = CARTESIAN_POINT ( 'NONE',  ( 17.89687500061451431, -3.027376345333610441, -5.243569643749999898 ) ) ;
#28924 = CARTESIAN_POINT ( 'NONE',  ( 24.59062500061451573, -3.027376345333610441, -5.243569643749999898 ) ) ;
#28925 = LINE ( 'NONE', #6032, #60433 ) ;
#28926 = CARTESIAN_POINT ( 'NONE',  ( 3.999999999999998668, 16.21250000000000213, 27.69059892324149175 ) ) ;
#28927 = CARTESIAN_POINT ( 'NONE',  ( 29.27812500061451573, 4.541064518000418104, 2.621784821874999949 ) ) ;
#28928 = CARTESIAN_POINT ( 'NONE',  ( 11.47500000122903252, 2.886751345948129099, -4.999999999999998224 ) ) ;
#28929 = VECTOR ( 'NONE', #36443, 1000.000000000000000 ) ;
#28930 = CARTESIAN_POINT ( 'NONE',  ( 7.237500001229035362, -4.330127018922194537, 2.499999999999995559 ) ) ;
#28931 = CARTESIAN_POINT ( 'NONE',  ( -3.999999999999997335, 19.13750000000000284, -27.69059892324149175 ) ) ;
#28932 = CARTESIAN_POINT ( 'NONE',  ( 26.62500000122903288, -5.773502691896255534, -1.060575238724906372E-15 ) ) ;
#28933 = CARTESIAN_POINT ( 'NONE',  ( 1.999999999999997335, 18.66874999877096641, 33.46410161513775705 ) ) ;
#28934 = CARTESIAN_POINT ( 'NONE',  ( 16.89375000122903359, 5.773502691896255534, 3.535250795749688894E-16 ) ) ;
#28935 = CARTESIAN_POINT ( 'NONE',  ( 8.859375000614518214, -4.541064518000417216, -2.621784821875001281 ) ) ;
#28936 = CARTESIAN_POINT ( 'NONE',  ( 17.66250000000000142, 2.886751345948162850, -4.999999999999940492 ) ) ;
#28937 = CARTESIAN_POINT ( 'NONE',  ( 17.99062500061451786, 6.054752690667223547, 3.707466751127219781E-16 ) ) ;
#28938 = CARTESIAN_POINT ( 'NONE',  ( 10.17187500061451999, -6.054752690667223547, -1.112240025338166033E-15 ) ) ;
#28939 = CARTESIAN_POINT ( 'NONE',  ( 29.58750000122903501, 4.330127018922191873, 2.499999999999999556 ) ) ;
#28940 = CARTESIAN_POINT ( 'NONE',  ( 20.03437500061451715, -4.541064518000419881, 2.621784821874995952 ) ) ;
#28941 = CARTESIAN_POINT ( 'NONE',  ( 7.584375000614516082, 6.421520780324663323E-16, -5.243569643749999010 ) ) ;
#28942 = CARTESIAN_POINT ( 'NONE',  ( 3.553125000614516082, 4.541064518000418104, -2.621784821874998173 ) ) ;
#28943 = CARTESIAN_POINT ( 'NONE',  ( 5.700000000000000178, 0.000000000000000000, 4.999999999999998224 ) ) ;
#28944 = CARTESIAN_POINT ( 'NONE',  ( 9.140625000614518214, -3.027376345333614438, 5.243569643749998122 ) ) ;
#28945 = CARTESIAN_POINT ( 'NONE',  ( 19.49062500061451431, -3.027376345333614438, 5.243569643749998122 ) ) ;
#28946 = ORIENTED_EDGE ( 'NONE', *, *, #31978, .F. ) ;
#28947 = CARTESIAN_POINT ( 'NONE',  ( 6.262500001229034829, 0.000000000000000000, 4.999999999999998224 ) ) ;
#28948 = CARTESIAN_POINT ( 'NONE',  ( 14.42812500061451786, 4.541064518000418104, 2.621784821874999949 ) ) ;
#28949 = CARTESIAN_POINT ( 'NONE',  ( 13.45312500061451466, 4.541064518000418104, -2.621784821874998173 ) ) ;
#28950 = CARTESIAN_POINT ( 'NONE',  ( 23.89687500061451786, 5.492252693125287522, 3.363034840372157021E-16 ) ) ;
#28951 = CARTESIAN_POINT ( 'NONE',  ( 14.43750000000000000, -2.886751345948125991, -5.000000000000000000 ) ) ;
#28952 = CARTESIAN_POINT ( 'NONE',  ( 8.887500001229033941, 4.330127018922191873, 2.499999999999999556 ) ) ;
#28953 = CARTESIAN_POINT ( 'NONE',  ( 5.128125000614516260, -4.541064518000419881, 2.621784821874995952 ) ) ;
#28954 = CARTESIAN_POINT ( 'NONE',  ( 17.51250000122903216, 0.000000000000000000, 4.999999999999998224 ) ) ;
#28955 = CARTESIAN_POINT ( 'NONE',  ( 28.16249999999999787, 2.886751345948126879, 4.999999999999999112 ) ) ;
#28956 = AXIS2_PLACEMENT_3D ( 'NONE', #1839, #13621, #18791 ) ;
#28957 = CARTESIAN_POINT ( 'NONE',  ( 9.001249775931846008E-16, 10.52187500061451964, -25.09994784771203058 ) ) ;
#28958 = CARTESIAN_POINT ( 'NONE',  ( 8.400000000000000355, 0.000000000000000000, 4.999999999999998224 ) ) ;
#28959 = EDGE_CURVE ( 'NONE', #54151, #16881, #47128, .T. ) ;
#28960 = CARTESIAN_POINT ( 'NONE',  ( 4.050000001229035362, -2.886751345948129988, 4.999999999999997335 ) ) ;
#28961 = CARTESIAN_POINT ( 'NONE',  ( -1.071796769724504328, 11.54240381056766829, -26.00000000000001066 ) ) ;
#28962 = CARTESIAN_POINT ( 'NONE',  ( 18.15937500061451715, 0.000000000000000000, 5.243569643749999010 ) ) ;
#28963 = CARTESIAN_POINT ( 'NONE',  ( 10.72500000122903252, 2.886751345948126879, 4.999999999999998224 ) ) ;
#28964 = AXIS2_PLACEMENT_3D ( 'NONE', #37805, #55175, #71431 ) ;
#28965 = CARTESIAN_POINT ( 'NONE',  ( 13.60312500061451679, 0.000000000000000000, 5.243569643749999010 ) ) ;
#28966 = CARTESIAN_POINT ( 'NONE',  ( 8.981250001229033941, -4.330127018922194537, 2.499999999999995559 ) ) ;
#28967 = CARTESIAN_POINT ( 'NONE',  ( -5.810221930991193690E-16, 14.60000000122903252, 26.00000000000000355 ) ) ;
#28968 = CARTESIAN_POINT ( 'NONE',  ( 28.84687500061452070, 6.054752690667223547, 3.707466751127219781E-16 ) ) ;
#28969 = CARTESIAN_POINT ( 'NONE',  ( 26.97187500061451360, 3.027376345333613106, -5.243569643749998122 ) ) ;
#28970 = CARTESIAN_POINT ( 'NONE',  ( 18.64687500061451431, -4.119189519843965641, -2.378215178125001383 ) ) ;
#28971 = CARTESIAN_POINT ( 'NONE',  ( 12.10312500061451857, 4.541064518000418104, -2.621784821874998173 ) ) ;
#28972 = AXIS2_PLACEMENT_3D ( 'NONE', #58030, #12974, #68416 ) ;
#28973 = CARTESIAN_POINT ( 'NONE',  ( 10.43437500061451750, 4.541064518000418104, 2.621784821874999949 ) ) ;
#28974 = ORIENTED_EDGE ( 'NONE', *, *, #28669, .F. ) ;
#28975 = CARTESIAN_POINT ( 'NONE',  ( 9.337499999999998579, -2.886751345948063374, 5.000000000000112799 ) ) ;
#28976 = CARTESIAN_POINT ( 'NONE',  ( 19.19062500061452070, -3.027376345333610441, -5.243569643749999898 ) ) ;
#28977 = CARTESIAN_POINT ( 'NONE',  ( 3.114445430177177343, 3.911558880626788248, -3.492103232390192602 ) ) ;
#28978 = CARTESIAN_POINT ( 'NONE',  ( 1.999999999999998668, 14.90000000000000036, 26.53589838486224650 ) ) ;
#28979 = CARTESIAN_POINT ( 'NONE',  ( 10.76250000000000107, -5.773502691896255534, -1.060575238724906372E-15 ) ) ;
#28980 = CARTESIAN_POINT ( 'NONE',  ( 22.35000000122903074, 5.773502691896255534, 3.535250795749688894E-16 ) ) ;
#28981 = CARTESIAN_POINT ( 'NONE',  ( 15.06562500061451537, -6.054752690667223547, -1.112240025338166033E-15 ) ) ;
#28982 = CARTESIAN_POINT ( 'NONE',  ( 10.54687500061451644, -4.119189519843965641, -2.378215178125001383 ) ) ;
#28983 = EDGE_LOOP ( 'NONE', ( #21022, #62018, #18850, #6009 ) ) ;
#28984 = CARTESIAN_POINT ( 'NONE',  ( 18.75000000000000000, 0.000000000000000000, 4.999999999999998224 ) ) ;
#28985 = CARTESIAN_POINT ( 'NONE',  ( 22.57499999999999929, 6.123233995736764310E-16, -4.999999999999998224 ) ) ;
#28986 = CARTESIAN_POINT ( 'NONE',  ( 19.28437500061451360, 6.421520780324663323E-16, -5.243569643749999010 ) ) ;
#28987 = CARTESIAN_POINT ( 'NONE',  ( 25.45312500061451644, -4.541064518000417216, -2.621784821875001281 ) ) ;
#28988 = ADVANCED_FACE ( 'NONE', ( #65231 ), #71146, .F. ) ;
#28989 = EDGE_LOOP ( 'NONE', ( #602, #31448, #53821, #28974 ) ) ;
#28990 = CARTESIAN_POINT ( 'NONE',  ( 27.93750000122903288, -4.330127018922194537, 2.499999999999995559 ) ) ;
#28991 = CARTESIAN_POINT ( 'NONE',  ( 7.190625000614518036, 6.054752690667223547, 3.707466751127219781E-16 ) ) ;
#28992 = CARTESIAN_POINT ( 'NONE',  ( -1.071796769724502107, 18.87634618820330346, 26.00000000000000711 ) ) ;
#28993 = CARTESIAN_POINT ( 'NONE',  ( 13.61250000000000071, 2.886751345948129099, -4.999999999999998224 ) ) ;
#28994 = CARTESIAN_POINT ( 'NONE',  ( -4.243569643749999898, 16.65312500061451573, 30.00000000000000000 ) ) ;
#28995 = CARTESIAN_POINT ( 'NONE',  ( 28.15312500061451573, -4.541064518000417216, -2.621784821875001281 ) ) ;
#28996 = CARTESIAN_POINT ( 'NONE',  ( -3.756430356250001434, 14.70312499938548179, 32.16877607737301048 ) ) ;
#28997 = CARTESIAN_POINT ( 'NONE',  ( 25.73437500061451644, 4.541064518000418104, 2.621784821874999949 ) ) ;
#28998 = ORIENTED_EDGE ( 'NONE', *, *, #23453, .T. ) ;
#28999 = CARTESIAN_POINT ( 'NONE',  ( 22.79062500061451502, -3.027376345333610441, -5.243569643749999898 ) ) ;
#29000 = CARTESIAN_POINT ( 'NONE',  ( 25.02187500061451431, -6.054752690667223547, -1.112240025338166033E-15 ) ) ;
#29001 = CARTESIAN_POINT ( 'NONE',  ( -4.243569643749999898, 19.80312500061451786, -30.00000000000000000 ) ) ;
#29002 = CARTESIAN_POINT ( 'NONE',  ( 11.51250000000000107, 2.886751345948126879, 4.999999999999999112 ) ) ;
#29003 = CARTESIAN_POINT ( 'NONE',  ( 9.028125000614517504, 4.541064518000418104, 2.621784821874999949 ) ) ;
#29004 = CARTESIAN_POINT ( 'NONE',  ( 28.35937500061451289, 4.119189519843966529, -2.378215178124998275 ) ) ;
#29005 = CARTESIAN_POINT ( 'NONE',  ( 29.57812500061451644, 6.421520780324663323E-16, -5.243569643749999010 ) ) ;
#29006 = CARTESIAN_POINT ( 'NONE',  ( 26.27812500061451573, -4.541064518000419881, 2.621784821874995952 ) ) ;
#29007 = CARTESIAN_POINT ( 'NONE',  ( 27.72187500061451715, 5.824947211148865298E-16, -4.756430356249998326 ) ) ;
#29008 = CARTESIAN_POINT ( 'NONE',  ( 13.13437500061451857, 4.119189519843966529, 2.378215178124999607 ) ) ;
#29009 = CARTESIAN_POINT ( 'NONE',  ( 18.34687500061451715, -3.027376345333610441, -5.243569643749999898 ) ) ;
#29010 = CARTESIAN_POINT ( 'NONE',  ( 2.121784821875001281, 11.45937500061451786, 33.67503911421598417 ) ) ;
#29011 = CARTESIAN_POINT ( 'NONE',  ( 19.09687500061451360, -3.027376345333614438, 5.243569643749998122 ) ) ;
#29012 = CARTESIAN_POINT ( 'NONE',  ( 27.83437500061451786, 6.421520780324663323E-16, -5.243569643749999010 ) ) ;
#29013 = CARTESIAN_POINT ( 'NONE',  ( -2.121784821874996840, 17.23437500061451999, 33.67503911421598417 ) ) ;
#29014 = CARTESIAN_POINT ( 'NONE',  ( 7.153125000614518392, 4.541064518000418104, -2.621784821874998173 ) ) ;
#29015 = FACE_OUTER_BOUND ( 'NONE', #63332, .T. ) ;
#29016 = CARTESIAN_POINT ( 'NONE',  ( 3.721875000614518036, 3.027376345333611329, 5.243569643749999010 ) ) ;
#29017 = CARTESIAN_POINT ( 'NONE',  ( 1.592000809091587073E-14, 15.95000000122903394, -34.00000000000000000 ) ) ;
#29018 = AXIS2_PLACEMENT_3D ( 'NONE', #23473, #46019, #52279 ) ;
#29019 = CARTESIAN_POINT ( 'NONE',  ( 6.253125000614517148, 4.541064518000418104, -2.621784821874998173 ) ) ;
#29020 = CARTESIAN_POINT ( 'NONE',  ( 9.046875000614518214, 6.054752690667223547, 3.707466751127219781E-16 ) ) ;
#29021 = CARTESIAN_POINT ( 'NONE',  ( 19.61250000122903359, 4.330127018922192761, -2.499999999999997780 ) ) ;
#29022 = CARTESIAN_POINT ( 'NONE',  ( 6.721875000614518925, 3.027376345333613106, -5.243569643749998122 ) ) ;
#29023 = CARTESIAN_POINT ( 'NONE',  ( 6.665625000614515905, 3.027376345333613106, -5.243569643749998122 ) ) ;
#29024 = DIRECTION ( 'NONE',  ( -1.000000000000000000, -0.000000000000000000, -0.000000000000000000 ) ) ;
#29025 = CARTESIAN_POINT ( 'NONE',  ( 22.96875000122903643, -5.773502691896255534, -1.060575238724906372E-15 ) ) ;
#29026 = CARTESIAN_POINT ( 'NONE',  ( 15.53437500061451715, -4.541064518000419881, 2.621784821874995952 ) ) ;
#29027 = CARTESIAN_POINT ( 'NONE',  ( 45.00000000000000000, 6.123233995736764310E-16, -4.999999999999998224 ) ) ;
#29028 = VERTEX_POINT ( 'NONE', #53058 ) ;
#29029 = CARTESIAN_POINT ( 'NONE',  ( 23.46562500061451573, 3.027376345333611329, 5.243569643749999010 ) ) ;
#29030 = CARTESIAN_POINT ( 'NONE',  ( 10.04062500061451502, -3.027376345333614438, 5.243569643749998122 ) ) ;
#29031 = CARTESIAN_POINT ( 'NONE',  ( 26.78437500061451360, -4.541064518000419881, 2.621784821874995952 ) ) ;
#29032 = APPLICATION_CONTEXT ( 'automotive_design' ) ;
#29033 = CARTESIAN_POINT ( 'NONE',  ( 10.04062500061451502, -3.027376345333614438, 5.243569643749998122 ) ) ;
#29034 = DIRECTION ( 'NONE',  ( -1.000000000000000000, -0.000000000000000000, -0.000000000000000000 ) ) ;
#29035 = CARTESIAN_POINT ( 'NONE',  ( 13.38750000122903394, 4.330127018922191873, 2.499999999999999556 ) ) ;
#29036 =( BOUNDED_CURVE ( )  B_SPLINE_CURVE ( 2, ( #60756, #32698, #4630, #44883, #50423, #72949, #539 ),
 .UNSPECIFIED., .F., .F. ) 
 B_SPLINE_CURVE_WITH_KNOTS ( ( 3, 2, 2, 3 ),
 ( 0.2500000000000000000, 0.2527777777777777679, 0.2555555555555554803, 0.2583333333333333037 ),
 .UNSPECIFIED. ) 
 CURVE ( )  GEOMETRIC_REPRESENTATION_ITEM ( )  RATIONAL_B_SPLINE_CURVE ( ( 1.000000000000000000, 0.8660254037844387076, 1.000000000000000000, 0.8660254037844387076, 1.000000000000000000, 0.8660254037844413721, 0.9999999999999973355 ) ) 
 REPRESENTATION_ITEM ( '' )  );
#29037 = CARTESIAN_POINT ( 'NONE',  ( 27.29062500061451502, -3.027376345333610441, -5.243569643749999898 ) ) ;
#29038 = CARTESIAN_POINT ( 'NONE',  ( 9.001249775931846008E-16, 13.16562500061451857, -25.09994784771203058 ) ) ;
#29039 = CARTESIAN_POINT ( 'NONE',  ( 13.80000000122903181, 5.773502691896255534, 3.535250795749688894E-16 ) ) ;
#29040 = CARTESIAN_POINT ( 'NONE',  ( 11.32500000000000107, 6.123233995736764310E-16, -4.999999999999998224 ) ) ;
#29041 = CARTESIAN_POINT ( 'NONE',  ( 20.42812500061451431, -4.541064518000419881, 2.621784821874995952 ) ) ;
#29042 = CARTESIAN_POINT ( 'NONE',  ( 6.384375000614516793, 4.541064518000418104, 2.621784821874999949 ) ) ;
#29043 = CARTESIAN_POINT ( 'NONE',  ( 19.76250000000000639, -5.773502691896255534, -1.060575238724906372E-15 ) ) ;
#29044 = CARTESIAN_POINT ( 'NONE',  ( 6.937500001229033764, 6.123233995736764310E-16, -4.999999999999998224 ) ) ;
#29045 = CARTESIAN_POINT ( 'NONE',  ( 16.53750000122903430, 4.330127018922191873, 2.499999999999999556 ) ) ;
#29046 = CARTESIAN_POINT ( 'NONE',  ( 12.66562500061451502, 3.027376345333611329, 5.243569643749999010 ) ) ;
#29047 = CARTESIAN_POINT ( 'NONE',  ( 15.14062500061451644, -3.027376345333610441, -5.243569643749999898 ) ) ;
#29048 = CARTESIAN_POINT ( 'NONE',  ( 25.35000000122903074, -2.886751345948125991, -5.000000000000000000 ) ) ;
#29049 = CARTESIAN_POINT ( 'NONE',  ( 20.62499999999999645, -4.330127018922194537, 2.499999999999995559 ) ) ;
#29050 = CARTESIAN_POINT ( 'NONE',  ( 22.84687500061451715, -3.027376345333610441, -5.243569643749999898 ) ) ;
#29051 = DIRECTION ( 'NONE',  ( -1.000000000000000000, -0.000000000000000000, -0.000000000000000000 ) ) ;
#29052 = CARTESIAN_POINT ( 'NONE',  ( 10.31250000122903288, 0.000000000000000000, 4.999999999999998224 ) ) ;
#29053 = CARTESIAN_POINT ( 'NONE',  ( 9.459375000614517859, 4.541064518000418104, -2.621784821874998173 ) ) ;
#29054 = CARTESIAN_POINT ( 'NONE',  ( 26.22187500061451715, 3.027376345333611329, 5.243569643749999010 ) ) ;
#29055 = CARTESIAN_POINT ( 'NONE',  ( 3.796875000614517326, -3.027376345333614438, 5.243569643749998122 ) ) ;
#29056 = CARTESIAN_POINT ( 'NONE',  ( 22.90312500061451573, 4.541064518000418104, -2.621784821874998173 ) ) ;
#29057 = CARTESIAN_POINT ( 'NONE',  ( 26.52187500061451431, 3.027376345333613106, -5.243569643749998122 ) ) ;
#29058 = CARTESIAN_POINT ( 'NONE',  ( 3.756430356250000546, 17.74062499938548498, 27.83122392262697886 ) ) ;
#29059 = CARTESIAN_POINT ( 'NONE',  ( 17.88749999999999929, -2.886751345948074920, 5.000000000000092371 ) ) ;
#29060 = VECTOR ( 'NONE', #1869, 1000.000000000000000 ) ;
#29061 = CARTESIAN_POINT ( 'NONE',  ( 8.446875000614518569, -3.027376345333610441, -5.243569643749999898 ) ) ;
#29062 = CARTESIAN_POINT ( 'NONE',  ( 0.6522972858965978560, 20.64114861271052348, 33.69936173848522998 ) ) ;
#29063 = CARTESIAN_POINT ( 'NONE',  ( 28.49062500061451431, -3.027376345333614438, 5.243569643749998122 ) ) ;
#29064 = CARTESIAN_POINT ( 'NONE',  ( 7.359375000614516438, 0.000000000000000000, 5.243569643749999010 ) ) ;
#29065 = CARTESIAN_POINT ( 'NONE',  ( 25.80000000000000071, 4.330127018922192761, -2.499999999999997780 ) ) ;
#29066 = CARTESIAN_POINT ( 'NONE',  ( -2.121784821874996840, 9.978125000614596729, 33.67503911421598417 ) ) ;
#29067 = CARTESIAN_POINT ( 'NONE',  ( 18.11250000000000071, 2.886751345948129099, -4.999999999999998224 ) ) ;
#29068 = ORIENTED_EDGE ( 'NONE', *, *, #22509, .T. ) ;
#29069 = CARTESIAN_POINT ( 'NONE',  ( 28.27499999999999858, -4.330127018922194537, 2.499999999999995559 ) ) ;
#29070 = CARTESIAN_POINT ( 'NONE',  ( 29.67187500061451644, 3.027376345333613106, -5.243569643749998122 ) ) ;
#29071 = ADVANCED_FACE ( 'NONE', ( #59686 ), #31255, .F. ) ;
#29072 = ORIENTED_EDGE ( 'NONE', *, *, #47483, .T. ) ;
#29073 = CARTESIAN_POINT ( 'NONE',  ( 16.04062500061451857, -3.027376345333610441, -5.243569643749999898 ) ) ;
#29074 = CARTESIAN_POINT ( 'NONE',  ( 5.878125000614517148, 4.541064518000418104, 2.621784821874999949 ) ) ;
#29075 = CARTESIAN_POINT ( 'NONE',  ( 19.35937500061451644, 2.746126346562643317, 4.756430356249998326 ) ) ;
#29076 = CARTESIAN_POINT ( 'NONE',  ( 5.409375000614516260, 4.541064518000418104, -2.621784821874998173 ) ) ;
#29077 = CARTESIAN_POINT ( 'NONE',  ( 15.03750000122903252, 6.123233995736764310E-16, -4.999999999999998224 ) ) ;
#29078 = CARTESIAN_POINT ( 'NONE',  ( 21.33749999999999858, 5.773502691896255534, 3.535250795749688894E-16 ) ) ;
#29079 = CARTESIAN_POINT ( 'NONE',  ( 28.87499999999999645, 6.123233995736764310E-16, -4.999999999999998224 ) ) ;
#29080 = CARTESIAN_POINT ( 'NONE',  ( 5.634375000614519458, -4.541064518000419881, 2.621784821874995952 ) ) ;
#29081 = CARTESIAN_POINT ( 'NONE',  ( 8.259375000614518569, 0.000000000000000000, 5.243569643749999010 ) ) ;
#29082 = CARTESIAN_POINT ( 'NONE',  ( 21.04687500061451644, -3.027376345333610441, -5.243569643749999898 ) ) ;
#29083 = CARTESIAN_POINT ( 'NONE',  ( 0.000000000000000000, 20.00000000000000000, -30.00000000000000000 ) ) ;
#29084 = EDGE_LOOP ( 'NONE', ( #52976, #59546, #56880, #33027 ) ) ;
#29085 = CARTESIAN_POINT ( 'NONE',  ( 5.071875000614519458, 3.027376345333611329, 5.243569643749999010 ) ) ;
#29086 = CARTESIAN_POINT ( 'NONE',  ( 5.662500000000000533, 2.886751345948126879, 4.999999999999999112 ) ) ;
#29087 = CARTESIAN_POINT ( 'NONE',  ( 6.609375000614519102, -4.541064518000417216, -2.621784821875001281 ) ) ;
#29088 = CARTESIAN_POINT ( 'NONE',  ( 17.47499999999999787, -4.330127018922194537, 2.499999999999995559 ) ) ;
#29089 = CARTESIAN_POINT ( 'NONE',  ( 16.49062500061451786, -3.027376345333610441, -5.243569643749999898 ) ) ;
#29090 = CARTESIAN_POINT ( 'NONE',  ( -3.999999999999999556, 19.88749999999999929, 27.69059892324149175 ) ) ;
#29091 = CARTESIAN_POINT ( 'NONE',  ( 4.206670228171102366, 2.702577582867563333, 4.419125496164216571 ) ) ;
#29092 = CARTESIAN_POINT ( 'NONE',  ( 20.82187500061451857, 2.746126346562643317, 4.756430356249998326 ) ) ;
#29093 = CARTESIAN_POINT ( 'NONE',  ( 9.328125000614518214, 6.421520780324663323E-16, -5.243569643749999010 ) ) ;
#29094 = CARTESIAN_POINT ( 'NONE',  ( 27.83437500061451786, 6.421520780324663323E-16, -5.243569643749999010 ) ) ;
#29095 = CARTESIAN_POINT ( 'NONE',  ( 0.000000000000000000, 20.00000000000000000, -30.00000000000000000 ) ) ;
#29096 = CARTESIAN_POINT ( 'NONE',  ( 26.63437500061451857, 4.541064518000418104, 2.621784821874999949 ) ) ;
#29097 = CARTESIAN_POINT ( 'NONE',  ( 8.324999999999999289, 4.330127018922191873, 2.499999999999999556 ) ) ;
#29098 = CARTESIAN_POINT ( 'NONE',  ( 4.000000000000000000, 13.55000000122903359, 32.30940107675849049 ) ) ;
#29099 = CARTESIAN_POINT ( 'NONE',  ( 6.675000001229034474, 2.886751345948126879, 4.999999999999999112 ) ) ;
#29100 = CARTESIAN_POINT ( 'NONE',  ( 18.23437500061451999, -4.541064518000419881, 2.621784821874995952 ) ) ;
#29101 = CARTESIAN_POINT ( 'NONE',  ( 11.25937500061451679, 4.541064518000418104, -2.621784821874998173 ) ) ;
#29102 = DIRECTION ( 'NONE',  ( -1.000000000000000000, -0.000000000000000000, -0.000000000000000000 ) ) ;
#29103 = EDGE_LOOP ( 'NONE', ( #11049, #57332, #66201, #62373 ) ) ;
#29104 = CARTESIAN_POINT ( 'NONE',  ( 14.50312500061451537, 0.000000000000000000, 5.243569643749999010 ) ) ;
#29105 = CARTESIAN_POINT ( 'NONE',  ( 25.35000000122903074, -2.886751345948125991, -5.000000000000000000 ) ) ;
#29106 = CARTESIAN_POINT ( 'NONE',  ( 13.77187500061451786, -6.054752690667223547, -1.112240025338166033E-15 ) ) ;
#29107 = AXIS2_PLACEMENT_3D ( 'NONE', #14663, #70465, #37206 ) ;
#29108 = CARTESIAN_POINT ( 'NONE',  ( 21.44999999999999929, 0.000000000000000000, 4.999999999999998224 ) ) ;
#29109 = CARTESIAN_POINT ( 'NONE',  ( 14.46562500061451750, 3.027376345333611329, 5.243569643749999010 ) ) ;
#29110 = LINE ( 'NONE', #63800, #66939 ) ;
#29111 = CARTESIAN_POINT ( 'NONE',  ( 25.95937500061451431, -4.541064518000417216, -2.621784821875001281 ) ) ;
#29112 = CARTESIAN_POINT ( 'NONE',  ( 2.886376055866514356, -4.082748248927369872, 3.290317514273759958 ) ) ;
#29113 = CARTESIAN_POINT ( 'NONE',  ( 11.58750000122903501, 4.330127018922191873, 2.499999999999999556 ) ) ;
#29114 = CARTESIAN_POINT ( 'NONE',  ( 8.334375000614516082, -4.119189519843968306, 2.378215178124996054 ) ) ;
#29115 = CARTESIAN_POINT ( 'NONE',  ( 14.88749999999999929, -2.886751345948126435, -5.000000000000000000 ) ) ;
#29116 = CARTESIAN_POINT ( 'NONE',  ( 2.121784821875001281, 16.40937500061452070, -26.32496088578401938 ) ) ;
#29117 = CARTESIAN_POINT ( 'NONE',  ( 17.74687500061451928, -3.027376345333614438, 5.243569643749998122 ) ) ;
#29118 = CARTESIAN_POINT ( 'NONE',  ( 20.10000000122903074, 5.773502691896255534, 3.535250795749688894E-16 ) ) ;
#29119 = CARTESIAN_POINT ( 'NONE',  ( 14.18437500061451750, -4.541064518000419881, 2.621784821874995952 ) ) ;
#29120 = CARTESIAN_POINT ( 'NONE',  ( 2.121784821875001281, 10.55937500061451750, 33.67503911421598417 ) ) ;
#29121 = CARTESIAN_POINT ( 'NONE',  ( 22.35000000122903074, 5.773502691896255534, 3.535250795749688894E-16 ) ) ;
#29122 = AXIS2_PLACEMENT_3D ( 'NONE', #20587, #43513, #66404 ) ;
#29123 = CARTESIAN_POINT ( 'NONE',  ( 14.87812500061451537, 4.541064518000418104, 2.621784821874999949 ) ) ;
#29124 = CARTESIAN_POINT ( 'NONE',  ( 29.65312500061451573, 4.541064518000418104, -2.621784821874998173 ) ) ;
#29125 = ORIENTED_EDGE ( 'NONE', *, *, #31318, .T. ) ;
#29126 = VERTEX_POINT ( 'NONE', #25719 ) ;
#29127 = CARTESIAN_POINT ( 'NONE',  ( 19.23749999999999716, -2.886751345948129988, 4.999999999999997335 ) ) ;
#29128 = DIRECTION ( 'NONE',  ( -0.000000000000000000, -1.000000000000000000, -0.000000000000000000 ) ) ;
#29129 = CARTESIAN_POINT ( 'NONE',  ( 3.780892357739493281, 3.275126314170738517, 31.33023311637936459 ) ) ;
#29130 = CARTESIAN_POINT ( 'NONE',  ( 15.60000000122903607, 5.773502691896255534, 3.535250795749688894E-16 ) ) ;
#29131 = CARTESIAN_POINT ( 'NONE',  ( 19.64062500061451644, -3.027376345333610441, -5.243569643749999898 ) ) ;
#29132 = CARTESIAN_POINT ( 'NONE',  ( 22.00312500061451360, 4.541064518000418104, -2.621784821874998173 ) ) ;
#29133 = CARTESIAN_POINT ( 'NONE',  ( 3.928125000614516527, 6.421520780324663323E-16, -5.243569643749999010 ) ) ;
#29134 = CARTESIAN_POINT ( 'NONE',  ( 26.58750000000000213, -2.886751345948125991, -5.000000000000000000 ) ) ;
#29135 = CARTESIAN_POINT ( 'NONE',  ( 17.71875000122903288, 2.886751345948129099, -4.999999999999997335 ) ) ;
#29136 = CARTESIAN_POINT ( 'NONE',  ( 8.859375000614518214, -4.119189519843965641, -2.378215178125001383 ) ) ;
#29137 = CARTESIAN_POINT ( 'NONE',  ( 0.000000000000000000, 20.00000000000000000, 26.00000000000000000 ) ) ;
#29138 = CARTESIAN_POINT ( 'NONE',  ( -2.000000000000000000, 10.13750000122903572, -33.46410161513775705 ) ) ;
#29139 = CARTESIAN_POINT ( 'NONE',  ( -4.243569643749997233, 15.39687500061451786, -27.54997392385601174 ) ) ;
#29140 = CARTESIAN_POINT ( 'NONE',  ( 5.175000001229033586, 2.886751345948129099, -4.999999999999998224 ) ) ;
#29141 = CARTESIAN_POINT ( 'NONE',  ( 9.375000000000001776, -4.330127018922194537, 2.499999999999995559 ) ) ;
#29142 = CARTESIAN_POINT ( 'NONE',  ( 4.725000001229034297, 2.886751345948129099, -4.999999999999998224 ) ) ;
#29143 = CARTESIAN_POINT ( 'NONE',  ( 8.784375000614518925, -4.541064518000419881, 2.621784821874995952 ) ) ;
#29144 = CARTESIAN_POINT ( 'NONE',  ( 19.31250000122903288, 0.000000000000000000, 4.999999999999998224 ) ) ;
#29145 = CARTESIAN_POINT ( 'NONE',  ( 24.71250000122903145, 0.000000000000000000, 4.999999999999998224 ) ) ;
#29146 = CARTESIAN_POINT ( 'NONE',  ( -1.974232797588181931, 9.810253314282340042, -35.67951850763265043 ) ) ;
#29147 = CARTESIAN_POINT ( 'NONE',  ( 17.02500000122903145, 2.886751345948161074, 4.999999999999941380 ) ) ;
#29148 = ADVANCED_FACE ( 'NONE', ( #42710 ), #24031, .T. ) ;
#29149 = CARTESIAN_POINT ( 'NONE',  ( 7.134375000614516793, 6.421520780324663323E-16, -5.243569643749999010 ) ) ;
#29150 = CARTESIAN_POINT ( 'NONE',  ( 12.57187500061451857, 3.027376345333613106, -5.243569643749998122 ) ) ;
#29151 = CARTESIAN_POINT ( 'NONE',  ( 3.525000000000000355, -4.330127018922194537, 2.499999999999995559 ) ) ;
#29152 = CARTESIAN_POINT ( 'NONE',  ( 6.112499999999999822, 2.886751345948126879, 4.999999999999999112 ) ) ;
#29153 = VECTOR ( 'NONE', #54208, 1000.000000000000000 ) ;
#29154 = CARTESIAN_POINT ( 'NONE',  ( 4.243569643749999010, 17.36562500061459602, 27.54997392385601174 ) ) ;
#29155 = CARTESIAN_POINT ( 'NONE',  ( 22.20937500061451431, 0.000000000000000000, 5.243569643749999010 ) ) ;
#29156 = CARTESIAN_POINT ( 'NONE',  ( 1.626862140677534273E-15, 11.11250000000000071, -26.00000000000000355 ) ) ;
#29157 = CARTESIAN_POINT ( 'NONE',  ( 25.80000000122903714, -2.886751345948125991, -5.000000000000000000 ) ) ;
#29158 = CARTESIAN_POINT ( 'NONE',  ( 16.88437500061451857, -2.746126346562642428, -4.756430356249999214 ) ) ;
#29159 = CARTESIAN_POINT ( 'NONE',  ( 23.72812500061451502, 6.421520780324663323E-16, -5.243569643749999010 ) ) ;
#29160 = CARTESIAN_POINT ( 'NONE',  ( 13.30312500061451786, -4.541064518000417216, -2.621784821875001281 ) ) ;
#29161 = CARTESIAN_POINT ( 'NONE',  ( 26.18437500061451573, -2.746126346562646425, 4.756430356249996549 ) ) ;
#29162 = CARTESIAN_POINT ( 'NONE',  ( 12.57187500061451857, 3.027376345333613106, -5.243569643749998122 ) ) ;
#29163 = CARTESIAN_POINT ( 'NONE',  ( 29.58749999999999858, -2.886751345948129988, 4.999999999999997335 ) ) ;
#29164 = CARTESIAN_POINT ( 'NONE',  ( 21.67500000122903359, -5.773502691896255534, -1.060575238724906372E-15 ) ) ;
#29165 = DIRECTION ( 'NONE',  ( 0.000000000000000000, 0.000000000000000000, -1.000000000000000000 ) ) ;
#29166 = CARTESIAN_POINT ( 'NONE',  ( 11.40937500061451892, 0.000000000000000000, 5.243569643749999010 ) ) ;
#29167 = CARTESIAN_POINT ( 'NONE',  ( 28.17187500061451644, -6.054752690667223547, -1.112240025338166033E-15 ) ) ;
#29168 = CARTESIAN_POINT ( 'NONE',  ( -3.999999999999997335, 12.38750000000000107, -27.69059892324149530 ) ) ;
#29169 = CARTESIAN_POINT ( 'NONE',  ( 21.79687500061451644, -3.027376345333614438, 5.243569643749998122 ) ) ;
#29170 = CARTESIAN_POINT ( 'NONE',  ( 13.17187500061451999, 3.027376345333611329, 5.243569643749999010 ) ) ;
#29171 = CARTESIAN_POINT ( 'NONE',  ( -1.878215178125001827, 18.45312499938548356, 33.25316411605952283 ) ) ;
#29172 = CARTESIAN_POINT ( 'NONE',  ( 25.31250000000000000, 2.886751345948129099, -4.999999999999998224 ) ) ;
#29173 = CARTESIAN_POINT ( 'NONE',  ( 2.000000000000000444, 13.47500000000000142, 26.53589838486224650 ) ) ;
#29174 = CARTESIAN_POINT ( 'NONE',  ( 28.02187500061451431, 2.746126346562643317, 4.756430356249998326 ) ) ;
#29175 = CARTESIAN_POINT ( 'NONE',  ( 18.29062500061451502, -3.027376345333610441, -5.243569643749999898 ) ) ;
#29176 = CARTESIAN_POINT ( 'NONE',  ( 7.462500000000001243, 2.886751345948126879, 4.999999999999999112 ) ) ;
#29177 =( BOUNDED_CURVE ( )  B_SPLINE_CURVE ( 2, ( #39317, #50757, #51481, #160, #6048, #62555, #28943 ),
 .UNSPECIFIED., .F., .F. ) 
 B_SPLINE_CURVE_WITH_KNOTS ( ( 3, 2, 2, 3 ),
 ( 0.8916666666666667185, 0.8944444444444444864, 0.8972222222222223653, 0.9000000000000001332 ),
 .UNSPECIFIED. ) 
 CURVE ( )  GEOMETRIC_REPRESENTATION_ITEM ( )  RATIONAL_B_SPLINE_CURVE ( ( 1.000000000000000000, 0.8660254037844387076, 1.000000000000000000, 0.8660254037844387076, 1.000000000000000000, 0.8660254037844333785, 1.000000000000005329 ) ) 
 REPRESENTATION_ITEM ( '' )  );
#29178 = CARTESIAN_POINT ( 'NONE',  ( 2.953125000614516438, -4.541064518000417216, -2.621784821875001281 ) ) ;
#29179 = CARTESIAN_POINT ( 'NONE',  ( 15.07499999999999929, 4.330127018922191873, 2.499999999999999556 ) ) ;
#29180 = CARTESIAN_POINT ( 'NONE',  ( 4.243569643749999898, 11.44062500061451715, 32.45002607614398471 ) ) ;
#29181 = CARTESIAN_POINT ( 'NONE',  ( 14.58750000000000036, 5.773502691896255534, 3.535250795749688401E-16 ) ) ;
#29182 = CARTESIAN_POINT ( 'NONE',  ( 26.55937500061451573, 4.541064518000418104, -2.621784821874998173 ) ) ;
#29183 = ORIENTED_EDGE ( 'NONE', *, *, #57737, .T. ) ;
#29184 = CARTESIAN_POINT ( 'NONE',  ( 22.86562500061451431, 3.027376345333613106, -5.243569643749998122 ) ) ;
#29185 = CARTESIAN_POINT ( 'NONE',  ( 20.07187500061451857, -6.054752690667223547, -1.112240025338166033E-15 ) ) ;
#29186 = CARTESIAN_POINT ( 'NONE',  ( 4.762499999999999289, 2.886751345948126879, 4.999999999999999112 ) ) ;
#29187 = CARTESIAN_POINT ( 'NONE',  ( 7.040625000614517681, -3.027376345333610441, -5.243569643749999898 ) ) ;
#29188 = CARTESIAN_POINT ( 'NONE',  ( 21.77812500061451928, -4.541064518000419881, 2.621784821874995952 ) ) ;
#29189 = CARTESIAN_POINT ( 'NONE',  ( 11.59687500061451892, -3.027376345333610441, -5.243569643749999898 ) ) ;
#29190 = CARTESIAN_POINT ( 'NONE',  ( 17.07187500061451502, 3.027376345333613106, -5.243569643749998122 ) ) ;
#29191 = CARTESIAN_POINT ( 'NONE',  ( 4.243569643749999898, 16.84062500061451573, 32.45002607614398471 ) ) ;
#29192 = CARTESIAN_POINT ( 'NONE',  ( 20.10000000122903074, 5.773502691896255534, 3.535250795749688894E-16 ) ) ;
#29193 = CARTESIAN_POINT ( 'NONE',  ( 14.37187500061451750, 2.746126346562645981, -4.756430356249997438 ) ) ;
#29194 = CARTESIAN_POINT ( 'NONE',  ( 9.665625000614516793, -6.054752690667223547, -1.112240025338166033E-15 ) ) ;
#29195 = CARTESIAN_POINT ( 'NONE',  ( 6.121875000614517504, -6.054752690667223547, -1.112240025338166033E-15 ) ) ;
#29196 = CARTESIAN_POINT ( 'NONE',  ( 4.471875000614518925, 3.027376345333613106, -5.243569643749998122 ) ) ;
#29197 = CARTESIAN_POINT ( 'NONE',  ( 25.24687500061451573, 6.054752690667223547, 3.707466751127219781E-16 ) ) ;
#29198 = CARTESIAN_POINT ( 'NONE',  ( 16.60312500061451857, 4.541064518000418104, -2.621784821874998173 ) ) ;
#29199 = CARTESIAN_POINT ( 'NONE',  ( 26.62500000122903288, -5.773502691896255534, -1.060575238724906372E-15 ) ) ;
#29200 = CARTESIAN_POINT ( 'NONE',  ( 25.79062500061451502, -3.027376345333614438, 5.243569643749998122 ) ) ;
#29201 = CARTESIAN_POINT ( 'NONE',  ( 22.24687500061451217, -3.027376345333614438, 5.243569643749998122 ) ) ;
#29202 = CARTESIAN_POINT ( 'NONE',  ( 18.29062500061451502, -3.027376345333610441, -5.243569643749999898 ) ) ;
#29203 = CARTESIAN_POINT ( 'NONE',  ( 4.243569643749999898, 16.48437500061451644, 30.00000000000000000 ) ) ;
#29204 = CARTESIAN_POINT ( 'NONE',  ( 22.79062500061451502, -3.027376345333610441, -5.243569643749999898 ) ) ;
#29205 = DIRECTION ( 'NONE',  ( -1.000000000000000000, -0.000000000000000000, -0.000000000000000000 ) ) ;
#29206 = VERTEX_POINT ( 'NONE', #57003 ) ;
#29207 = CARTESIAN_POINT ( 'NONE',  ( 25.38749999999999929, 5.773502691896255534, 3.535250795749688894E-16 ) ) ;
#29208 = CARTESIAN_POINT ( 'NONE',  ( -3.999999999999999556, 13.21250000000000213, -32.30940107675850470 ) ) ;
#29209 = CARTESIAN_POINT ( 'NONE',  ( 3.756430356249998770, 20.36562499938548143, 32.16877607737302469 ) ) ;
#29210 = CARTESIAN_POINT ( 'NONE',  ( 28.26562500061451289, 3.027376345333613106, -5.243569643749998122 ) ) ;
#29211 = CARTESIAN_POINT ( 'NONE',  ( 9.178125000614517859, -4.541064518000419881, 2.621784821874995952 ) ) ;
#29212 = CARTESIAN_POINT ( 'NONE',  ( 22.42500000122903359, 2.886751345948126879, 4.999999999999999112 ) ) ;
#29213 = CARTESIAN_POINT ( 'NONE',  ( 28.37812500061451715, 4.541064518000418104, 2.621784821874999949 ) ) ;
#29214 = CARTESIAN_POINT ( 'NONE',  ( 26.62500000000000000, 6.123233995736764310E-16, -4.999999999999998224 ) ) ;
#29215 = CARTESIAN_POINT ( 'NONE',  ( -3.999999999999999556, 17.37500000122903288, -32.30940107675850470 ) ) ;
#29216 = CARTESIAN_POINT ( 'NONE',  ( 25.31250000122903288, -4.330127018922190985, -2.500000000000001332 ) ) ;
#29217 = CARTESIAN_POINT ( 'NONE',  ( 10.04062500061451502, -3.027376345333614438, 5.243569643749998122 ) ) ;
#29218 = VERTEX_POINT ( 'NONE', #68468 ) ;
#29219 = EDGE_CURVE ( 'NONE', #43350, #32246, #40438, .T. ) ;
#29220 = CARTESIAN_POINT ( 'NONE',  ( 26.46562500061451573, 3.027376345333613106, -5.243569643749998122 ) ) ;
#29221 = CARTESIAN_POINT ( 'NONE',  ( 7.753125000614518036, 0.000000000000000000, 5.243569643749999010 ) ) ;
#29222 = CARTESIAN_POINT ( 'NONE',  ( 6.403125000614517504, 0.000000000000000000, 5.243569643749999010 ) ) ;
#29223 = CARTESIAN_POINT ( 'NONE',  ( 16.20937500061451786, 4.119189519843966529, -2.378215178124998275 ) ) ;
#29224 = EDGE_CURVE ( 'NONE', #36937, #24863, #56652, .T. ) ;
#29225 = CYLINDRICAL_SURFACE ( 'NONE', #17296, 3.999999999999996447 ) ;
#29226 =( BOUNDED_CURVE ( )  B_SPLINE_CURVE ( 2, ( #46414, #51230, #12426, #17236, #62671, #11708, #17593 ),
 .UNSPECIFIED., .F., .F. ) 
 B_SPLINE_CURVE_WITH_KNOTS ( ( 3, 2, 2, 3 ),
 ( 0.5166666666666666075, 0.5194444444444443754, 0.5222222222222222543, 0.5250000000000000222 ),
 .UNSPECIFIED. ) 
 CURVE ( )  GEOMETRIC_REPRESENTATION_ITEM ( )  RATIONAL_B_SPLINE_CURVE ( ( 1.000000000000005329, 0.8660254037844333785, 1.000000000000000000, 0.8660254037844387076, 1.000000000000000000, 0.8660254037844387076, 1.000000000000000000 ) ) 
 REPRESENTATION_ITEM ( '' )  );
#29227 = CARTESIAN_POINT ( 'NONE',  ( 15.52500000000000036, 4.330127018922191873, 2.499999999999999556 ) ) ;
#29228 = EDGE_CURVE ( 'NONE', #9597, #55622, #54263, .T. ) ;
#29229 =( BOUNDED_CURVE ( )  B_SPLINE_CURVE ( 2, ( #9856, #19830, #32023, #54559, #49025 ),
 .UNSPECIFIED., .F., .F. ) 
 B_SPLINE_CURVE_WITH_KNOTS ( ( 3, 2, 3 ),
 ( 0.000000000000000000, 0.007246376811594202987, 0.01086956521739130578 ),
 .UNSPECIFIED. ) 
 CURVE ( )  GEOMETRIC_REPRESENTATION_ITEM ( )  RATIONAL_B_SPLINE_CURVE ( ( 1.000000000000000000, 0.8660254037844387076, 1.000000000000000000, 0.9330127018922192983, 0.9330127018922194093 ) ) 
 REPRESENTATION_ITEM ( '' )  );
#29230 = CARTESIAN_POINT ( 'NONE',  ( 15.27187500061451786, 3.027376345333613106, -5.243569643749998122 ) ) ;
#29231 = CARTESIAN_POINT ( 'NONE',  ( 11.70000000122903216, -2.886751345948129988, 4.999999999999997335 ) ) ;
#29232 = CARTESIAN_POINT ( 'NONE',  ( 18.12187500061451573, 3.027376345333611329, 5.243569643749999010 ) ) ;
#29233 = CARTESIAN_POINT ( 'NONE',  ( 17.69999999999999929, 4.330127018922192761, -2.499999999999997780 ) ) ;
#29234 = CARTESIAN_POINT ( 'NONE',  ( 21.87187500061451573, -6.054752690667223547, -1.112240025338166033E-15 ) ) ;
#29235 = CARTESIAN_POINT ( 'NONE',  ( -2.121784821874999949, 13.42812500061451786, -33.67503911421598417 ) ) ;
#29236 = DIRECTION ( 'NONE',  ( -1.000000000000000000, 0.000000000000000000, 0.000000000000000000 ) ) ;
#29237 = CARTESIAN_POINT ( 'NONE',  ( 24.04687500061451289, -4.119189519843965641, -2.378215178125001383 ) ) ;
#29238 = CARTESIAN_POINT ( 'NONE',  ( 34.99999999999999289, 2.500000000000000000, -3.500000000000000000 ) ) ;
#29239 = CARTESIAN_POINT ( 'NONE',  ( 24.06562500061451715, -6.054752690667223547, -1.112240025338166033E-15 ) ) ;
#29240 = CARTESIAN_POINT ( 'NONE',  ( 27.49687500061451217, 6.054752690667223547, 3.707466751127219781E-16 ) ) ;
#29241 = CARTESIAN_POINT ( 'NONE',  ( 25.27499999999999858, 6.123233995736764310E-16, -4.999999999999998224 ) ) ;
#29242 =( BOUNDED_CURVE ( )  B_SPLINE_CURVE ( 2, ( #27178, #54881, #49712, #4287, #71878, #21251, #43804, #11641, #1282 ),
 .UNSPECIFIED., .F., .F. ) 
 B_SPLINE_CURVE_WITH_KNOTS ( ( 3, 2, 2, 2, 3 ),
 ( 0.8194444444444444198, 0.8240740740740740700, 0.8333333333333333703, 0.8425925925925925597, 0.8472222222222222099 ),
 .UNSPECIFIED. ) 
 CURVE ( )  GEOMETRIC_REPRESENTATION_ITEM ( )  RATIONAL_B_SPLINE_CURVE ( ( 0.9330127018922194093, 0.9330127018922194093, 1.000000000000000000, 0.8660254037844387076, 1.000000000000000000, 0.8660254037844387076, 1.000000000000000000, 0.9330127018922194093, 0.9330127018922194093 ) ) 
 REPRESENTATION_ITEM ( '' )  );
#29243 = CARTESIAN_POINT ( 'NONE',  ( 7.603125000614517681, 4.541064518000418104, -2.621784821874998173 ) ) ;
#29244 = CARTESIAN_POINT ( 'NONE',  ( 25.95937500061451431, 2.746126346562645981, -4.756430356249997438 ) ) ;
#29245 = CARTESIAN_POINT ( 'NONE',  ( 19.13437500061451857, -4.541064518000419881, 2.621784821874995952 ) ) ;
#29246 = CARTESIAN_POINT ( 'NONE',  ( 11.85937500061451644, -5.492252693125287522, -1.008910452111647106E-15 ) ) ;
#29247 = CARTESIAN_POINT ( 'NONE',  ( 4.490625000614516971, 6.054752690667223547, 3.707466751127219781E-16 ) ) ;
#29248 = CARTESIAN_POINT ( 'NONE',  ( 9.534375000614517148, 4.541064518000418104, 2.621784821874999949 ) ) ;
#29249 = ORIENTED_EDGE ( 'NONE', *, *, #22798, .F. ) ;
#29250 = CARTESIAN_POINT ( 'NONE',  ( 18.64687500061451786, -3.027376345333614438, 5.243569643749998122 ) ) ;
#29251 = CARTESIAN_POINT ( 'NONE',  ( 13.80000000122903536, 5.773502691896255534, 3.535250795749688401E-16 ) ) ;
#29252 = CARTESIAN_POINT ( 'NONE',  ( 29.55000000000000071, 0.000000000000000000, 4.999999999999998224 ) ) ;
#29254 = EDGE_CURVE ( 'NONE', #40553, #49807, #33960, .T. ) ;
#29253 = CARTESIAN_POINT ( 'NONE',  ( 3.675000000000001155, 6.123233995736764310E-16, -4.999999999999998224 ) ) ;
#29255 = AXIS2_PLACEMENT_3D ( 'NONE', #7874, #70658, #20032 ) ;
#29256 = CARTESIAN_POINT ( 'NONE',  ( 45.00000000000000000, 6.123233995736764310E-16, -4.999999999999998224 ) ) ;
#29257 = ORIENTED_EDGE ( 'NONE', *, *, #55418, .T. ) ;
#29258 = CARTESIAN_POINT ( 'NONE',  ( 9.825000000000001066, -4.330127018922194537, 2.499999999999995559 ) ) ;
#29259 = CARTESIAN_POINT ( 'NONE',  ( 12.08437500061451608, 5.492252693125287522, 3.363034840372157021E-16 ) ) ;
#29260 = CARTESIAN_POINT ( 'NONE',  ( 24.29062500061451502, 6.054752690667223547, 3.707466751127219781E-16 ) ) ;
#29261 = CARTESIAN_POINT ( 'NONE',  ( 13.46249999999999858, -5.773502691896255534, -1.060575238724906372E-15 ) ) ;
#29262 = CARTESIAN_POINT ( 'NONE',  ( 10.76250000122903572, 0.000000000000000000, 4.999999999999998224 ) ) ;
#29263 = CARTESIAN_POINT ( 'NONE',  ( 8.953125000614518214, 4.541064518000418104, -2.621784821874998173 ) ) ;
#29264 = CARTESIAN_POINT ( 'NONE',  ( 25.05000000000000071, 0.000000000000000000, 4.999999999999998224 ) ) ;
#29265 = CARTESIAN_POINT ( 'NONE',  ( 20.72812500061451502, 4.541064518000418104, 2.621784821874999949 ) ) ;
#29266 = DIRECTION ( 'NONE',  ( 0.000000000000000000, 0.000000000000000000, 1.000000000000000000 ) ) ;
#29267 = CARTESIAN_POINT ( 'NONE',  ( 27.41250000122903430, 0.000000000000000000, 4.999999999999998224 ) ) ;
#29268 = CARTESIAN_POINT ( 'NONE',  ( -3.756430356249999214, 17.32812499938548356, 27.83122392262697176 ) ) ;
#29269 = CARTESIAN_POINT ( 'NONE',  ( 7.537500000000002309, -2.886751345948129988, 4.999999999999997335 ) ) ;
#29270 = ORIENTED_EDGE ( 'NONE', *, *, #27261, .T. ) ;
#29271 = CARTESIAN_POINT ( 'NONE',  ( 22.22812500061451502, -4.541064518000419881, 2.621784821874995952 ) ) ;
#29272 = CARTESIAN_POINT ( 'NONE',  ( 3.303520312748406962, -3.753280843300089487, -3.373494653866986770 ) ) ;
#29273 = CARTESIAN_POINT ( 'NONE',  ( 28.32187500061451502, 3.027376345333613106, -5.243569643749998122 ) ) ;
#29274 = CARTESIAN_POINT ( 'NONE',  ( 18.08437500061451431, 4.541064518000418104, 2.621784821874999949 ) ) ;
#29275 = CARTESIAN_POINT ( 'NONE',  ( 15.10312500061451502, -4.541064518000417216, -2.621784821875001281 ) ) ;
#29276 = FACE_OUTER_BOUND ( 'NONE', #51031, .T. ) ;
#29277 = CARTESIAN_POINT ( 'NONE',  ( 27.33750000122903145, 4.330127018922191873, 2.499999999999999556 ) ) ;
#29278 = CARTESIAN_POINT ( 'NONE',  ( 21.79687500061451644, -2.746126346562646425, 4.756430356249996549 ) ) ;
#29279 = CARTESIAN_POINT ( 'NONE',  ( 15.81562500061451537, 3.027376345333611329, 5.243569643749999010 ) ) ;
#29280 = CARTESIAN_POINT ( 'NONE',  ( 25.06875000122902719, 2.886751345948140646, 4.999999999999974243 ) ) ;
#29281 = CARTESIAN_POINT ( 'NONE',  ( 2.812500001229033320, -4.330127018922190985, -2.500000000000001332 ) ) ;
#29282 = CARTESIAN_POINT ( 'NONE',  ( 11.89687500061451608, -3.027376345333614438, 5.243569643749998122 ) ) ;
#29283 = CARTESIAN_POINT ( 'NONE',  ( 11.93437500061451573, -4.541064518000419881, 2.621784821874995952 ) ) ;
#29284 = CARTESIAN_POINT ( 'NONE',  ( 19.05937500061451928, 0.000000000000000000, 5.243569643749999010 ) ) ;
#29285 = ORIENTED_EDGE ( 'NONE', *, *, #23020, .T. ) ;
#29286 = CARTESIAN_POINT ( 'NONE',  ( 24.11250000122903359, 4.330127018922192761, -2.499999999999997780 ) ) ;
#29287 = CARTESIAN_POINT ( 'NONE',  ( 23.76562500061451644, 3.027376345333613106, -5.243569643749998122 ) ) ;
#29288 = CARTESIAN_POINT ( 'NONE',  ( 18.64687500061451786, -3.027376345333614438, 5.243569643749998122 ) ) ;
#29289 = CARTESIAN_POINT ( 'NONE',  ( 24.32812500061451289, 4.541064518000418104, 2.621784821874999949 ) ) ;
#29290 = CARTESIAN_POINT ( 'NONE',  ( 2.000000000000001332, 12.05000000000000249, -26.53589838486224650 ) ) ;
#29291 = CARTESIAN_POINT ( 'NONE',  ( -3.999999999999997335, 14.18750000000000000, 32.30940107675850470 ) ) ;
#29292 = CARTESIAN_POINT ( 'NONE',  ( 28.37812500061451715, 4.541064518000418104, 2.621784821874999949 ) ) ;
#29293 = CARTESIAN_POINT ( 'NONE',  ( 10.12500000122903465, 2.886751345948129099, -4.999999999999998224 ) ) ;
#29294 = CARTESIAN_POINT ( 'NONE',  ( 6.562500001229032875, 4.330127018922192761, -2.499999999999997780 ) ) ;
#29295 = FACE_OUTER_BOUND ( 'NONE', #52672, .T. ) ;
#29296 = CARTESIAN_POINT ( 'NONE',  ( 28.20000000122903216, 5.773502691896255534, 3.535250795749688894E-16 ) ) ;
#29297 = CARTESIAN_POINT ( 'NONE',  ( -3.756430356249999214, 13.39062499938548179, 27.83122392262697531 ) ) ;
#29298 = CARTESIAN_POINT ( 'NONE',  ( 16.29375000122903216, -2.886751345948125991, -5.000000000000000000 ) ) ;
#29299 = CARTESIAN_POINT ( 'NONE',  ( 8.709375000614517859, 0.000000000000000000, 5.243569643749999010 ) ) ;
#29300 = CARTESIAN_POINT ( 'NONE',  ( 1.626862140677534273E-15, 15.27500000122903501, 34.00000000000000000 ) ) ;
#29301 = CARTESIAN_POINT ( 'NONE',  ( 17.20312500061451644, 0.000000000000000000, 5.243569643749999010 ) ) ;
#29302 = CARTESIAN_POINT ( 'NONE',  ( 11.93437500061451573, -4.541064518000419881, 2.621784821874995952 ) ) ;
#29303 = CARTESIAN_POINT ( 'NONE',  ( 3.365625000614516082, -6.054752690667223547, -1.112240025338166033E-15 ) ) ;
#29304 = CARTESIAN_POINT ( 'NONE',  ( 19.32187500061451857, 3.027376345333612662, -5.243569643749998122 ) ) ;
#29305 = CARTESIAN_POINT ( 'NONE',  ( 7.321875000614516793, 3.027376345333611329, 5.243569643749999010 ) ) ;
#29306 = CARTESIAN_POINT ( 'NONE',  ( 2.840625000614518392, -3.027376345333614438, 5.243569643749998122 ) ) ;
#29307 = CARTESIAN_POINT ( 'NONE',  ( 10.65000000000000036, 0.000000000000000000, 4.999999999999998224 ) ) ;
#29308 = CARTESIAN_POINT ( 'NONE',  ( 7.415625000614516793, -6.054752690667223547, -1.112240025338166033E-15 ) ) ;
#29309 = CARTESIAN_POINT ( 'NONE',  ( 17.95312500061451644, 4.541064518000418104, -2.621784821874998173 ) ) ;
#29310 = EDGE_LOOP ( 'NONE', ( #21238, #37203, #55190 ) ) ;
#29311 = CARTESIAN_POINT ( 'NONE',  ( 5.137500001229033941, 6.123233995736764310E-16, -4.999999999999998224 ) ) ;
#29312 = CARTESIAN_POINT ( 'NONE',  ( 14.99062500061451786, -3.027376345333614438, 5.243569643749998122 ) ) ;
#29313 = CARTESIAN_POINT ( 'NONE',  ( 13.41562500061451502, 3.027376345333613106, -5.243569643749998122 ) ) ;
#29314 = CARTESIAN_POINT ( 'NONE',  ( 23.07187500061451857, 2.746126346562643317, 4.756430356249998326 ) ) ;
#29315 = CARTESIAN_POINT ( 'NONE',  ( 13.57500000000000107, 6.123233995736764310E-16, -4.999999999999998224 ) ) ;
#29316 = CARTESIAN_POINT ( 'NONE',  ( 7.800000001229035362, -2.886751345948125991, -5.000000000000000000 ) ) ;
#29317 = CARTESIAN_POINT ( 'NONE',  ( 4.678125000614516971, -4.541064518000419881, 2.621784821874995952 ) ) ;
#29318 = EDGE_CURVE ( 'NONE', #32246, #35438, #19283, .T. ) ;
#29319 = EDGE_CURVE ( 'NONE', #69237, #33272, #6589, .T. ) ;
#29320 = CARTESIAN_POINT ( 'NONE',  ( 19.65000000122902790, 5.773502691896255534, 3.535250795749688894E-16 ) ) ;
#29321 = CARTESIAN_POINT ( 'NONE',  ( 25.61250000000000071, -5.773502691896255534, -1.060575238724906372E-15 ) ) ;
#29322 = CARTESIAN_POINT ( 'NONE',  ( -3.000416591977282496E-16, 11.19687500061451679, -34.90005215228797653 ) ) ;
#29323 = CARTESIAN_POINT ( 'NONE',  ( 0.000000000000000000, 20.00000000000000000, 30.00000000000000000 ) ) ;
#29324 = CARTESIAN_POINT ( 'NONE',  ( 3.825000001229032609, 2.886751345948129099, -4.999999999999998224 ) ) ;
#29325 = DIRECTION ( 'NONE',  ( 0.000000000000000000, 0.000000000000000000, 1.000000000000000000 ) ) ;
#29326 = DIRECTION ( 'NONE',  ( 0.000000000000000000, 0.000000000000000000, 1.000000000000000000 ) ) ;
#29327 = CARTESIAN_POINT ( 'NONE',  ( 17.74687500061451928, -3.027376345333614438, 5.243569643749998122 ) ) ;
#29328 = LINE ( 'NONE', #69220, #20929 ) ;
#29329 = CARTESIAN_POINT ( 'NONE',  ( 14.69062500061451537, -3.027376345333610441, -5.243569643749999898 ) ) ;
#29330 = CARTESIAN_POINT ( 'NONE',  ( 8.568750001229034297, -5.773502691896255534, -1.060575238724906372E-15 ) ) ;
#29331 = CARTESIAN_POINT ( 'NONE',  ( 15.93750000122903110, 6.123233995736764310E-16, -4.999999999999998224 ) ) ;
#29332 = CARTESIAN_POINT ( 'NONE',  ( 25.92187500061451999, -6.054752690667223547, -1.112240025338166033E-15 ) ) ;
#29333 = CARTESIAN_POINT ( 'NONE',  ( 17.22187500061451360, -4.119189519843968306, 2.378215178124996054 ) ) ;
#29334 = CARTESIAN_POINT ( 'NONE',  ( 13.15312500061451750, 0.000000000000000000, 5.243569643749999010 ) ) ;
#29335 = CARTESIAN_POINT ( 'NONE',  ( 15.38437500061451679, 4.541064518000418104, 2.621784821874999949 ) ) ;
#29336 = ORIENTED_EDGE ( 'NONE', *, *, #9782, .T. ) ;
#29337 = CARTESIAN_POINT ( 'NONE',  ( 28.52812500061451573, -4.541064518000419881, 2.621784821874995952 ) ) ;
#29338 = CARTESIAN_POINT ( 'NONE',  ( 21.40312500061451573, -4.541064518000417216, -2.621784821875001281 ) ) ;
#29339 = CARTESIAN_POINT ( 'NONE',  ( 29.24062500061451431, 6.054752690667223547, 3.707466751127219781E-16 ) ) ;
#29340 = CARTESIAN_POINT ( 'NONE',  ( 3.999999999999999112, 15.38750000122903394, -30.00000000000000000 ) ) ;
#29341 = CARTESIAN_POINT ( 'NONE',  ( 10.46249999999999858, 2.886751345948129099, -4.999999999999998224 ) ) ;
#29342 = CARTESIAN_POINT ( 'NONE',  ( 20.02500000122903145, 2.886751345948129099, -4.999999999999998224 ) ) ;
#29343 = DIRECTION ( 'NONE',  ( -1.000000000000000000, -0.000000000000000000, -0.000000000000000000 ) ) ;
#29344 = CARTESIAN_POINT ( 'NONE',  ( 10.13437500061451502, -2.746126346562642428, -4.756430356249999214 ) ) ;
#29345 = ORIENTED_EDGE ( 'NONE', *, *, #24132, .F. ) ;
#29346 = CARTESIAN_POINT ( 'NONE',  ( 17.81250000000000355, 2.886751345948126879, 4.999999999999999112 ) ) ;
#29347 = CARTESIAN_POINT ( 'NONE',  ( 20.36249999999999716, 2.886751345948129099, -4.999999999999998224 ) ) ;
#29348 = CARTESIAN_POINT ( 'NONE',  ( 18.90937500061451360, 4.541064518000418104, -2.621784821874998173 ) ) ;
#29349 = CARTESIAN_POINT ( 'NONE',  ( 25.60312500061451502, 4.541064518000418104, -2.621784821874998173 ) ) ;
#29350 = ORIENTED_EDGE ( 'NONE', *, *, #3296, .T. ) ;
#29351 = CARTESIAN_POINT ( 'NONE',  ( 13.57500000000000107, 6.123233995736764310E-16, -4.999999999999998224 ) ) ;
#29352 = CARTESIAN_POINT ( 'NONE',  ( 8.503125000614515372, 4.541064518000418104, -2.621784821874998173 ) ) ;
#29353 = CARTESIAN_POINT ( 'NONE',  ( 3.196875000614517237, 6.054752690667223547, 3.707466751127219781E-16 ) ) ;
#29354 = CARTESIAN_POINT ( 'NONE',  ( 14.69999999999999929, 0.000000000000000000, 4.999999999999998224 ) ) ;
#29355 = CARTESIAN_POINT ( 'NONE',  ( 2.121784821874999061, 17.40312500061451573, 26.32496088578401583 ) ) ;
#29356 = CARTESIAN_POINT ( 'NONE',  ( 29.20312500061451644, 4.541064518000418104, -2.621784821874998173 ) ) ;
#29357 = CARTESIAN_POINT ( 'NONE',  ( 9.787499999999999645, -2.886751345948129988, 4.999999999999997335 ) ) ;
#29358 = CARTESIAN_POINT ( 'NONE',  ( -7.967954043666661671E-16, 16.12812499938548427, 34.33755215474603517 ) ) ;
#29359 = CARTESIAN_POINT ( 'NONE',  ( 25.28437500061451715, 4.541064518000418104, 2.621784821874999949 ) ) ;
#29360 = ORIENTED_EDGE ( 'NONE', *, *, #71944, .F. ) ;
#29361 = CARTESIAN_POINT ( 'NONE',  ( 21.40312500061451573, -4.541064518000417216, -2.621784821875001281 ) ) ;
#29362 = CARTESIAN_POINT ( 'NONE',  ( 23.82187500061451502, 3.027376345333613106, -5.243569643749998122 ) ) ;
#29363 = EDGE_CURVE ( 'NONE', #31619, #66176, #11083, .T. ) ;
#29364 = CARTESIAN_POINT ( 'NONE',  ( -4.243569643749998122, 16.69062500061459531, -27.54997392385601174 ) ) ;
#29365 = CARTESIAN_POINT ( 'NONE',  ( 11.28749999999999787, -2.886751345948125991, -5.000000000000000000 ) ) ;
#29366 = CARTESIAN_POINT ( 'NONE',  ( 9.290625000614515017, -3.027376345333610441, -5.243569643749999898 ) ) ;
#29367 = CARTESIAN_POINT ( 'NONE',  ( 3.750000000000000000, 4.330127018922192761, -2.499999999999997780 ) ) ;
#29368 = CARTESIAN_POINT ( 'NONE',  ( 24.77812500061451217, 4.541064518000418104, 2.621784821874999949 ) ) ;
#29369 = CARTESIAN_POINT ( 'NONE',  ( 27.00937500061451502, 2.746126346562643317, 4.756430356249998326 ) ) ;
#29370 = CARTESIAN_POINT ( 'NONE',  ( 12.27187500061451786, 2.746126346562643317, 4.756430356249998326 ) ) ;
#29371 = CARTESIAN_POINT ( 'NONE',  ( 19.17187500061451999, -6.054752690667223547, -1.112240025338166033E-15 ) ) ;
#29372 = CARTESIAN_POINT ( 'NONE',  ( 2.121784821875001281, 12.80937500061451928, 33.67503911421598417 ) ) ;
#29373 = CARTESIAN_POINT ( 'NONE',  ( 20.37187500061451573, 3.027376345333611329, 5.243569643749999010 ) ) ;
#29374 = CARTESIAN_POINT ( 'NONE',  ( 27.94687500061451502, 6.054752690667223547, 3.707466751127219781E-16 ) ) ;
#29375 = CARTESIAN_POINT ( 'NONE',  ( 4.243569643749999010, 16.52187500061451786, 27.54997392385601174 ) ) ;
#29376 = CARTESIAN_POINT ( 'NONE',  ( 7.340625000614518392, -3.027376345333614438, 5.243569643749998122 ) ) ;
#29377 = CARTESIAN_POINT ( 'NONE',  ( 1.999999999999998668, 10.51250000122903572, -33.46410161513775705 ) ) ;
#29378 = CARTESIAN_POINT ( 'NONE',  ( 3.459375000614519635, -4.541064518000417216, -2.621784821875001281 ) ) ;
#29379 = CARTESIAN_POINT ( 'NONE',  ( 26.02500000122903145, 2.886751345948110892, 5.000000000000026645 ) ) ;
#29380 = CARTESIAN_POINT ( 'NONE',  ( 4.790625000614518569, -3.027376345333610441, -5.243569643749999898 ) ) ;
#29381 = CARTESIAN_POINT ( 'NONE',  ( 8.746875000614515727, -3.027376345333614438, 5.243569643749998122 ) ) ;
#29382 = CARTESIAN_POINT ( 'NONE',  ( 15.63750000122903216, 4.330127018922191873, 2.499999999999999556 ) ) ;
#29383 = CARTESIAN_POINT ( 'NONE',  ( 6.534375000614517148, -4.541064518000419881, 2.621784821874995952 ) ) ;
#29384 = CARTESIAN_POINT ( 'NONE',  ( 6.815625000614517148, 3.027376345333611329, 5.243569643749999010 ) ) ;
#29385 = CYLINDRICAL_SURFACE ( 'NONE', #33944, 4.999999999999998224 ) ;
#29386 = CARTESIAN_POINT ( 'NONE',  ( 23.00625000122903430, -4.330127018922190985, -2.500000000000001332 ) ) ;
#29387 = CARTESIAN_POINT ( 'NONE',  ( 17.63437500061451502, 4.541064518000418104, 2.621784821874999949 ) ) ;
#29388 = CARTESIAN_POINT ( 'NONE',  ( 1.626862140677534470E-15, 13.68124999877096748, 34.00000000000000000 ) ) ;
#29389 = VERTEX_POINT ( 'NONE', #38435 ) ;
#29390 = CARTESIAN_POINT ( 'NONE',  ( 25.75312500061451715, 0.000000000000000000, 5.243569643749999010 ) ) ;
#29391 = CARTESIAN_POINT ( 'NONE',  ( 10.11562500061451608, -6.054752690667223547, -1.112240025338166033E-15 ) ) ;
#29392 = CARTESIAN_POINT ( 'NONE',  ( 26.40937500061451715, -4.541064518000417216, -2.621784821875001281 ) ) ;
#29393 = CARTESIAN_POINT ( 'NONE',  ( 9.740625000614516082, -3.027376345333610441, -5.243569643749999898 ) ) ;
#29394 = LINE ( 'NONE', #34562, #62754 ) ;
#29395 = CARTESIAN_POINT ( 'NONE',  ( 11.43750000122903465, 6.123233995736764310E-16, -4.999999999999998224 ) ) ;
#29396 = CARTESIAN_POINT ( 'NONE',  ( 26.16562500061451502, 3.027376345333611329, 5.243569643749999010 ) ) ;
#29397 = CARTESIAN_POINT ( 'NONE',  ( 4.243569643749999898, 13.69062500061451537, -27.54997392385601529 ) ) ;
#29398 = CARTESIAN_POINT ( 'NONE',  ( 12.00000000122903465, 5.773502691896255534, 3.535250795749688894E-16 ) ) ;
#29399 = CARTESIAN_POINT ( 'NONE',  ( 21.51562500061451644, 3.027376345333613106, -5.243569643749998122 ) ) ;
#29400 = CARTESIAN_POINT ( 'NONE',  ( 12.07499999999999929, -4.330127018922194537, 2.499999999999995559 ) ) ;
#29401 = CARTESIAN_POINT ( 'NONE',  ( 20.65312500061451573, 4.541064518000418104, -2.621784821874998173 ) ) ;
#29402 = CARTESIAN_POINT ( 'NONE',  ( 5.296875000614517326, -3.027376345333610441, -5.243569643749999898 ) ) ;
#29403 = CARTESIAN_POINT ( 'NONE',  ( 20.81250000000000000, 2.886751345948129099, -4.999999999999998224 ) ) ;
#29404 = CARTESIAN_POINT ( 'NONE',  ( 7.050000001229036251, 5.773502691896255534, 3.535250795749688894E-16 ) ) ;
#29405 = CARTESIAN_POINT ( 'NONE',  ( 15.15000000122903323, 5.773502691896255534, 3.535250795749688894E-16 ) ) ;
#29406 = CARTESIAN_POINT ( 'NONE',  ( 12.51562500061451821, 3.027376345333613106, -5.243569643749998122 ) ) ;
#29407 = CARTESIAN_POINT ( 'NONE',  ( 16.67812500061451786, 4.541064518000418104, 2.621784821874999949 ) ) ;
#29408 = EDGE_CURVE ( 'NONE', #16877, #57346, #10057, .T. ) ;
#29409 = CARTESIAN_POINT ( 'NONE',  ( 25.80000000122903714, -2.886751345948125991, -5.000000000000000000 ) ) ;
#29410 = CARTESIAN_POINT ( 'NONE',  ( 19.53749999999999432, 5.773502691896255534, 3.535250795749688894E-16 ) ) ;
#29411 = CARTESIAN_POINT ( 'NONE',  ( 23.89687500061451786, 6.054752690667223547, 3.707466751127219781E-16 ) ) ;
#29412 = CARTESIAN_POINT ( 'NONE',  ( -5.000000000000004441, 6.123233995736764310E-16, -4.999999999999998224 ) ) ;
#29413 = CARTESIAN_POINT ( 'NONE',  ( 9.337500001229033231, 4.330127018922191873, 2.499999999999999556 ) ) ;
#29414 = CARTESIAN_POINT ( 'NONE',  ( 7.734375000614517326, 4.541064518000418104, 2.621784821874999949 ) ) ;
#29415 = CARTESIAN_POINT ( 'NONE',  ( 25.05937500061451573, -4.541064518000417216, -2.621784821875001281 ) ) ;
#29416 = CARTESIAN_POINT ( 'NONE',  ( 23.92499999999999716, 6.123233995736764310E-16, -4.999999999999998224 ) ) ;
#29417 = CARTESIAN_POINT ( 'NONE',  ( 21.66562500061451502, 3.027376345333611329, 5.243569643749999010 ) ) ;
#29418 = CARTESIAN_POINT ( 'NONE',  ( 26.70937500061451431, 0.000000000000000000, 5.243569643749999010 ) ) ;
#29419 = CARTESIAN_POINT ( 'NONE',  ( -3.756430356249999214, 17.89062499938548356, 27.83122392262697176 ) ) ;
#29420 = CARTESIAN_POINT ( 'NONE',  ( 8.746875000614515727, -3.027376345333614438, 5.243569643749998122 ) ) ;
#29421 = CARTESIAN_POINT ( 'NONE',  ( 19.97812500061451502, -4.541064518000419881, 2.621784821874995952 ) ) ;
#29422 = VERTEX_POINT ( 'NONE', #60960 ) ;
#29423 = CARTESIAN_POINT ( 'NONE',  ( 27.74062500061451431, -3.027376345333610441, -5.243569643749999898 ) ) ;
#29424 = CARTESIAN_POINT ( 'NONE',  ( 5.071875000614519458, 3.027376345333611329, 5.243569643749999010 ) ) ;
#29425 = CARTESIAN_POINT ( 'NONE',  ( 22.72500000122903785, 2.886751345948162850, -4.999999999999940492 ) ) ;
#29426 = CARTESIAN_POINT ( 'NONE',  ( 30.00000000000000000, 0.000000000000000000, 4.999999999999998224 ) ) ;
#29427 = CARTESIAN_POINT ( 'NONE',  ( 16.68750000000000000, -2.886751345948125991, -5.000000000000000000 ) ) ;
#29428 = VERTEX_POINT ( 'NONE', #44719 ) ;
#29429 = CARTESIAN_POINT ( 'NONE',  ( 24.03750000000000142, 5.773502691896255534, 3.535250795749688894E-16 ) ) ;
#29430 = CARTESIAN_POINT ( 'NONE',  ( 26.33437500061451431, -4.541064518000419881, 2.621784821874995952 ) ) ;
#29431 = VERTEX_POINT ( 'NONE', #16254 ) ;
#29432 = CARTESIAN_POINT ( 'NONE',  ( 15.96562500061451573, -6.054752690667223547, -1.112240025338166033E-15 ) ) ;
#29433 = CARTESIAN_POINT ( 'NONE',  ( 6.178125000614518747, 6.421520780324663323E-16, -5.243569643749999010 ) ) ;
#29434 = CARTESIAN_POINT ( 'NONE',  ( 19.77187500061451786, 4.119189519843966529, 2.378215178124999607 ) ) ;
#29435 = CARTESIAN_POINT ( 'NONE',  ( 29.72812500061451502, 4.541064518000418104, 2.621784821874999949 ) ) ;
#29436 = CARTESIAN_POINT ( 'NONE',  ( 15.45000000122903216, -2.886751345948125991, -5.000000000000000000 ) ) ;
#29437 = CARTESIAN_POINT ( 'NONE',  ( 20.99999999999999645, 0.000000000000000000, 4.999999999999998224 ) ) ;
#29438 = CARTESIAN_POINT ( 'NONE',  ( 28.31250000000000000, -5.773502691896255534, -1.060575238724906372E-15 ) ) ;
#29439 = CARTESIAN_POINT ( 'NONE',  ( 5.559375000614517504, 0.000000000000000000, 5.243569643749999010 ) ) ;
#29440 = CARTESIAN_POINT ( 'NONE',  ( 9.496875000614517504, 6.054752690667223547, 3.707466751127219781E-16 ) ) ;
#29441 = CARTESIAN_POINT ( 'NONE',  ( 19.50937500061451857, 0.000000000000000000, 5.243569643749999010 ) ) ;
#29442 = ORIENTED_EDGE ( 'NONE', *, *, #4248, .T. ) ;
#29443 = CARTESIAN_POINT ( 'NONE',  ( 5.184375000614516615, -4.541064518000419881, 2.621784821874995952 ) ) ;
#29444 = CARTESIAN_POINT ( 'NONE',  ( 3.487500000000000711, -2.886751345948129988, 4.999999999999997335 ) ) ;
#29445 = CARTESIAN_POINT ( 'NONE',  ( 5.634375000614519458, -4.541064518000419881, 2.621784821874995952 ) ) ;
#29446 = CARTESIAN_POINT ( 'NONE',  ( 18.78749999999999432, -2.886751345948129988, 4.999999999999997335 ) ) ;
#29447 = CARTESIAN_POINT ( 'NONE',  ( 15.96562500061451573, -6.054752690667223547, -1.112240025338166033E-15 ) ) ;
#29448 = CARTESIAN_POINT ( 'NONE',  ( -3.999999999999999556, 19.43750000000000000, 27.69059892324149175 ) ) ;
#29449 = CARTESIAN_POINT ( 'NONE',  ( 45.00000000000000000, 0.000000000000000000, 4.999999999999998224 ) ) ;
#29450 = CARTESIAN_POINT ( 'NONE',  ( 19.88437500061451857, 4.119189519843966529, 2.378215178124999607 ) ) ;
#29451 = CARTESIAN_POINT ( 'NONE',  ( 9.065625000614517148, 3.027376345333611329, 5.243569643749999010 ) ) ;
#29452 = CARTESIAN_POINT ( 'NONE',  ( 27.08437500061451786, 4.541064518000418104, 2.621784821874999949 ) ) ;
#29453 = CARTESIAN_POINT ( 'NONE',  ( 2.121784821874999061, 18.80937500061451928, 26.32496088578401583 ) ) ;
#29454 = CARTESIAN_POINT ( 'NONE',  ( 27.19687500061451857, -3.027376345333614438, 5.243569643749998122 ) ) ;
#29455 = CARTESIAN_POINT ( 'NONE',  ( 7.912499999999999645, 2.886751345948126879, 4.999999999999999112 ) ) ;
#29456 = CARTESIAN_POINT ( 'NONE',  ( 3.999999999999999112, 12.23750000122903359, 30.00000000000000000 ) ) ;
#29457 = CARTESIAN_POINT ( 'NONE',  ( 15.77812500061451573, 4.541064518000418104, 2.621784821874999949 ) ) ;
#29459 =( BOUNDED_CURVE ( )  B_SPLINE_CURVE ( 2, ( #30367, #2655, #66081, #65715, #15101, #54634, #7465, #64338, #24084 ),
 .UNSPECIFIED., .F., .F. ) 
 B_SPLINE_CURVE_WITH_KNOTS ( ( 3, 2, 2, 2, 3 ),
 ( 0.3472222222222222654, 0.3518518518518518601, 0.3611111111111111049, 0.3703703703703703498, 0.3750000000000000000 ),
 .UNSPECIFIED. ) 
 CURVE ( )  GEOMETRIC_REPRESENTATION_ITEM ( )  RATIONAL_B_SPLINE_CURVE ( ( 0.9330127018922194093, 0.9330127018922197424, 1.000000000000000000, 0.8660254037844387076, 1.000000000000000000, 0.8660254037844387076, 1.000000000000000000, 0.9330127018922194093, 0.9330127018922194093 ) ) 
 REPRESENTATION_ITEM ( '' )  );
#29458 = CARTESIAN_POINT ( 'NONE',  ( 7.350000001229033408, -2.886751345948125991, -5.000000000000000000 ) ) ;
#29460 = CARTESIAN_POINT ( 'NONE',  ( 18.27187500061451431, -6.054752690667223547, -1.112240025338166033E-15 ) ) ;
#29461 = CARTESIAN_POINT ( 'NONE',  ( 11.67187500061451821, 3.027376345333613106, -5.243569643749998122 ) ) ;
#29462 = CARTESIAN_POINT ( 'NONE',  ( -2.506492529888154408, 4.347006505069263227, -33.15646410307740410 ) ) ;
#29463 = ORIENTED_EDGE ( 'NONE', *, *, #40217, .F. ) ;
#29464 = CARTESIAN_POINT ( 'NONE',  ( 12.74062500061451786, -3.027376345333614438, 5.243569643749998122 ) ) ;
#29465 = CARTESIAN_POINT ( 'NONE',  ( 24.93750000122903288, 6.123233995736764310E-16, -4.999999999999998224 ) ) ;
#29466 = CARTESIAN_POINT ( 'NONE',  ( 13.17187500061451999, 3.027376345333611329, 5.243569643749999010 ) ) ;
#29467 = CARTESIAN_POINT ( 'NONE',  ( 20.78732959644809952, -4.500000000000000000, -5.500000000000000000 ) ) ;
#29468 = CARTESIAN_POINT ( 'NONE',  ( 15.74062500061451608, 6.054752690667223547, 3.707466751127219781E-16 ) ) ;
#29469 = CARTESIAN_POINT ( 'NONE',  ( 20.78732959644809952, -2.499999999999999556, -3.499999999999999556 ) ) ;
#29470 = CARTESIAN_POINT ( 'NONE',  ( 23.70937500061451786, -4.541064518000417216, -2.621784821875001281 ) ) ;
#29471 = DIRECTION ( 'NONE',  ( 0.000000000000000000, 0.000000000000000000, -1.000000000000000000 ) ) ;
#29472 = CARTESIAN_POINT ( 'NONE',  ( 11.73750000122903181, -4.330127018922194537, 2.499999999999995559 ) ) ;
#29473 = CARTESIAN_POINT ( 'NONE',  ( 7.659375000614518036, 4.119189519843966529, -2.378215178124998275 ) ) ;
#29474 = CYLINDRICAL_SURFACE ( 'NONE', #38362, 4.999999999999998224 ) ;
#29475 = CARTESIAN_POINT ( 'NONE',  ( -3.000416591977282496E-16, 17.04687500061451999, -34.90005215228797653 ) ) ;
#29476 = CARTESIAN_POINT ( 'NONE',  ( 17.63437500061451502, 4.541064518000418104, 2.621784821874999949 ) ) ;
#29477 = CARTESIAN_POINT ( 'NONE',  ( 18.78750000122903430, 4.330127018922191873, 2.499999999999999556 ) ) ;
#29478 = CARTESIAN_POINT ( 'NONE',  ( 13.47187500061451537, 3.027376345333613106, -5.243569643749998122 ) ) ;
#29479 = ADVANCED_FACE ( 'NONE', ( #66508 ), #61325, .F. ) ;
#29480 = CARTESIAN_POINT ( 'NONE',  ( -3.000416591977282496E-16, 10.74687500061451928, 25.09994784771203058 ) ) ;
#29481 = CARTESIAN_POINT ( 'NONE',  ( 20.58750000122903145, 4.330127018922191873, 2.499999999999999556 ) ) ;
#29482 = CARTESIAN_POINT ( 'NONE',  ( 14.24062500061451608, -3.027376345333610441, -5.243569643749999898 ) ) ;
#29483 = ORIENTED_EDGE ( 'NONE', *, *, #71543, .F. ) ;
#29484 = VERTEX_POINT ( 'NONE', #55793 ) ;
#29485 = CARTESIAN_POINT ( 'NONE',  ( 18.11250000000000071, 2.886751345948129099, -4.999999999999998224 ) ) ;
#29486 = CARTESIAN_POINT ( 'NONE',  ( 3.590625000614518836, 6.054752690667223547, 3.707466751127219781E-16 ) ) ;
#29487 = CARTESIAN_POINT ( 'NONE',  ( 14.32500000122903394, 2.886751345948126879, 4.999999999999999112 ) ) ;
#29488 = CARTESIAN_POINT ( 'NONE',  ( 26.89687500061451431, -3.027376345333610441, -5.243569643749999898 ) ) ;
#29489 = CARTESIAN_POINT ( 'NONE',  ( 20.05312500061451431, -4.541064518000417216, -2.621784821875001281 ) ) ;
#29490 = CARTESIAN_POINT ( 'NONE',  ( 23.69062500061451004, -3.027376345333610441, -5.243569643749999898 ) ) ;
#29491 = CARTESIAN_POINT ( 'NONE',  ( 3.028125000614518392, 6.421520780324663323E-16, -5.243569643749999010 ) ) ;
#29492 = EDGE_CURVE ( 'NONE', #15264, #21571, #33611, .T. ) ;
#29493 = CARTESIAN_POINT ( 'NONE',  ( 26.51249999999999929, -5.773502691896255534, -1.060575238724906372E-15 ) ) ;
#29494 = CARTESIAN_POINT ( 'NONE',  ( 4.650000000000001243, 4.330127018922192761, -2.499999999999997780 ) ) ;
#29495 = CARTESIAN_POINT ( 'NONE',  ( 8.146875000614516082, 5.492252693125287522, 3.363034840372157021E-16 ) ) ;
#29496 = DIRECTION ( 'NONE',  ( -0.000000000000000000, -1.000000000000000000, -0.000000000000000000 ) ) ;
#29497 = CYLINDRICAL_SURFACE ( 'NONE', #61854, 4.999999999999998224 ) ;
#29498 = CARTESIAN_POINT ( 'NONE',  ( 9.001249775931846008E-16, 15.92187500061451821, -25.09994784771203058 ) ) ;
#29499 = CARTESIAN_POINT ( 'NONE',  ( 5.475000001229035185, -5.773502691896255534, -1.060575238724906372E-15 ) ) ;
#29500 = CARTESIAN_POINT ( 'NONE',  ( 5.287500000000000533, -2.886751345948129988, 4.999999999999997335 ) ) ;
#29501 = ADVANCED_FACE ( 'NONE', ( #39532 ), #67969, .F. ) ;
#29502 = CARTESIAN_POINT ( 'NONE',  ( 4.125000001229034652, -5.773502691896255534, -1.060575238724906372E-15 ) ) ;
#29503 = CARTESIAN_POINT ( 'NONE',  ( 8.746875000614515727, -3.027376345333614438, 5.243569643749998122 ) ) ;
#29504 = CARTESIAN_POINT ( 'NONE',  ( 28.41562500061451502, 3.027376345333611329, 5.243569643749999010 ) ) ;
#29505 = CARTESIAN_POINT ( 'NONE',  ( 4.000000000000000000, 10.73750000000000071, 32.30940107675849760 ) ) ;
#29506 = CARTESIAN_POINT ( 'NONE',  ( 5.475000001229035185, -5.773502691896255534, -1.060575238724906372E-15 ) ) ;
#29507 = CARTESIAN_POINT ( 'NONE',  ( 12.65625000122903110, -4.330127018922190985, -2.500000000000001332 ) ) ;
#29508 = CARTESIAN_POINT ( 'NONE',  ( 7.584375000614516082, 6.421520780324663323E-16, -5.243569643749999010 ) ) ;
#29509 = CARTESIAN_POINT ( 'NONE',  ( 11.03437500061451715, -4.541064518000419881, 2.621784821874995952 ) ) ;
#29510 = CARTESIAN_POINT ( 'NONE',  ( 6.524999999999999467, 4.330127018922191873, 2.499999999999999556 ) ) ;
#29511 = CARTESIAN_POINT ( 'NONE',  ( 2.121784821875001281, 15.45312500061459460, 33.67503911421598417 ) ) ;
#29512 = CARTESIAN_POINT ( 'NONE',  ( 21.68437500061451573, 4.541064518000418104, 2.621784821874999949 ) ) ;
#29513 = CARTESIAN_POINT ( 'NONE',  ( 0.000000000000000000, 25.54316770519903557, 26.00000000000000000 ) ) ;
#29514 = CARTESIAN_POINT ( 'NONE',  ( 5.700000000000000178, 0.000000000000000000, 4.999999999999998224 ) ) ;
#29515 = CARTESIAN_POINT ( 'NONE',  ( 27.41250000122903430, 0.000000000000000000, 4.999999999999998224 ) ) ;
#29516 = CARTESIAN_POINT ( 'NONE',  ( 17.25937500061451502, -5.492252693125287522, -1.008910452111647106E-15 ) ) ;
#29517 = CARTESIAN_POINT ( 'NONE',  ( 23.50312500061451360, 0.000000000000000000, 5.243569643749999010 ) ) ;
#29518 = CARTESIAN_POINT ( 'NONE',  ( 11.95312500061451644, -4.541064518000417216, -2.621784821875001281 ) ) ;
#29519 = CARTESIAN_POINT ( 'NONE',  ( 26.70937500061451431, -5.492252693125287522, -1.008910452111647106E-15 ) ) ;
#29520 = CARTESIAN_POINT ( 'NONE',  ( 12.45937500061451786, -4.541064518000417216, -2.621784821875001281 ) ) ;
#29521 = CARTESIAN_POINT ( 'NONE',  ( 28.98750000000000071, 5.773502691896255534, 3.535250795749688894E-16 ) ) ;
#29522 = CARTESIAN_POINT ( 'NONE',  ( 22.05000000122903714, -2.886751345948129988, 4.999999999999997335 ) ) ;
#29523 = CARTESIAN_POINT ( 'NONE',  ( 45.00000000000000000, 2.500000000000000444, 3.499999999999999112 ) ) ;
#29524 = CARTESIAN_POINT ( 'NONE',  ( 10.65937500061451715, -4.541064518000417216, -2.621784821875001281 ) ) ;
#29525 = CARTESIAN_POINT ( 'NONE',  ( 29.52187500061451431, -6.054752690667223547, -1.112240025338166033E-15 ) ) ;
#29526 = CARTESIAN_POINT ( 'NONE',  ( 2.896875000614518747, -3.027376345333614438, 5.243569643749998122 ) ) ;
#29527 = DIRECTION ( 'NONE',  ( 0.000000000000000000, 0.000000000000000000, 1.000000000000000000 ) ) ;
#29528 = CARTESIAN_POINT ( 'NONE',  ( 23.14687500061451786, -3.027376345333614438, 5.243569643749998122 ) ) ;
#29529 = CARTESIAN_POINT ( 'NONE',  ( 14.48437500061451821, 4.541064518000418104, 2.621784821874999949 ) ) ;
#29530 = CARTESIAN_POINT ( 'NONE',  ( 2.655984681222220721E-16, 18.26562499938548356, 25.66244784525396483 ) ) ;
#29531 = CARTESIAN_POINT ( 'NONE',  ( 26.77499999999999858, 4.330127018922191873, 2.499999999999999556 ) ) ;
#29532 = CARTESIAN_POINT ( 'NONE',  ( -1.999999999999999112, 12.65000000000000213, 26.53589838486224650 ) ) ;
#29533 = CARTESIAN_POINT ( 'NONE',  ( 27.64687500061452141, -2.746126346562646425, 4.756430356249996549 ) ) ;
#29534 = CARTESIAN_POINT ( 'NONE',  ( 17.12812500061451715, 4.541064518000418104, 2.621784821874999949 ) ) ;
#29535 = CARTESIAN_POINT ( 'NONE',  ( 7.500000000000000000, 0.000000000000000000, 4.999999999999998224 ) ) ;
#29536 = CARTESIAN_POINT ( 'NONE',  ( 12.15000000122903145, -2.886751345948063374, 5.000000000000112799 ) ) ;
#29537 = CARTESIAN_POINT ( 'NONE',  ( 15.26249999999999929, -5.773502691896255534, -1.060575238724906372E-15 ) ) ;
#29538 = CARTESIAN_POINT ( 'NONE',  ( 9.001249775931846008E-16, 10.46562500061451928, 34.90005215228797653 ) ) ;
#29539 = CARTESIAN_POINT ( 'NONE',  ( -4.000000000000000000, 19.47499999999999787, 30.00000000000000000 ) ) ;
#29540 = CARTESIAN_POINT ( 'NONE',  ( 25.69687500061451502, 6.054752690667223547, 3.707466751127219781E-16 ) ) ;
#29541 = VERTEX_POINT ( 'NONE', #19 ) ;
#29542 = CARTESIAN_POINT ( 'NONE',  ( 20.27812500061451573, 4.541064518000418104, 2.621784821874999949 ) ) ;
#29543 = CARTESIAN_POINT ( 'NONE',  ( 20.70937500061451786, 4.541064518000418104, -2.621784821874998173 ) ) ;
#29544 = CARTESIAN_POINT ( 'NONE',  ( 3.187500000000002220, -2.886751345948125991, -5.000000000000000000 ) ) ;
#29545 = CARTESIAN_POINT ( 'NONE',  ( 7.603125000614517681, 4.541064518000418104, -2.621784821874998173 ) ) ;
#29546 = CARTESIAN_POINT ( 'NONE',  ( 20.80312500061451431, 0.000000000000000000, 5.243569643749999010 ) ) ;
#29547 = CARTESIAN_POINT ( 'NONE',  ( 12.30937500061451573, 0.000000000000000000, 5.243569643749999010 ) ) ;
#29548 = CARTESIAN_POINT ( 'NONE',  ( 16.39687500061451786, -3.027376345333614438, 5.243569643749998122 ) ) ;
#29549 = CARTESIAN_POINT ( 'NONE',  ( -2.121784821874999949, 16.57812500061451644, 26.32496088578401938 ) ) ;
#29550 = CARTESIAN_POINT ( 'NONE',  ( 20.17500000122903359, 2.886751345948126879, 4.999999999999999112 ) ) ;
#29551 = CARTESIAN_POINT ( 'NONE',  ( 14.10937500061451644, 0.000000000000000000, 4.756430356249998326 ) ) ;
#29552 = CARTESIAN_POINT ( 'NONE',  ( 8.653125000614515727, 0.000000000000000000, 5.243569643749999010 ) ) ;
#29553 = CARTESIAN_POINT ( 'NONE',  ( 3.384375000614517237, -4.541064518000419881, 2.621784821874995952 ) ) ;
#29554 = CARTESIAN_POINT ( 'NONE',  ( 4.959375000614516971, 4.541064518000418104, -2.621784821874998173 ) ) ;
#29555 = CARTESIAN_POINT ( 'NONE',  ( 26.29687500061451644, -3.027376345333614438, 5.243569643749998122 ) ) ;
#29556 = CARTESIAN_POINT ( 'NONE',  ( 17.87812500061451715, 6.421520780324663323E-16, -5.243569643749999010 ) ) ;
#29557 = CARTESIAN_POINT ( 'NONE',  ( 26.17500000122903359, -5.773502691896255534, -1.060575238724906372E-15 ) ) ;
#29558 = CARTESIAN_POINT ( 'NONE',  ( 25.04062500061451502, -3.027376345333610441, -5.243569643749999898 ) ) ;
#29559 = CARTESIAN_POINT ( 'NONE',  ( 21.72187500061451715, 3.027376345333611329, 5.243569643749999010 ) ) ;
#29560 = CARTESIAN_POINT ( 'NONE',  ( 17.20312500061451644, 0.000000000000000000, 5.243569643749999010 ) ) ;
#29561 = CARTESIAN_POINT ( 'NONE',  ( 4.243569643749999898, 17.34687500061451715, 32.45002607614398471 ) ) ;
#29562 = CARTESIAN_POINT ( 'NONE',  ( 23.12812500061451360, -4.541064518000419881, 2.621784821874995952 ) ) ;
#29563 = LINE ( 'NONE', #12207, #52669 ) ;
#29564 = VERTEX_POINT ( 'NONE', #22526 ) ;
#29565 = CARTESIAN_POINT ( 'NONE',  ( 25.34999999999999787, 4.330127018922192761, -2.499999999999997780 ) ) ;
#29566 = CARTESIAN_POINT ( 'NONE',  ( 3.999999999999999112, 13.92500000000000071, -30.00000000000000000 ) ) ;
#29567 = CARTESIAN_POINT ( 'NONE',  ( -1.878215178124999163, 19.20312499938548356, 26.74683588394047007 ) ) ;
#29568 = ADVANCED_FACE ( 'NONE', ( #50260 ), #6268, .T. ) ;
#29569 = CARTESIAN_POINT ( 'NONE',  ( 3.459375000614519635, -4.541064518000417216, -2.621784821875001281 ) ) ;
#29570 = CARTESIAN_POINT ( 'NONE',  ( 9.703125000614514661, -4.541064518000417216, -2.621784821875001281 ) ) ;
#29571 = CARTESIAN_POINT ( 'NONE',  ( 23.25000000122903288, 5.773502691896255534, 3.535250795749688894E-16 ) ) ;
#29572 = CARTESIAN_POINT ( 'NONE',  ( 26.65312500061451573, 0.000000000000000000, 5.243569643749999010 ) ) ;
#29573 = CARTESIAN_POINT ( 'NONE',  ( 24.89999999999999858, 4.330127018922192761, -2.499999999999997780 ) ) ;
#29574 = CARTESIAN_POINT ( 'NONE',  ( -3.999999999999997335, 16.10000000122903430, -27.69059892324149175 ) ) ;
#29575 = CARTESIAN_POINT ( 'NONE',  ( 29.42812500061451431, -4.541064518000419881, 2.621784821874995952 ) ) ;
#29576 = CARTESIAN_POINT ( 'NONE',  ( 9.853125000614516793, 4.541064518000418104, -2.621784821874998173 ) ) ;
#29577 = ORIENTED_EDGE ( 'NONE', *, *, #15596, .T. ) ;
#29578 = EDGE_CURVE ( 'NONE', #8958, #17518, #62241, .T. ) ;
#29579 = CARTESIAN_POINT ( 'NONE',  ( 25.26562500061451289, 3.027376345333611329, 5.243569643749999010 ) ) ;
#29580 = CARTESIAN_POINT ( 'NONE',  ( 7.603125000614517681, 4.541064518000418104, -2.621784821874998173 ) ) ;
#29581 = CARTESIAN_POINT ( 'NONE',  ( 5.803125000614517859, 4.541064518000418104, -2.621784821874998173 ) ) ;
#29582 = CARTESIAN_POINT ( 'NONE',  ( 16.09687500061452070, -2.746126346562642428, -4.756430356249999214 ) ) ;
#29583 = CARTESIAN_POINT ( 'NONE',  ( 4.635052905075760954, -1.875242991712875451, 4.896808582233176388 ) ) ;
#29584 = CARTESIAN_POINT ( 'NONE',  ( 13.31250000000000178, 2.886751345948126879, 4.999999999999999112 ) ) ;
#29585 = CARTESIAN_POINT ( 'NONE',  ( 14.67187500061451821, -6.054752690667223547, -1.112240025338166033E-15 ) ) ;
#29586 = CARTESIAN_POINT ( 'NONE',  ( 10.23750000122903359, 4.330127018922191873, 2.499999999999999556 ) ) ;
#29587 = CARTESIAN_POINT ( 'NONE',  ( 17.55937500061451573, 4.541064518000418104, -2.621784821874998173 ) ) ;
#29588 = CARTESIAN_POINT ( 'NONE',  ( 18.22499999999999787, 4.330127018922191873, 2.499999999999999556 ) ) ;
#29589 = CARTESIAN_POINT ( 'NONE',  ( 8.146875000614516082, 6.054752690667223547, 3.707466751127219781E-16 ) ) ;
#29590 = CARTESIAN_POINT ( 'NONE',  ( -4.243569643749999898, 10.76562500061451644, -32.45002607614398471 ) ) ;
#29591 = LINE ( 'NONE', #34764, #4098 ) ;
#29592 = CARTESIAN_POINT ( 'NONE',  ( 23.67187500061451289, 5.824947211148865298E-16, -4.756430356249998326 ) ) ;
#29593 = ORIENTED_EDGE ( 'NONE', *, *, #21830, .F. ) ;
#29594 = CARTESIAN_POINT ( 'NONE',  ( 24.55312500061451786, -4.541064518000417216, -2.621784821875001281 ) ) ;
#29595 = SURFACE_SIDE_STYLE ('',( #444 ) ) ;
#29596 = CARTESIAN_POINT ( 'NONE',  ( 29.33437500061451431, 4.541064518000418104, 2.621784821874999949 ) ) ;
#29597 =( BOUNDED_CURVE ( )  B_SPLINE_CURVE ( 2, ( #2923, #60153, #43188, #25453, #71250, #65708, #37630, #24716, #30267 ),
 .UNSPECIFIED., .F., .F. ) 
 B_SPLINE_CURVE_WITH_KNOTS ( ( 3, 2, 2, 2, 3 ),
 ( 0.3369565217391304324, 0.3405797101449275499, 0.3478260869565217295, 0.3550724637681159646, 0.3586956521739130821 ),
 .UNSPECIFIED. ) 
 CURVE ( )  GEOMETRIC_REPRESENTATION_ITEM ( )  RATIONAL_B_SPLINE_CURVE ( ( 0.9330127018922194093, 0.9330127018922194093, 1.000000000000000000, 0.8660254037844387076, 1.000000000000000000, 0.8660254037844387076, 1.000000000000000000, 0.9330127018922188542, 0.9330127018922194093 ) ) 
 REPRESENTATION_ITEM ( '' )  );
#29598 = CARTESIAN_POINT ( 'NONE',  ( 24.75000000000000000, -4.330127018922190985, -2.500000000000001332 ) ) ;
#29599 = CARTESIAN_POINT ( 'NONE',  ( 7.190625000614518036, 6.054752690667223547, 3.707466751127219781E-16 ) ) ;
#29600 = CARTESIAN_POINT ( 'NONE',  ( 25.62187500061451573, 4.119189519843966529, 2.378215178124999607 ) ) ;
#29601 = CARTESIAN_POINT ( 'NONE',  ( 18.83437500061451431, 6.421520780324663323E-16, -5.243569643749999010 ) ) ;
#29602 = CARTESIAN_POINT ( 'NONE',  ( 10.77187500061451608, 4.119189519843966529, 2.378215178124999607 ) ) ;
#29603 = CARTESIAN_POINT ( 'NONE',  ( 28.57500000122903572, 2.886751345948129099, -4.999999999999998224 ) ) ;
#29604 = CARTESIAN_POINT ( 'NONE',  ( 7.884375000614517681, -4.541064518000419881, 2.621784821874995952 ) ) ;
#29605 = ORIENTED_EDGE ( 'NONE', *, *, #3025, .T. ) ;
#29606 = CARTESIAN_POINT ( 'NONE',  ( 18.42187500061451644, 3.027376345333613106, -5.243569643749998122 ) ) ;
#29607 = CARTESIAN_POINT ( 'NONE',  ( -2.000000000000001776, 15.89374999877096784, 33.46410161513775705 ) ) ;
#29608 = CARTESIAN_POINT ( 'NONE',  ( 26.96249999999999858, -5.773502691896255534, -1.060575238724906372E-15 ) ) ;
#29609 = CARTESIAN_POINT ( 'NONE',  ( 29.03437500061451715, -4.541064518000419881, 2.621784821874995952 ) ) ;
#29610 = CARTESIAN_POINT ( 'NONE',  ( -5.810221930991193690E-16, 10.43750000000000000, -34.00000000000000000 ) ) ;
#29611 = CARTESIAN_POINT ( 'NONE',  ( 15.86250000000000071, 2.886751345948073588, -5.000000000000094147 ) ) ;
#29612 = ORIENTED_EDGE ( 'NONE', *, *, #24336, .T. ) ;
#29613 = CARTESIAN_POINT ( 'NONE',  ( 9.412499999999999645, -5.773502691896255534, -1.060575238724906372E-15 ) ) ;
#29614 = CARTESIAN_POINT ( 'NONE',  ( 12.64687500061451786, 0.000000000000000000, 4.756430356249998326 ) ) ;
#29615 = CARTESIAN_POINT ( 'NONE',  ( 24.62812500061451715, 6.421520780324663323E-16, -5.243569643749999010 ) ) ;
#29616 = CARTESIAN_POINT ( 'NONE',  ( 13.95000000000000107, -4.330127018922190985, -2.500000000000001332 ) ) ;
#29617 = CARTESIAN_POINT ( 'NONE',  ( 8.025000001229035007, 2.886751345948126879, 4.999999999999999112 ) ) ;
#29618 = CARTESIAN_POINT ( 'NONE',  ( 7.115625000614516082, 3.027376345333613106, -5.243569643749998122 ) ) ;
#29619 = CARTESIAN_POINT ( 'NONE',  ( 21.44999999999999929, 0.000000000000000000, 4.999999999999998224 ) ) ;
#29620 = EDGE_CURVE ( 'NONE', #33795, #52020, #11338, .T. ) ;
#29621 = CARTESIAN_POINT ( 'NONE',  ( 19.79062500061451502, 6.054752690667223547, 3.707466751127219781E-16 ) ) ;
#29622 = CARTESIAN_POINT ( 'NONE',  ( 26.36250000122903003, 4.330127018922192761, -2.499999999999997780 ) ) ;
#29623 = CARTESIAN_POINT ( 'NONE',  ( -3.756430356249999214, 17.77812499938548285, 27.83122392262697176 ) ) ;
#29624 = CARTESIAN_POINT ( 'NONE',  ( 4.837500000000001243, -2.886751345948129988, 4.999999999999997335 ) ) ;
#29625 = ORIENTED_EDGE ( 'NONE', *, *, #5562, .T. ) ;
#29626 = CARTESIAN_POINT ( 'NONE',  ( 21.36562500061451431, -6.054752690667223547, -1.112240025338166033E-15 ) ) ;
#29627 = CARTESIAN_POINT ( 'NONE',  ( 3.275492200589926739, -3.777717676570560901, -3.275492200590059078 ) ) ;
#29628 = CARTESIAN_POINT ( 'NONE',  ( 28.24687500061451573, -3.027376345333610441, -5.243569643749999898 ) ) ;
#29629 = CARTESIAN_POINT ( 'NONE',  ( 18.83437500061451431, 6.421520780324663323E-16, -5.243569643749999010 ) ) ;
#29630 = CARTESIAN_POINT ( 'NONE',  ( 14.84062500061451750, 6.054752690667223547, 3.707466751127219781E-16 ) ) ;
#29631 = CARTESIAN_POINT ( 'NONE',  ( 2.121784821874999061, 10.20312500061459460, -33.67503911421598417 ) ) ;
#29632 = CARTESIAN_POINT ( 'NONE',  ( 26.02500000122903145, 2.886751345948126879, 4.999999999999999112 ) ) ;
#29633 = CARTESIAN_POINT ( 'NONE',  ( 23.03437500061451715, 4.119189519843966529, 2.378215178124999607 ) ) ;
#29634 = CARTESIAN_POINT ( 'NONE',  ( 17.01562500061451644, 3.027376345333612662, -5.243569643749998122 ) ) ;
#29635 = CARTESIAN_POINT ( 'NONE',  ( 1.071796769724488119, 18.33259618943233704, -26.00000000000000000 ) ) ;
#29636 = CARTESIAN_POINT ( 'NONE',  ( 4.350000001229033408, 5.773502691896255534, 3.535250795749688894E-16 ) ) ;
#29637 = CARTESIAN_POINT ( 'NONE',  ( 13.32187500061451502, -6.054752690667223547, -1.112240025338166033E-15 ) ) ;
#29638 = CARTESIAN_POINT ( 'NONE',  ( 12.72187500061451537, 3.027376345333611329, 5.243569643749999010 ) ) ;
#29639 = CARTESIAN_POINT ( 'NONE',  ( 19.92187500061451644, 3.027376345333611329, 5.243569643749999010 ) ) ;
#29640 = ORIENTED_EDGE ( 'NONE', *, *, #49317, .F. ) ;
#29641 = CARTESIAN_POINT ( 'NONE',  ( 9.787499999999999645, -2.886751345948130876, 4.999999999999996447 ) ) ;
#29642 = CARTESIAN_POINT ( 'NONE',  ( 23.72812500061451502, 6.421520780324663323E-16, -5.243569643749999010 ) ) ;
#29643 = CARTESIAN_POINT ( 'NONE',  ( 19.69687500061451857, -3.027376345333610441, -5.243569643749999898 ) ) ;
#29644 = CARTESIAN_POINT ( 'NONE',  ( 25.15312500061451217, 4.541064518000418104, -2.621784821874998173 ) ) ;
#29645 = CARTESIAN_POINT ( 'NONE',  ( 3.999999999999999112, 18.98750000122903359, -30.00000000000000000 ) ) ;
#29646 = CARTESIAN_POINT ( 'NONE',  ( 3.999999999999999112, 15.27500000000000036, 30.00000000000000000 ) ) ;
#29647 = CARTESIAN_POINT ( 'NONE',  ( 3.534375000614518036, 6.421520780324663323E-16, -5.243569643749999010 ) ) ;
#29648 = CARTESIAN_POINT ( 'NONE',  ( 8.925000001229033586, 2.886751345948126879, 4.999999999999999112 ) ) ;
#29649 = CARTESIAN_POINT ( 'NONE',  ( 5.212500001229032343, 4.330127018922192761, -2.499999999999997780 ) ) ;
#29650 = CARTESIAN_POINT ( 'NONE',  ( 28.57499999999999929, 4.330127018922191873, 2.499999999999999556 ) ) ;
#29651 = CARTESIAN_POINT ( 'NONE',  ( 28.12500000122902932, 2.886751345948129099, -4.999999999999998224 ) ) ;
#29652 = CARTESIAN_POINT ( 'NONE',  ( 2.000000000000000444, 19.71874999877096712, 26.53589838486224650 ) ) ;
#29653 = ADVANCED_FACE ( 'NONE', ( #36101 ), #12485, .F. ) ;
#29654 = CARTESIAN_POINT ( 'NONE',  ( 10.17187500061451999, -6.054752690667223547, -1.112240025338166033E-15 ) ) ;
#29655 = CARTESIAN_POINT ( 'NONE',  ( 10.21875000122902932, 2.886751345948238789, 4.999999999999807265 ) ) ;
#29656 = CARTESIAN_POINT ( 'NONE',  ( 16.90312500061451573, -4.541064518000417216, -2.621784821875001281 ) ) ;
#29657 = CARTESIAN_POINT ( 'NONE',  ( 10.92187500061451644, 3.027376345333611329, 5.243569643749999010 ) ) ;
#29658 = CARTESIAN_POINT ( 'NONE',  ( 28.46250000122903145, -4.330127018922190985, -2.500000000000001332 ) ) ;
#29659 = CARTESIAN_POINT ( 'NONE',  ( 18.72187500061451360, -6.054752690667223547, -1.112240025338166033E-15 ) ) ;
#29660 = CARTESIAN_POINT ( 'NONE',  ( 7.921875000614517326, -6.054752690667223547, -1.112240025338166033E-15 ) ) ;
#29661 = CARTESIAN_POINT ( 'NONE',  ( 2.915625000614516793, -6.054752690667223547, -1.112240025338166033E-15 ) ) ;
#29662 = CARTESIAN_POINT ( 'NONE',  ( 11.70000000122903216, -2.886751345948130876, 4.999999999999996447 ) ) ;
#29663 = CARTESIAN_POINT ( 'NONE',  ( 7.978125000614517681, 6.421520780324663323E-16, -5.243569643749999010 ) ) ;
#29664 =( BOUNDED_CURVE ( )  B_SPLINE_CURVE ( 2, ( #23559, #25010, #19456, #42016, #47552, #64537, #23919 ),
 .UNSPECIFIED., .F., .F. ) 
 B_SPLINE_CURVE_WITH_KNOTS ( ( 3, 2, 2, 3 ),
 ( 0.3333333333333333703, 0.3361111111111111382, 0.3388888888888889062, 0.3416666666666666186 ),
 .UNSPECIFIED. ) 
 CURVE ( )  GEOMETRIC_REPRESENTATION_ITEM ( )  RATIONAL_B_SPLINE_CURVE ( ( 0.9999999999999973355, 0.8660254037844413721, 1.000000000000000000, 0.8660254037844387076, 1.000000000000000000, 0.8660254037844413721, 0.9999999999999973355 ) ) 
 REPRESENTATION_ITEM ( '' )  );
#29665 = CARTESIAN_POINT ( 'NONE',  ( 17.24062500061451786, -3.027376345333614438, 5.243569643749998122 ) ) ;
#29666 = ORIENTED_EDGE ( 'NONE', *, *, #1611, .F. ) ;
#29667 = CARTESIAN_POINT ( 'NONE',  ( 5.287500001229035185, 4.330127018922191873, 2.499999999999999556 ) ) ;
#29668 = CARTESIAN_POINT ( 'NONE',  ( 13.90312500061451750, 4.541064518000418104, -2.621784821874998173 ) ) ;
#29669 = CARTESIAN_POINT ( 'NONE',  ( 13.97812500061451679, 4.541064518000418104, 2.621784821874999949 ) ) ;
#29670 = CARTESIAN_POINT ( 'NONE',  ( 23.85937500061451644, 4.119189519843966529, -2.378215178124998275 ) ) ;
#29671 = CARTESIAN_POINT ( 'NONE',  ( 13.72500000000000142, 4.330127018922191873, 2.499999999999999556 ) ) ;
#29672 = CARTESIAN_POINT ( 'NONE',  ( 5.512500001229033941, -4.330127018922190985, -2.500000000000001332 ) ) ;
#29673 = CARTESIAN_POINT ( 'NONE',  ( 29.25000000000000000, -4.330127018922190985, -2.500000000000001332 ) ) ;
#29674 = CARTESIAN_POINT ( 'NONE',  ( 16.13437500061451502, 6.421520780324663323E-16, -5.243569643749999010 ) ) ;
#29675 = CARTESIAN_POINT ( 'NONE',  ( 17.66250000122903430, -4.330127018922190985, -2.500000000000001332 ) ) ;
#29676 = CARTESIAN_POINT ( 'NONE',  ( 24.29999999999999716, -4.330127018922190985, -2.500000000000001332 ) ) ;
#29677 = CARTESIAN_POINT ( 'NONE',  ( -3.000416591977282496E-16, 19.24062500061451431, -34.90005215228797653 ) ) ;
#29678 = CARTESIAN_POINT ( 'NONE',  ( -4.000000000000000000, 14.46874999877096712, 30.00000000000000000 ) ) ;
#29679 = CARTESIAN_POINT ( 'NONE',  ( 23.55000000122903359, -2.886751345948159742, -4.999999999999942268 ) ) ;
#29680 = CARTESIAN_POINT ( 'NONE',  ( 3.046343057529203424, 3.964819538874875704, 3.046343057529141696 ) ) ;
#29681 = CARTESIAN_POINT ( 'NONE',  ( 3.242103837493086330E-14, 13.13749999999999929, 26.00000000000000711 ) ) ;
#29682 = CARTESIAN_POINT ( 'NONE',  ( 19.54687500061451644, -3.027376345333614438, 5.243569643749998122 ) ) ;
#29683 = CARTESIAN_POINT ( 'NONE',  ( 15.26249999999999929, -5.773502691896255534, -1.060575238724906372E-15 ) ) ;
#29684 = CARTESIAN_POINT ( 'NONE',  ( 14.42812500061451786, 4.541064518000418104, 2.621784821874999949 ) ) ;
#29685 = CARTESIAN_POINT ( 'NONE',  ( 8.793750001229033941, 5.773502691896255534, 3.535250795749688894E-16 ) ) ;
#29686 = CARTESIAN_POINT ( 'NONE',  ( 15.75000000122903643, -2.886751345948197045, 4.999999999999880096 ) ) ;
#29687 = CARTESIAN_POINT ( 'NONE',  ( 25.99687500061451928, -3.027376345333610441, -5.243569643749999898 ) ) ;
#29688 = CARTESIAN_POINT ( 'NONE',  ( 18.53437500061451360, -2.746126346562646425, 4.756430356249996549 ) ) ;
#29689 = CARTESIAN_POINT ( 'NONE',  ( 9.740625000614516082, -3.027376345333610441, -5.243569643749999898 ) ) ;
#29690 = CARTESIAN_POINT ( 'NONE',  ( 15.75937500061451857, 4.541064518000418104, -2.621784821874998173 ) ) ;
#29691 = VERTEX_POINT ( 'NONE', #6943 ) ;
#29692 = CARTESIAN_POINT ( 'NONE',  ( 26.42812500061451431, 6.421520780324663323E-16, -5.243569643749999010 ) ) ;
#29693 = CARTESIAN_POINT ( 'NONE',  ( 19.60312500061451502, -4.541064518000417216, -2.621784821875001281 ) ) ;
#29694 = CARTESIAN_POINT ( 'NONE',  ( 18.89999999999999858, -4.330127018922190985, -2.500000000000001332 ) ) ;
#29695 = CARTESIAN_POINT ( 'NONE',  ( -3.999999999999999112, 14.26250000122903572, -30.00000000000000000 ) ) ;
#29696 = CARTESIAN_POINT ( 'NONE',  ( 9.412499999999999645, -5.773502691896255534, -1.060575238724906372E-15 ) ) ;
#29697 = CARTESIAN_POINT ( 'NONE',  ( 18.75000000122903288, 5.773502691896255534, 3.535250795749688894E-16 ) ) ;
#29698 = CARTESIAN_POINT ( 'NONE',  ( 3.999999999999999112, 10.32500000000000107, 30.00000000000000000 ) ) ;
#29699 = CARTESIAN_POINT ( 'NONE',  ( 9.721875000614517148, 5.824947211148865298E-16, -4.756430356249998326 ) ) ;
#29700 = ORIENTED_EDGE ( 'NONE', *, *, #23453, .F. ) ;
#29701 = CARTESIAN_POINT ( 'NONE',  ( 18.30000000000000071, 0.000000000000000000, 4.999999999999998224 ) ) ;
#29702 = CARTESIAN_POINT ( 'NONE',  ( 21.30000000000000071, 4.330127018922192761, -2.499999999999997780 ) ) ;
#29703 = CARTESIAN_POINT ( 'NONE',  ( 18.98437500061451644, 4.541064518000418104, 2.621784821874999949 ) ) ;
#29704 = CARTESIAN_POINT ( 'NONE',  ( 24.51562500061451289, -6.054752690667223547, -1.112240025338166033E-15 ) ) ;
#29705 = ORIENTED_EDGE ( 'NONE', *, *, #32955, .T. ) ;
#29706 = CARTESIAN_POINT ( 'NONE',  ( 1.592000809091587073E-14, 16.85000000122903785, 26.00000000000000000 ) ) ;
#29707 = CARTESIAN_POINT ( 'NONE',  ( 5.015625000614518214, 3.027376345333611329, 5.243569643749999010 ) ) ;
#29708 = CARTESIAN_POINT ( 'NONE',  ( -1.999999999999999112, 18.89374999877096784, 26.53589838486224650 ) ) ;
#29709 = CARTESIAN_POINT ( 'NONE',  ( 14.55000000000000071, 4.330127018922192761, -2.499999999999997780 ) ) ;
#29710 = CARTESIAN_POINT ( 'NONE',  ( 2.121784821875001281, 18.60312500061451857, 33.67503911421598417 ) ) ;
#29711 = CARTESIAN_POINT ( 'NONE',  ( 28.90312500061451217, 0.000000000000000000, 5.243569643749999010 ) ) ;
#29712 = CARTESIAN_POINT ( 'NONE',  ( 10.46249999999999858, 2.886751345948129099, -4.999999999999998224 ) ) ;
#29713 = CARTESIAN_POINT ( 'NONE',  ( 3.756430356250000102, 16.24062499938548143, 30.00000000000000000 ) ) ;
#29714 = CARTESIAN_POINT ( 'NONE',  ( 25.17187500061451644, 3.027376345333613106, -5.243569643749998122 ) ) ;
#29715 = VERTEX_POINT ( 'NONE', #35012 ) ;
#29716 = CARTESIAN_POINT ( 'NONE',  ( 21.21562500061451573, 3.027376345333611329, 5.243569643749999010 ) ) ;
#29717 = CARTESIAN_POINT ( 'NONE',  ( 23.22187500061451715, -6.054752690667223547, -1.112240025338166033E-15 ) ) ;
#29718 = CARTESIAN_POINT ( 'NONE',  ( 2.121784821874999061, 16.95312500061459460, -33.67503911421598417 ) ) ;
#29719 = CARTESIAN_POINT ( 'NONE',  ( 7.340625000614518392, -3.027376345333614438, 5.243569643749998122 ) ) ;
#29720 = CARTESIAN_POINT ( 'NONE',  ( 29.14687500061451431, -2.746126346562641984, -4.756430356249999214 ) ) ;
#29721 = CARTESIAN_POINT ( 'NONE',  ( 23.72812500061451502, 6.421520780324663323E-16, -5.243569643749999010 ) ) ;
#29722 = CARTESIAN_POINT ( 'NONE',  ( 27.12187500061451573, -4.119189519843968306, 2.378215178124996054 ) ) ;
#29723 = CARTESIAN_POINT ( 'NONE',  ( 13.54687500061451999, 5.492252693125287522, 3.363034840372157021E-16 ) ) ;
#29724 = CARTESIAN_POINT ( 'NONE',  ( 17.78437500061451715, -4.541064518000419881, 2.621784821874995952 ) ) ;
#29725 = EDGE_CURVE ( 'NONE', #4282, #59530, #51880, .T. ) ;
#29726 = CARTESIAN_POINT ( 'NONE',  ( 19.13437500061451857, -4.541064518000419881, 2.621784821874995952 ) ) ;
#29727 = CARTESIAN_POINT ( 'NONE',  ( 26.25937500061451857, 0.000000000000000000, 5.243569643749999010 ) ) ;
#29728 = CARTESIAN_POINT ( 'NONE',  ( 2.121784821875001281, 17.30937500061451573, 33.67503911421598417 ) ) ;
#29729 = CARTESIAN_POINT ( 'NONE',  ( 8.690625000614515372, -3.027376345333614438, 5.243569643749998122 ) ) ;
#29730 = DIRECTION ( 'NONE',  ( -1.000000000000000000, -0.000000000000000000, -0.000000000000000000 ) ) ;
#29731 = CARTESIAN_POINT ( 'NONE',  ( 5.634375000614519458, -4.541064518000419881, 2.621784821874995952 ) ) ;
#29732 = CARTESIAN_POINT ( 'NONE',  ( 29.74687500061451573, 0.000000000000000000, 4.756430356249998326 ) ) ;
#29733 = CARTESIAN_POINT ( 'NONE',  ( 4.640625000614518214, -3.027376345333614438, 5.243569643749998122 ) ) ;
#29734 = CARTESIAN_POINT ( 'NONE',  ( 10.80937500061451928, 4.541064518000418104, -2.621784821874998173 ) ) ;
#29735 = DIRECTION ( 'NONE',  ( 0.000000000000000000, 0.000000000000000000, 1.000000000000000000 ) ) ;
#29736 = CARTESIAN_POINT ( 'NONE',  ( 16.50000000122903288, 5.773502691896255534, 3.535250795749688894E-16 ) ) ;
#29737 = CARTESIAN_POINT ( 'NONE',  ( 4.659375000614518925, 0.000000000000000000, 5.243569643749999010 ) ) ;
#29738 = CARTESIAN_POINT ( 'NONE',  ( 6.290625000614517681, 6.054752690667223547, 3.707466751127219781E-16 ) ) ;
#29739 = CARTESIAN_POINT ( 'NONE',  ( 0.000000000000000000, 27.50000000000000000, 30.00000000000000000 ) ) ;
#29740 = CARTESIAN_POINT ( 'NONE',  ( 24.46875000122903288, 2.886751345948129099, -4.999999999999998224 ) ) ;
#29741 = CARTESIAN_POINT ( 'NONE',  ( 17.22187500061451715, 3.027376345333611329, 5.243569643749999010 ) ) ;
#29742 = FACE_OUTER_BOUND ( 'NONE', #53429, .T. ) ;
#29743 = ORIENTED_EDGE ( 'NONE', *, *, #18362, .F. ) ;
#29744 = CARTESIAN_POINT ( 'NONE',  ( 25.07812500061451644, 6.421520780324663323E-16, -5.243569643749999010 ) ) ;
#29745 = CARTESIAN_POINT ( 'NONE',  ( 8.653125000614515727, 0.000000000000000000, 5.243569643749999010 ) ) ;
#29746 = CARTESIAN_POINT ( 'NONE',  ( 26.55937500061451573, 4.541064518000418104, -2.621784821874998173 ) ) ;
#29747 = CARTESIAN_POINT ( 'NONE',  ( 9.065625000614517148, 3.027376345333611329, 5.243569643749999010 ) ) ;
#29748 = CARTESIAN_POINT ( 'NONE',  ( 29.02499999999999858, 4.330127018922191873, 2.499999999999999556 ) ) ;
#29749 = CARTESIAN_POINT ( 'NONE',  ( 11.21250000122903501, 0.000000000000000000, 4.999999999999998224 ) ) ;
#29750 = CARTESIAN_POINT ( 'NONE',  ( 25.41562500061451146, -6.054752690667223547, -1.112240025338166033E-15 ) ) ;
#29751 = VECTOR ( 'NONE', #70777, 1000.000000000000000 ) ;
#29752 = CARTESIAN_POINT ( 'NONE',  ( -2.121784821874996840, 12.67812500061451786, -26.32496088578401583 ) ) ;
#29753 = CARTESIAN_POINT ( 'NONE',  ( 11.66250000122903430, 0.000000000000000000, 4.999999999999998224 ) ) ;
#29754 = CARTESIAN_POINT ( 'NONE',  ( 22.86562500061451431, 3.027376345333613106, -5.243569643749998122 ) ) ;
#29755 = CARTESIAN_POINT ( 'NONE',  ( 10.65000000000000036, 0.000000000000000000, 4.999999999999998224 ) ) ;
#29756 = CARTESIAN_POINT ( 'NONE',  ( 19.26562500061451644, 3.027376345333613106, -5.243569643749998122 ) ) ;
#29757 = CARTESIAN_POINT ( 'NONE',  ( 5.071875000614518569, 3.027376345333611329, 5.243569643749999010 ) ) ;
#29758 = CARTESIAN_POINT ( 'NONE',  ( 20.36249999999999716, 2.886751345948129099, -4.999999999999998224 ) ) ;
#29759 = CARTESIAN_POINT ( 'NONE',  ( 13.35000000122903430, 5.773502691896255534, 3.535250795749688894E-16 ) ) ;
#29760 = CARTESIAN_POINT ( 'NONE',  ( 9.928125000614517859, 4.541064518000418104, 2.621784821874999949 ) ) ;
#29761 = CARTESIAN_POINT ( 'NONE',  ( 15.47812500061451679, -4.541064518000419881, 2.621784821874995952 ) ) ;
#29762 = CARTESIAN_POINT ( 'NONE',  ( 24.93750000122903288, 6.123233995736764310E-16, -4.999999999999998224 ) ) ;
#29763 = CARTESIAN_POINT ( 'NONE',  ( 22.58437500061451431, 4.541064518000418104, 2.621784821874999949 ) ) ;
#29764 = CARTESIAN_POINT ( 'NONE',  ( 22.18125000122903145, 6.123233995736764310E-16, -4.999999999999998224 ) ) ;
#29765 = ADVANCED_FACE ( 'NONE', ( #35734 ), #29474, .T. ) ;
#29766 = CARTESIAN_POINT ( 'NONE',  ( 6.600000001229032520, 5.773502691896255534, 3.535250795749688894E-16 ) ) ;
#29767 = EDGE_CURVE ( 'NONE', #24148, #68292, #14118, .T. ) ;
#29768 = CARTESIAN_POINT ( 'NONE',  ( 9.271875000614516082, -6.054752690667223547, -1.112240025338166033E-15 ) ) ;
#29769 = CARTESIAN_POINT ( 'NONE',  ( 26.78437500061451360, -4.541064518000419881, 2.621784821874995952 ) ) ;
#29770 = CARTESIAN_POINT ( 'NONE',  ( 23.73749999999999716, -2.886751345948130876, 4.999999999999996447 ) ) ;
#29771 = CARTESIAN_POINT ( 'NONE',  ( 20.31562500061451715, 3.027376345333611329, 5.243569643749999010 ) ) ;
#29772 = CARTESIAN_POINT ( 'NONE',  ( 25.58437500061451431, 6.421520780324663323E-16, -5.243569643749999010 ) ) ;
#29773 = CARTESIAN_POINT ( 'NONE',  ( 3.756430356250000546, 17.29062499938548214, 27.83122392262697886 ) ) ;
#29774 = CARTESIAN_POINT ( 'NONE',  ( 16.33125000122903359, 6.123233995736764310E-16, -4.999999999999998224 ) ) ;
#29775 = CARTESIAN_POINT ( 'NONE',  ( 7.809375000614519280, 0.000000000000000000, 5.243569643749999010 ) ) ;
#29776 = CARTESIAN_POINT ( 'NONE',  ( 20.09062500061451573, -3.027376345333610441, -5.243569643749999898 ) ) ;
#29777 = ORIENTED_EDGE ( 'NONE', *, *, #33488, .T. ) ;
#29778 = CARTESIAN_POINT ( 'NONE',  ( 0.000000000000000000, 20.00000000000000000, 30.00000000000000000 ) ) ;
#29779 = CARTESIAN_POINT ( 'NONE',  ( 27.44062500061451715, 6.054752690667223547, 3.707466751127219781E-16 ) ) ;
#29780 = CARTESIAN_POINT ( 'NONE',  ( 5.184375000614516615, -4.541064518000419881, 2.621784821874995952 ) ) ;
#29781 = CARTESIAN_POINT ( 'NONE',  ( 0.000000000000000000, 20.00000000000000000, -30.00000000000000000 ) ) ;
#29782 = CARTESIAN_POINT ( 'NONE',  ( 30.00000000000000000, 6.123233995736764310E-16, -4.999999999999998224 ) ) ;
#29783 = CARTESIAN_POINT ( 'NONE',  ( 17.62500000000000000, 6.123233995736764310E-16, -4.999999999999998224 ) ) ;
#29784 = CARTESIAN_POINT ( 'NONE',  ( 21.59062500061451928, 6.054752690667223547, 3.707466751127219781E-16 ) ) ;
#29785 = VERTEX_POINT ( 'NONE', #41293 ) ;
#29786 = CARTESIAN_POINT ( 'NONE',  ( 25.80000000000000071, 4.330127018922192761, -2.499999999999997780 ) ) ;
#29787 = CARTESIAN_POINT ( 'NONE',  ( 25.84687500061451360, -3.027376345333614438, 5.243569643749998122 ) ) ;
#29788 = EDGE_LOOP ( 'NONE', ( #14515, #30380, #18332, #4563 ) ) ;
#29789 = AXIS2_PLACEMENT_3D ( 'NONE', #41867, #17866, #46330 ) ;
#29790 = CARTESIAN_POINT ( 'NONE',  ( 12.44062500061451537, -3.027376345333610441, -5.243569643749999898 ) ) ;
#29791 = CARTESIAN_POINT ( 'NONE',  ( 6.515625000614516438, -6.054752690667223547, -1.112240025338166033E-15 ) ) ;
#29792 = CARTESIAN_POINT ( 'NONE',  ( 17.78437500061451360, -2.746126346562642428, -4.756430356249999214 ) ) ;
#29793 = CARTESIAN_POINT ( 'NONE',  ( 28.67812500061451431, 6.421520780324663323E-16, -5.243569643749999010 ) ) ;
#29794 = CARTESIAN_POINT ( 'NONE',  ( 15.07500000122903394, 2.886751345948129099, -4.999999999999998224 ) ) ;
#29795 = CARTESIAN_POINT ( 'NONE',  ( 22.98749999999999716, -2.886751345948125991, -5.000000000000000000 ) ) ;
#29796 = CARTESIAN_POINT ( 'NONE',  ( 29.32499999999999929, 6.123233995736764310E-16, -4.999999999999998224 ) ) ;
#29797 = CARTESIAN_POINT ( 'NONE',  ( 4.096875000614518925, 6.054752690667223547, 3.707466751127219781E-16 ) ) ;
#29798 = CARTESIAN_POINT ( 'NONE',  ( 9.121875000614517504, 3.027376345333611329, 5.243569643749999010 ) ) ;
#29799 = CARTESIAN_POINT ( 'NONE',  ( 19.13437500061451857, -4.541064518000419881, 2.621784821874995952 ) ) ;
#29800 = CARTESIAN_POINT ( 'NONE',  ( 45.00000000000000000, 0.000000000000000000, 0.000000000000000000 ) ) ;
#29801 = VERTEX_POINT ( 'NONE', #1412 ) ;
#29802 = CARTESIAN_POINT ( 'NONE',  ( 28.45312500061451289, 0.000000000000000000, 5.243569643749999010 ) ) ;
#29803 = CARTESIAN_POINT ( 'NONE',  ( 4.312500000000000000, 2.886751345948126879, 4.999999999999999112 ) ) ;
#29804 = EDGE_CURVE ( 'NONE', #72082, #964, #29664, .T. ) ;
#29805 = CARTESIAN_POINT ( 'NONE',  ( 4.621875000614516615, 3.027376345333611329, 5.243569643749999010 ) ) ;
#29806 = CARTESIAN_POINT ( 'NONE',  ( 19.68750000000000355, -2.886751345948129988, 4.999999999999997335 ) ) ;
#29807 = CARTESIAN_POINT ( 'NONE',  ( 13.04062500061451502, 6.054752690667223547, 3.707466751127219781E-16 ) ) ;
#29808 = CARTESIAN_POINT ( 'NONE',  ( 4.000000000000000000, 18.83749999999999858, 27.69059892324149530 ) ) ;
#29809 = CARTESIAN_POINT ( 'NONE',  ( 0.000000000000000000, 20.00000000000000000, 30.00000000000000000 ) ) ;
#29810 = CARTESIAN_POINT ( 'NONE',  ( 5.000000000000000000, 6.176262757673013563E-16, -5.043301270189223473 ) ) ;
#29811 = CARTESIAN_POINT ( 'NONE',  ( 21.04687500061451644, -2.746126346562642428, -4.756430356249999214 ) ) ;
#29812 = CARTESIAN_POINT ( 'NONE',  ( 7.153125000614518392, 4.541064518000418104, -2.621784821874998173 ) ) ;
#29813 = CARTESIAN_POINT ( 'NONE',  ( 24.45937500061451786, 0.000000000000000000, 5.243569643749999010 ) ) ;
#29814 = CARTESIAN_POINT ( 'NONE',  ( -4.243569643749999898, 18.47187500061451715, 27.54997392385601529 ) ) ;
#29815 = CARTESIAN_POINT ( 'NONE',  ( 26.44687500061451502, -3.027376345333610441, -5.243569643749999898 ) ) ;
#29816 = CARTESIAN_POINT ( 'NONE',  ( 8.212500000000000355, 2.886751345948129099, -4.999999999999998224 ) ) ;
#29817 = CARTESIAN_POINT ( 'NONE',  ( -3.999999999999999556, 14.22500000122903430, 27.69059892324149530 ) ) ;
#29818 = CARTESIAN_POINT ( 'NONE',  ( 14.39062500061451821, 6.054752690667223547, 3.707466751127219781E-16 ) ) ;
#29819 = CARTESIAN_POINT ( 'NONE',  ( 7.312500001229033764, -4.330127018922190985, -2.500000000000001332 ) ) ;
#29820 = CARTESIAN_POINT ( 'NONE',  ( 17.48437500061451999, 6.421520780324663323E-16, -5.243569643749999010 ) ) ;
#29821 = CARTESIAN_POINT ( 'NONE',  ( 11.93437500061451573, -4.541064518000419881, 2.621784821874995952 ) ) ;
#29822 = DIRECTION ( 'NONE',  ( -0.000000000000000000, -1.000000000000000000, -0.000000000000000000 ) ) ;
#29823 = ORIENTED_EDGE ( 'NONE', *, *, #47090, .F. ) ;
#29824 = CARTESIAN_POINT ( 'NONE',  ( 11.50312500061451892, -4.541064518000417216, -2.621784821875001281 ) ) ;
#29825 = CARTESIAN_POINT ( 'NONE',  ( 29.21250000122903145, 0.000000000000000000, 4.999999999999998224 ) ) ;
#29826 = CARTESIAN_POINT ( 'NONE',  ( 23.32500000122903572, 2.886751345948126879, 4.999999999999999112 ) ) ;
#29827 = CARTESIAN_POINT ( 'NONE',  ( 13.62187500061451750, 3.027376345333611329, 5.243569643749999010 ) ) ;
#29828 = CARTESIAN_POINT ( 'NONE',  ( 15.32812500061451644, 4.541064518000418104, 2.621784821874999949 ) ) ;
#29829 = CARTESIAN_POINT ( 'NONE',  ( 2.000000000000001332, 16.55000000000000071, -26.53589838486224650 ) ) ;
#29830 = CARTESIAN_POINT ( 'NONE',  ( 23.48437500061451644, 4.541064518000418104, 2.621784821874999949 ) ) ;
#29831 = LINE ( 'NONE', #69370, #51375 ) ;
#29832 = CARTESIAN_POINT ( 'NONE',  ( 12.30000000122903181, -2.886751345948125991, -5.000000000000000000 ) ) ;
#29833 = CARTESIAN_POINT ( 'NONE',  ( 4.295826441391526807, 3.688361401553225338, -3.611570655833856502 ) ) ;
#29834 = CARTESIAN_POINT ( 'NONE',  ( 22.63125000122903430, 6.123233995736764310E-16, -4.999999999999998224 ) ) ;
#29835 = CARTESIAN_POINT ( 'NONE',  ( 4.243569643749999898, 16.93437500061451573, -30.00000000000000000 ) ) ;
#29836 = CARTESIAN_POINT ( 'NONE',  ( 18.79687500061451644, -3.027376345333610441, -5.243569643749999898 ) ) ;
#29837 = CARTESIAN_POINT ( 'NONE',  ( 17.73750000122903359, 6.123233995736764310E-16, -4.999999999999998224 ) ) ;
#29838 = CARTESIAN_POINT ( 'NONE',  ( 13.13437500061451857, 4.541064518000418104, 2.621784821874999949 ) ) ;
#29839 = CARTESIAN_POINT ( 'NONE',  ( -4.243569643749997233, 10.44687500061451857, 32.45002607614398471 ) ) ;
#29840 = CARTESIAN_POINT ( 'NONE',  ( 19.98750000122903359, 6.123233995736764310E-16, -4.999999999999998224 ) ) ;
#29841 = CARTESIAN_POINT ( 'NONE',  ( 13.86562500061451431, 3.027376345333613106, -5.243569643749998122 ) ) ;
#29842 = VERTEX_POINT ( 'NONE', #51649 ) ;
#29843 = VERTEX_POINT ( 'NONE', #69006 ) ;
#29844 = CARTESIAN_POINT ( 'NONE',  ( 17.13749999999999929, -2.886751345948125991, -5.000000000000000000 ) ) ;
#29845 = CARTESIAN_POINT ( 'NONE',  ( 3.999999999999998668, 14.26250000000000107, 32.30940107675850470 ) ) ;
#29846 = CARTESIAN_POINT ( 'NONE',  ( 13.43437500061451750, 6.421520780324663323E-16, -5.243569643749999010 ) ) ;
#29847 = DIRECTION ( 'NONE',  ( -0.000000000000000000, -0.000000000000000000, -1.000000000000000000 ) ) ;
#29848 = CARTESIAN_POINT ( 'NONE',  ( 15.82500000122903216, -5.773502691896255534, -1.060575238724906372E-15 ) ) ;
#29849 = CARTESIAN_POINT ( 'NONE',  ( 27.68437500061451573, -4.541064518000419881, 2.621784821874995952 ) ) ;
#29850 = CARTESIAN_POINT ( 'NONE',  ( 21.06562500061451715, 3.027376345333613106, -5.243569643749998122 ) ) ;
#29851 = CARTESIAN_POINT ( 'NONE',  ( 22.45312500061451644, 4.541064518000418104, -2.621784821874998173 ) ) ;
#29852 = CARTESIAN_POINT ( 'NONE',  ( 29.32500000122903216, -5.773502691896255534, -1.060575238724906372E-15 ) ) ;
#29853 = CARTESIAN_POINT ( 'NONE',  ( 28.53749999999999787, 5.773502691896255534, 3.535250795749688894E-16 ) ) ;
#29854 = CARTESIAN_POINT ( 'NONE',  ( -2.000000000000000000, 10.13750000122903572, -33.46410161513775705 ) ) ;
#29855 = CARTESIAN_POINT ( 'NONE',  ( 9.159375000614515372, 0.000000000000000000, 4.756430356249998326 ) ) ;
#29856 = CARTESIAN_POINT ( 'NONE',  ( 0.000000000000000000, 20.00000000000000000, -30.00000000000000000 ) ) ;
#29857 = CARTESIAN_POINT ( 'NONE',  ( -1.999999999999997113, 9.837500001229035007, -26.53589838486224295 ) ) ;
#29858 = CARTESIAN_POINT ( 'NONE',  ( 2.121784821874999061, 15.20937500061451786, -33.67503911421598417 ) ) ;
#29859 = CARTESIAN_POINT ( 'NONE',  ( 7.312500001229033764, -4.330127018922190985, -2.500000000000001332 ) ) ;
#29860 = CARTESIAN_POINT ( 'NONE',  ( 5.512499999999999289, 2.886751345948129099, -4.999999999999998224 ) ) ;
#29861 = CARTESIAN_POINT ( 'NONE',  ( 28.78125000122903288, -4.330127018922194537, 2.499999999999995559 ) ) ;
#29862 = CARTESIAN_POINT ( 'NONE',  ( 9.796875000614519990, -3.027376345333610441, -5.243569643749999898 ) ) ;
#29863 = CARTESIAN_POINT ( 'NONE',  ( 28.30312500061451431, 4.541064518000418104, -2.621784821874998173 ) ) ;
#29864 = LINE ( 'NONE', #18400, #19655 ) ;
#29865 = CARTESIAN_POINT ( 'NONE',  ( 30.00000000000000000, 0.000000000000000000, 0.000000000000000000 ) ) ;
#29866 = CARTESIAN_POINT ( 'NONE',  ( 7.546875000614517326, -3.027376345333610441, -5.243569643749999898 ) ) ;
#29867 = CARTESIAN_POINT ( 'NONE',  ( 12.38437500061451857, -4.541064518000419881, 2.621784821874995952 ) ) ;
#29868 = CARTESIAN_POINT ( 'NONE',  ( 6.037500000000001421, 5.773502691896255534, 3.535250795749688894E-16 ) ) ;
#29869 = CARTESIAN_POINT ( 'NONE',  ( -4.243569643749999898, 13.91562500061459140, 27.54997392385601529 ) ) ;
#29870 = CARTESIAN_POINT ( 'NONE',  ( 3.974238962994274260, 25.00693170370651686, 29.47568919947315180 ) ) ;
#29871 =( BOUNDED_CURVE ( )  B_SPLINE_CURVE ( 2, ( #48721, #66068, #71244, #20623, #54621, #65701, #14360, #15088, #3292 ),
 .UNSPECIFIED., .F., .F. ) 
 B_SPLINE_CURVE_WITH_KNOTS ( ( 3, 2, 2, 2, 3 ),
 ( 0.9239130434782608647, 0.9275362318840579823, 0.9347826086956522174, 0.9420289855072463414, 0.9456521739130434590 ),
 .UNSPECIFIED. ) 
 CURVE ( )  GEOMETRIC_REPRESENTATION_ITEM ( )  RATIONAL_B_SPLINE_CURVE ( ( 0.9330127018922194093, 0.9330127018922194093, 1.000000000000000000, 0.8660254037844387076, 1.000000000000000000, 0.8660254037844387076, 1.000000000000000000, 0.9330127018922194093, 0.9330127018922194093 ) ) 
 REPRESENTATION_ITEM ( '' )  );
#29872 = CARTESIAN_POINT ( 'NONE',  ( 7.537500000000002309, -2.886751345948129988, 4.999999999999997335 ) ) ;
#29873 = CARTESIAN_POINT ( 'NONE',  ( 26.10000000122903430, -2.886751345948129988, 4.999999999999997335 ) ) ;
#29874 = CARTESIAN_POINT ( 'NONE',  ( 17.67187500061451644, -4.119189519843968306, 2.378215178124996054 ) ) ;
#29875 = CARTESIAN_POINT ( 'NONE',  ( 23.84062500061451928, 6.054752690667223547, 3.707466751127219781E-16 ) ) ;
#29876 = CARTESIAN_POINT ( 'NONE',  ( 13.26562500061451644, -6.054752690667223547, -1.112240025338166033E-15 ) ) ;
#29877 = CARTESIAN_POINT ( 'NONE',  ( 25.39687500061451431, -4.119189519843965641, -2.378215178125001383 ) ) ;
#29878 = CARTESIAN_POINT ( 'NONE',  ( 8.634375000614518569, 4.541064518000418104, 2.621784821874999949 ) ) ;
#29879 = CARTESIAN_POINT ( 'NONE',  ( 26.84999999999999787, 0.000000000000000000, 4.999999999999998224 ) ) ;
#29880 = CARTESIAN_POINT ( 'NONE',  ( 23.06250000122903288, -4.330127018922190985, -2.500000000000001332 ) ) ;
#29881 = CARTESIAN_POINT ( 'NONE',  ( 12.12187500061451573, 3.027376345333613106, -5.243569643749998122 ) ) ;
#29882 = CARTESIAN_POINT ( 'NONE',  ( 26.07187500061451857, 3.027376345333613106, -5.243569643749998122 ) ) ;
#29883 = CARTESIAN_POINT ( 'NONE',  ( 3.234375000614516438, 4.541064518000418104, 2.621784821874999949 ) ) ;
#29884 = CARTESIAN_POINT ( 'NONE',  ( 4.000000000000000000, 13.55000000122903359, -27.69059892324149885 ) ) ;
#29885 = CARTESIAN_POINT ( 'NONE',  ( 21.75937500061451502, 0.000000000000000000, 5.243569643749999010 ) ) ;
#29886 = CARTESIAN_POINT ( 'NONE',  ( 11.74687500061451573, 6.054752690667223547, 3.707466751127219781E-16 ) ) ;
#29887 = CARTESIAN_POINT ( 'NONE',  ( 1.878215178124997609, 17.62812499938548427, 33.25316411605952993 ) ) ;
#29888 = CARTESIAN_POINT ( 'NONE',  ( 25.12499999999999645, -4.330127018922194537, 2.499999999999995559 ) ) ;
#29889 = CARTESIAN_POINT ( 'NONE',  ( 1.999999999999997335, 12.87500000000000178, 33.46410161513775705 ) ) ;
#29890 = CARTESIAN_POINT ( 'NONE',  ( -3.000416591977282496E-16, 12.54687500061451999, -34.90005215228797653 ) ) ;
#29891 = CARTESIAN_POINT ( 'NONE',  ( 27.15937500061451360, 0.000000000000000000, 4.756430356249998326 ) ) ;
#29892 = CARTESIAN_POINT ( 'NONE',  ( 15.70312500061451644, 4.541064518000418104, -2.621784821874998173 ) ) ;
#29893 = CARTESIAN_POINT ( 'NONE',  ( 6.000000000000001776, 4.330127018922192761, -2.499999999999997780 ) ) ;
#29894 = DIRECTION ( 'NONE',  ( 0.000000000000000000, 0.000000000000000000, -1.000000000000000000 ) ) ;
#29895 = CARTESIAN_POINT ( 'NONE',  ( 18.93749999999999645, -2.886751345948181946, -4.999999999999904077 ) ) ;
#29896 = CARTESIAN_POINT ( 'NONE',  ( 14.77500000000000036, -4.330127018922194537, 2.499999999999995559 ) ) ;
#29897 = EDGE_CURVE ( 'NONE', #15065, #57451, #64284, .T. ) ;
#29898 = CARTESIAN_POINT ( 'NONE',  ( 4.243569643749999898, 11.02812500061451750, 30.00000000000000000 ) ) ;
#29899 = CARTESIAN_POINT ( 'NONE',  ( 14.13750000122903394, 6.123233995736764310E-16, -4.999999999999998224 ) ) ;
#29900 = CARTESIAN_POINT ( 'NONE',  ( 24.79687500061451999, 6.054752690667223547, 3.707466751127219781E-16 ) ) ;
#29901 = ORIENTED_EDGE ( 'NONE', *, *, #37581, .T. ) ;
#29902 = CARTESIAN_POINT ( 'NONE',  ( 20.54062500061451502, -3.027376345333610441, -5.243569643749999898 ) ) ;
#29903 = CARTESIAN_POINT ( 'NONE',  ( 19.58437500061451786, -4.541064518000419881, 2.621784821874995952 ) ) ;
#29904 = CARTESIAN_POINT ( 'NONE',  ( 5.175000000000002487, 4.330127018922191873, 2.499999999999999556 ) ) ;
#29905 = CARTESIAN_POINT ( 'NONE',  ( 7.340625000614518392, -3.027376345333614438, 5.243569643749998122 ) ) ;
#29906 = CARTESIAN_POINT ( 'NONE',  ( 22.49062500061451431, 6.054752690667223547, 3.707466751127219781E-16 ) ) ;
#29907 = CARTESIAN_POINT ( 'NONE',  ( 17.59687500061451715, 6.054752690667223547, 3.707466751127219781E-16 ) ) ;
#29908 = CARTESIAN_POINT ( 'NONE',  ( 4.243569643749999010, 14.66562500061451857, 27.54997392385601174 ) ) ;
#29909 = CARTESIAN_POINT ( 'NONE',  ( 19.46250000122903145, -4.330127018922190985, -2.500000000000001332 ) ) ;
#29910 = CARTESIAN_POINT ( 'NONE',  ( 13.35937500061451821, -4.119189519843965641, -2.378215178125001383 ) ) ;
#29911 = CARTESIAN_POINT ( 'NONE',  ( 8.428125000614517859, 6.421520780324663323E-16, -5.243569643749999010 ) ) ;
#29912 = CARTESIAN_POINT ( 'NONE',  ( 16.72500000000000142, 6.123233995736764310E-16, -4.999999999999998224 ) ) ;
#29913 = CARTESIAN_POINT ( 'NONE',  ( 29.31562500061451715, 3.027376345333611329, 5.243569643749999010 ) ) ;
#29914 = CARTESIAN_POINT ( 'NONE',  ( 25.54687500061451644, -3.027376345333610441, -5.243569643749999898 ) ) ;
#29915 = CARTESIAN_POINT ( 'NONE',  ( 16.49062500061451786, -3.027376345333610441, -5.243569643749999898 ) ) ;
#29916 = CARTESIAN_POINT ( 'NONE',  ( 24.75000000122902932, -2.886751345948129988, 4.999999999999997335 ) ) ;
#29917 = CARTESIAN_POINT ( 'NONE',  ( 25.41562500061451146, -6.054752690667223547, -1.112240025338166033E-15 ) ) ;
#29918 = CARTESIAN_POINT ( 'NONE',  ( 22.65937500061451715, 0.000000000000000000, 5.243569643749999010 ) ) ;
#29919 = CARTESIAN_POINT ( 'NONE',  ( 15.29062500061451679, 6.054752690667223547, 3.707466751127219781E-16 ) ) ;
#29920 = CARTESIAN_POINT ( 'NONE',  ( -4.243569643749999898, 16.70937500061451786, 30.00000000000000000 ) ) ;
#29921 = CARTESIAN_POINT ( 'NONE',  ( 21.44062500061452070, -3.027376345333610441, -5.243569643749999898 ) ) ;
#29922 = CARTESIAN_POINT ( 'NONE',  ( 2.925000001229034918, 2.886751345948129099, -4.999999999999998224 ) ) ;
#29923 = ORIENTED_EDGE ( 'NONE', *, *, #25902, .F. ) ;
#29924 = CARTESIAN_POINT ( 'NONE',  ( 24.67500000000000071, -4.330127018922194537, 2.499999999999995559 ) ) ;
#29925 = CARTESIAN_POINT ( 'NONE',  ( -3.999999999999999112, 13.70000000000000107, -30.00000000000000000 ) ) ;
#29926 = CARTESIAN_POINT ( 'NONE',  ( -1.878215178124999163, 19.65312499938548285, 26.74683588394047007 ) ) ;
#29927 = CARTESIAN_POINT ( 'NONE',  ( 2.896875000614518747, -3.027376345333614438, 5.243569643749998122 ) ) ;
#29928 = CARTESIAN_POINT ( 'NONE',  ( 8.315625000614515372, -6.054752690667223547, -1.112240025338166033E-15 ) ) ;
#29929 = CARTESIAN_POINT ( 'NONE',  ( 22.57500000122903572, -5.773502691896255534, -1.060575238724906372E-15 ) ) ;
#29930 = CARTESIAN_POINT ( 'NONE',  ( 26.12812500061451360, 4.541064518000418104, 2.621784821874999949 ) ) ;
#29931 = CARTESIAN_POINT ( 'NONE',  ( 24.52499999999999858, 4.330127018922191873, 2.499999999999999556 ) ) ;
#29932 = CARTESIAN_POINT ( 'NONE',  ( -2.000000000000000000, 15.08750000122903501, -33.46410161513775705 ) ) ;
#29933 = CARTESIAN_POINT ( 'NONE',  ( -2.000000000000000000, 15.53750000122903430, -33.46410161513775705 ) ) ;
#29934 = CARTESIAN_POINT ( 'NONE',  ( 10.41562500061451679, 3.027376345333611329, 5.243569643749999010 ) ) ;
#29935 = ORIENTED_EDGE ( 'NONE', *, *, #41750, .T. ) ;
#29936 = CARTESIAN_POINT ( 'NONE',  ( 26.76562500061451644, -6.054752690667223547, -1.112240025338166033E-15 ) ) ;
#29937 = CARTESIAN_POINT ( 'NONE',  ( 6.928125000614516082, -4.541064518000419881, 2.621784821874995952 ) ) ;
#29938 = CARTESIAN_POINT ( 'NONE',  ( 3.740625000614516527, -3.027376345333614438, 5.243569643749998122 ) ) ;
#29939 = CARTESIAN_POINT ( 'NONE',  ( 16.69687500061451502, 5.492252693125287522, 3.363034840372157021E-16 ) ) ;
#29940 = CARTESIAN_POINT ( 'NONE',  ( 4.670675770459133069, -1.784685619568015635, 4.930540594781983366 ) ) ;
#29941 = CARTESIAN_POINT ( 'NONE',  ( 12.86250000000000071, 2.886751345948126879, 4.999999999999999112 ) ) ;
#29942 = CARTESIAN_POINT ( 'NONE',  ( 12.83437500061451786, -4.541064518000419881, 2.621784821874995952 ) ) ;
#29943 = CARTESIAN_POINT ( 'NONE',  ( 9.900000001229033231, -2.886751345948129988, 4.999999999999997335 ) ) ;
#29944 = CARTESIAN_POINT ( 'NONE',  ( 16.05937500061451573, -4.541064518000417216, -2.621784821875001281 ) ) ;
#29945 = CARTESIAN_POINT ( 'NONE',  ( 18.45000000000000284, -4.330127018922190985, -2.500000000000001332 ) ) ;
#29946 = CARTESIAN_POINT ( 'NONE',  ( 7.659375000614518036, 4.541064518000418104, -2.621784821874998173 ) ) ;
#29947 = CARTESIAN_POINT ( 'NONE',  ( 4.243569643749999898, 10.57812500061451821, -30.00000000000000000 ) ) ;
#29948 = CARTESIAN_POINT ( 'NONE',  ( 4.000000000000000000, 16.58750000000000213, 32.30940107675849760 ) ) ;
#29949 = CARTESIAN_POINT ( 'NONE',  ( 23.74687500061451573, 4.119189519843966529, -2.378215178124998275 ) ) ;
#29950 = CARTESIAN_POINT ( 'NONE',  ( 26.36249999999999716, 2.886751345948113556, 5.000000000000023093 ) ) ;
#29951 = CARTESIAN_POINT ( 'NONE',  ( 23.61562500061451431, -6.054752690667223547, -1.112240025338166033E-15 ) ) ;
#29952 = LINE ( 'NONE', #25132, #53391 ) ;
#29953 = CARTESIAN_POINT ( 'NONE',  ( 28.80937500061451573, 4.541064518000418104, -2.621784821874998173 ) ) ;
#29954 = CARTESIAN_POINT ( 'NONE',  ( 21.03750000000000142, -2.886751345948129988, 4.999999999999997335 ) ) ;
#29955 = CARTESIAN_POINT ( 'NONE',  ( 7.865625000614516971, -6.054752690667223547, -1.112240025338166033E-15 ) ) ;
#29956 = CARTESIAN_POINT ( 'NONE',  ( 24.42187500061451289, -4.119189519843968306, 2.378215178124996054 ) ) ;
#29957 = CARTESIAN_POINT ( 'NONE',  ( 16.05937500061451573, -4.541064518000417216, -2.621784821875001281 ) ) ;
#29958 = CARTESIAN_POINT ( 'NONE',  ( 9.121875000614517504, -4.119189519843968306, 2.378215178124996054 ) ) ;
#29959 = CARTESIAN_POINT ( 'NONE',  ( 29.32500000122903216, -5.773502691896255534, -1.060575238724906372E-15 ) ) ;
#29960 = CARTESIAN_POINT ( 'NONE',  ( 8.034375000614518925, 6.421520780324663323E-16, -5.243569643749999010 ) ) ;
#29961 = ORIENTED_EDGE ( 'NONE', *, *, #38656, .T. ) ;
#29962 = CARTESIAN_POINT ( 'NONE',  ( 18.27187500061451431, -6.054752690667223547, -1.112240025338166033E-15 ) ) ;
#29963 = CARTESIAN_POINT ( 'NONE',  ( -0.5230845267916411911, 25.53603409863758955, 33.97449076415956171 ) ) ;
#29964 = CARTESIAN_POINT ( 'NONE',  ( 26.06250000000000000, -5.773502691896255534, -1.060575238724906372E-15 ) ) ;
#29965 = CARTESIAN_POINT ( 'NONE',  ( 3.600000000000002309, -4.330127018922190985, -2.500000000000001332 ) ) ;
#29966 = CARTESIAN_POINT ( 'NONE',  ( 30.00000000000000000, 0.000000000000000000, 0.000000000000000000 ) ) ;
#29967 = CARTESIAN_POINT ( 'NONE',  ( 10.72500000000000142, -4.330127018922194537, 2.499999999999995559 ) ) ;
#29968 = ORIENTED_EDGE ( 'NONE', *, *, #39854, .F. ) ;
#29969 = CARTESIAN_POINT ( 'NONE',  ( 10.35000000000000142, -4.330127018922190985, -2.500000000000001332 ) ) ;
#29970 = CARTESIAN_POINT ( 'NONE',  ( 10.69687500061451679, 4.119189519843966529, -2.378215178124998275 ) ) ;
#29971 = CARTESIAN_POINT ( 'NONE',  ( 23.57812500061451289, -4.541064518000419881, 2.621784821874995952 ) ) ;
#29972 = CARTESIAN_POINT ( 'NONE',  ( 14.32500000000000107, -4.330127018922194537, 2.499999999999995559 ) ) ;
#29973 = CARTESIAN_POINT ( 'NONE',  ( 7.425000001229034474, 2.886751345948129099, -4.999999999999998224 ) ) ;
#29974 = CARTESIAN_POINT ( 'NONE',  ( 6.665625000614515905, 3.027376345333613106, -5.243569643749998122 ) ) ;
#29975 = CARTESIAN_POINT ( 'NONE',  ( 22.68750000000000000, 5.773502691896255534, 3.535250795749688894E-16 ) ) ;
#29976 = EDGE_CURVE ( 'NONE', #20756, #1724, #26876, .T. ) ;
#29977 = CARTESIAN_POINT ( 'NONE',  ( 20.35312500061451502, 0.000000000000000000, 5.243569643749999010 ) ) ;
#29978 = CARTESIAN_POINT ( 'NONE',  ( 4.117801095115578569, -2.836267711383653634, 4.249660802484540589 ) ) ;
#29979 = CARTESIAN_POINT ( 'NONE',  ( 25.23750000122903359, -4.330127018922194537, 2.499999999999995559 ) ) ;
#29980 = CARTESIAN_POINT ( 'NONE',  ( -3.756430356249999214, 18.22812499938548214, 27.83122392262697176 ) ) ;
#29981 = CARTESIAN_POINT ( 'NONE',  ( 5.812500000000001776, -5.773502691896255534, -1.060575238724906372E-15 ) ) ;
#29982 = VERTEX_POINT ( 'NONE', #52369 ) ;
#29983 = CARTESIAN_POINT ( 'NONE',  ( 21.02812500061451573, 6.421520780324663323E-16, -5.243569643749999010 ) ) ;
#29984 = CARTESIAN_POINT ( 'NONE',  ( 27.89062500061451289, 6.054752690667223547, 3.707466751127219781E-16 ) ) ;
#29985 = CARTESIAN_POINT ( 'NONE',  ( 27.19687500061451857, -3.027376345333614438, 5.243569643749998122 ) ) ;
#29986 = CARTESIAN_POINT ( 'NONE',  ( 14.99062500061451786, -3.027376345333614438, 5.243569643749998122 ) ) ;
#29987 = DIRECTION ( 'NONE',  ( -0.000000000000000000, -1.000000000000000000, -0.000000000000000000 ) ) ;
#29988 = CARTESIAN_POINT ( 'NONE',  ( 26.17500000122903359, -5.773502691896255534, -1.060575238724906372E-15 ) ) ;
#29989 = CARTESIAN_POINT ( 'NONE',  ( 22.32187500061451857, -5.492252693125287522, -1.008910452111647106E-15 ) ) ;
#29990 = CARTESIAN_POINT ( 'NONE',  ( 16.82812500061451644, -4.541064518000419881, 2.621784821874995952 ) ) ;
#29991 = CARTESIAN_POINT ( 'NONE',  ( -1.999999999999997113, 16.92500000000000426, -26.53589838486224295 ) ) ;
#29992 = CARTESIAN_POINT ( 'NONE',  ( 5.812500001229035540, 0.000000000000000000, 4.999999999999998224 ) ) ;
#29993 = CARTESIAN_POINT ( 'NONE',  ( 9.684375000614517504, -4.541064518000419881, 2.621784821874995952 ) ) ;
#29994 = CARTESIAN_POINT ( 'NONE',  ( 10.17187500061451999, -6.054752690667223547, -1.112240025338166033E-15 ) ) ;
#29995 = CARTESIAN_POINT ( 'NONE',  ( 20.97187500061451715, -6.054752690667223547, -1.112240025338166033E-15 ) ) ;
#29996 = ORIENTED_EDGE ( 'NONE', *, *, #34066, .T. ) ;
#29997 = CARTESIAN_POINT ( 'NONE',  ( -3.039972894299037609, 9.532883912050410302, 24.81249067399576447 ) ) ;
#29998 = CARTESIAN_POINT ( 'NONE',  ( 23.05312500061451431, 0.000000000000000000, 5.243569643749999010 ) ) ;
#29999 = CARTESIAN_POINT ( 'NONE',  ( 18.90937500061451360, 4.541064518000418104, -2.621784821874998173 ) ) ;
#30000 = CARTESIAN_POINT ( 'NONE',  ( 23.35312500061451857, 4.541064518000418104, -2.621784821874998173 ) ) ;
#30001 = CARTESIAN_POINT ( 'NONE',  ( 1.071796769724500997, 18.65134618820329848, 33.99999999999999289 ) ) ;
#30002 = CARTESIAN_POINT ( 'NONE',  ( 1.999999999999998668, 14.45000000000000107, 26.53589838486224650 ) ) ;
#30003 = VECTOR ( 'NONE', #61214, 1000.000000000000000 ) ;
#30004 = CARTESIAN_POINT ( 'NONE',  ( 29.42812500061451431, -4.541064518000419881, 2.621784821874995952 ) ) ;
#30005 = CARTESIAN_POINT ( 'NONE',  ( 9.900000001229033231, -2.886751345948129988, 4.999999999999997335 ) ) ;
#30006 = ORIENTED_EDGE ( 'NONE', *, *, #45894, .T. ) ;
#30007 = CARTESIAN_POINT ( 'NONE',  ( 4.200000001229033053, -2.886751345948125991, -5.000000000000000000 ) ) ;
#30008 = CARTESIAN_POINT ( 'NONE',  ( -3.999999999999999112, 19.55000000000000071, -30.00000000000000000 ) ) ;
#30009 = CARTESIAN_POINT ( 'NONE',  ( 28.27500000122903145, 2.886751345948126879, 4.999999999999999112 ) ) ;
#30010 = CARTESIAN_POINT ( 'NONE',  ( -1.878215178124999163, 13.35312499938548392, 26.74683588394047007 ) ) ;
#30011 = CARTESIAN_POINT ( 'NONE',  ( 10.20937500061451786, -4.541064518000417216, -2.621784821875001281 ) ) ;
#30012 = CARTESIAN_POINT ( 'NONE',  ( 3.999999999999998668, 10.02500000122903323, 27.69059892324149530 ) ) ;
#30013 = CARTESIAN_POINT ( 'NONE',  ( 17.16562500061451502, 3.027376345333611329, 5.243569643749999010 ) ) ;
#30014 = CARTESIAN_POINT ( 'NONE',  ( 10.05937500061451750, 0.000000000000000000, 5.243569643749999010 ) ) ;
#30015 = CARTESIAN_POINT ( 'NONE',  ( 28.91250000122903074, -4.330127018922190985, -2.500000000000001332 ) ) ;
#30016 = CARTESIAN_POINT ( 'NONE',  ( 18.94687500061451857, 6.054752690667223547, 3.707466751127219781E-16 ) ) ;
#30017 = CARTESIAN_POINT ( 'NONE',  ( 7.434375000614519280, -4.541064518000419881, 2.621784821874995952 ) ) ;
#30018 = CARTESIAN_POINT ( 'NONE',  ( 8.390625000614518214, -3.027376345333610441, -5.243569643749999898 ) ) ;
#30019 = CARTESIAN_POINT ( 'NONE',  ( 17.72812500061451502, -4.541064518000419881, 2.621784821874995952 ) ) ;
#30020 = ORIENTED_EDGE ( 'NONE', *, *, #65744, .T. ) ;
#30021 = CIRCLE ( 'NONE', #71312, 9.000000000000000000 ) ;
#30022 = CARTESIAN_POINT ( 'NONE',  ( 5.512500001229033941, -4.330127018922190985, -2.500000000000001332 ) ) ;
#30023 = CARTESIAN_POINT ( 'NONE',  ( 15.06562500061451537, -6.054752690667223547, -1.112240025338166033E-15 ) ) ;
#30024 = CARTESIAN_POINT ( 'NONE',  ( 10.30312500061451431, 4.541064518000418104, -2.621784821874998173 ) ) ;
#30025 = CARTESIAN_POINT ( 'NONE',  ( 23.93437500061451573, 4.119189519843966529, 2.378215178124999607 ) ) ;
#30026 = CARTESIAN_POINT ( 'NONE',  ( 10.95000000000000107, 4.330127018922192761, -2.499999999999997780 ) ) ;
#30027 = CARTESIAN_POINT ( 'NONE',  ( 7.725000001229034297, -5.773502691896255534, -1.060575238724906372E-15 ) ) ;
#30028 =( BOUNDED_CURVE ( )  B_SPLINE_CURVE ( 2, ( #14955, #60014, #9425, #43412, #65937, #9785, #32318 ),
 .UNSPECIFIED., .F., .F. ) 
 B_SPLINE_CURVE_WITH_KNOTS ( ( 3, 2, 2, 3 ),
 ( 0.9257108577306782937, 0.9277777777777778123, 0.9305555555555555802, 0.9323466298429085031 ),
 .UNSPECIFIED. ) 
 CURVE ( )  GEOMETRIC_REPRESENTATION_ITEM ( )  RATIONAL_B_SPLINE_CURVE ( ( 0.9489772546989883040, 0.9003106796607971418, 1.000000000000000000, 0.8660254037844387076, 1.000000000000000000, 0.9136149564015341173, 0.9386297746918415008 ) ) 
 REPRESENTATION_ITEM ( '' )  );
#30029 = ADVANCED_FACE ( 'NONE', ( #70815 ), #20190, .F. ) ;
#30030 = CARTESIAN_POINT ( 'NONE',  ( 14.63437500061451679, -4.541064518000419881, 2.621784821874995952 ) ) ;
#30031 = CARTESIAN_POINT ( 'NONE',  ( 17.36250000122903359, 4.330127018922192761, -2.499999999999997780 ) ) ;
#30032 = B_SPLINE_CURVE_WITH_KNOTS ( 'NONE', 3,
 ( #44205, #56007, #33461, #65994, #32374, #4321, #26846, #71909, #10212, #50106 ),
 .UNSPECIFIED., .F., .F.,
 ( 4, 3, 3, 4 ),
 ( 1.795354992613655247E-16, 0.0001572292605084571135, 0.0003224816258534031780, 0.0004877840086384408781 ),
 .UNSPECIFIED. ) ;
#30033 = CARTESIAN_POINT ( 'NONE',  ( 25.53750000000000142, -2.886751345948129988, 4.999999999999997335 ) ) ;
#30034 = EDGE_CURVE ( 'NONE', #67801, #46954, #21677, .T. ) ;
#30035 = CARTESIAN_POINT ( 'NONE',  ( 2.121784821875001281, 17.70312500061451644, -26.32496088578401938 ) ) ;
#30036 = CARTESIAN_POINT ( 'NONE',  ( -2.000000000000001776, 13.25000000000000178, 33.46410161513775705 ) ) ;
#30037 = CARTESIAN_POINT ( 'NONE',  ( 3.242103837493086330E-14, 11.00000000122903288, -34.00000000000000000 ) ) ;
#30038 = CARTESIAN_POINT ( 'NONE',  ( 4.607378645714853782, 3.612521970890910872, 4.230067690458080953 ) ) ;
#30039 = CARTESIAN_POINT ( 'NONE',  ( 17.33437500061451431, -4.541064518000419881, 2.621784821874995952 ) ) ;
#30040 = ADVANCED_FACE ( 'NONE', ( #31291 ), #65636, .T. ) ;
#30041 = CARTESIAN_POINT ( 'NONE',  ( 18.35625000122903216, 0.000000000000000000, 4.999999999999998224 ) ) ;
#30042 = CARTESIAN_POINT ( 'NONE',  ( 14.27812500061451573, 6.421520780324663323E-16, -5.243569643749999010 ) ) ;
#30043 = CARTESIAN_POINT ( 'NONE',  ( 9.768750001229035362, 2.886751345948126879, 4.999999999999999112 ) ) ;
#30044 = DIRECTION ( 'NONE',  ( -1.000000000000000000, -0.000000000000000000, -0.000000000000000000 ) ) ;
#30045 = CARTESIAN_POINT ( 'NONE',  ( 25.73437500061451644, 4.541064518000418104, 2.621784821874999949 ) ) ;
#30046 = CARTESIAN_POINT ( 'NONE',  ( 17.29687500061451644, -4.119189519843965641, -2.378215178125001383 ) ) ;
#30047 = CARTESIAN_POINT ( 'NONE',  ( 10.07812500061451644, -4.541064518000419881, 2.621784821874995952 ) ) ;
#30048 = CARTESIAN_POINT ( 'NONE',  ( 16.28437500061452070, 4.541064518000418104, 2.621784821874999949 ) ) ;
#30049 = ORIENTED_EDGE ( 'NONE', *, *, #54952, .T. ) ;
#30050 = CARTESIAN_POINT ( 'NONE',  ( 27.23437500061451644, -4.541064518000419881, 2.621784821874995952 ) ) ;
#30051 = CARTESIAN_POINT ( 'NONE',  ( 28.67812500061451431, 6.421520780324663323E-16, -5.243569643749999010 ) ) ;
#30052 = CARTESIAN_POINT ( 'NONE',  ( 19.90312500061451573, 0.000000000000000000, 5.243569643749999010 ) ) ;
#30053 = CARTESIAN_POINT ( 'NONE',  ( 28.97812500061451502, -4.541064518000419881, 2.621784821874995952 ) ) ;
#30054 = EDGE_CURVE ( 'NONE', #14839, #1970, #46585, .T. ) ;
#30055 = CARTESIAN_POINT ( 'NONE',  ( 2.000000000000001332, 14.75000000000000178, 33.46410161513774995 ) ) ;
#30056 = AXIS2_PLACEMENT_3D ( 'NONE', #32233, #48866, #38880 ) ;
#30057 = CARTESIAN_POINT ( 'NONE',  ( 10.08749999999999858, 5.773502691896255534, 3.535250795749688894E-16 ) ) ;
#30058 = CARTESIAN_POINT ( 'NONE',  ( 20.47500000122903074, 2.886751345948129099, -4.999999999999998224 ) ) ;
#30059 = CARTESIAN_POINT ( 'NONE',  ( 0.000000000000000000, 20.00000000000000000, 30.00000000000000000 ) ) ;
#30060 = CARTESIAN_POINT ( 'NONE',  ( 11.52187500061451608, 5.824947211148865298E-16, -4.756430356249998326 ) ) ;
#30061 = ORIENTED_EDGE ( 'NONE', *, *, #66541, .T. ) ;
#30062 = CARTESIAN_POINT ( 'NONE',  ( 18.22499999999999787, 4.330127018922191873, 2.499999999999999556 ) ) ;
#30063 = CARTESIAN_POINT ( 'NONE',  ( 20.54999999999999716, 0.000000000000000000, 4.999999999999998224 ) ) ;
#30064 = CARTESIAN_POINT ( 'NONE',  ( 18.49687500061452283, 6.054752690667223547, 3.707466751127219781E-16 ) ) ;
#30065 = CARTESIAN_POINT ( 'NONE',  ( 14.61562500061451608, -6.054752690667223547, -1.112240025338166033E-15 ) ) ;
#30066 = VERTEX_POINT ( 'NONE', #47925 ) ;
#30067 = CARTESIAN_POINT ( 'NONE',  ( 3.637500001229036162, -4.330127018922194537, 2.499999999999995559 ) ) ;
#30068 = CARTESIAN_POINT ( 'NONE',  ( 6.815625000614517148, 3.027376345333611329, 5.243569643749999010 ) ) ;
#30069 = CARTESIAN_POINT ( 'NONE',  ( 12.03749999999999964, -2.886751345948129988, 4.999999999999997335 ) ) ;
#30070 = CARTESIAN_POINT ( 'NONE',  ( 27.53437500061451715, -2.746126346562646425, 4.756430356249996549 ) ) ;
#30071 = CARTESIAN_POINT ( 'NONE',  ( -2.121784821874996840, 16.27812500061451573, 33.67503911421598417 ) ) ;
#30072 = CARTESIAN_POINT ( 'NONE',  ( 28.67812500061451431, 6.421520780324663323E-16, -5.243569643749999010 ) ) ;
#30073 = CARTESIAN_POINT ( 'NONE',  ( 8.625000000000000000, 6.123233995736764310E-16, -4.999999999999998224 ) ) ;
#30074 = VECTOR ( 'NONE', #67820, 1000.000000000000000 ) ;
#30075 = CARTESIAN_POINT ( 'NONE',  ( 3.756430356250000546, 16.72812499938548214, 27.83122392262697886 ) ) ;
#30076 = CARTESIAN_POINT ( 'NONE',  ( 24.72187500061451360, 3.027376345333613106, -5.243569643749998122 ) ) ;
#30077 = ORIENTED_EDGE ( 'NONE', *, *, #54489, .T. ) ;
#30078 = CARTESIAN_POINT ( 'NONE',  ( 22.49062500061451431, 6.054752690667223547, 3.707466751127219781E-16 ) ) ;
#30079 = CARTESIAN_POINT ( 'NONE',  ( 23.18437500061451573, -4.541064518000419881, 2.621784821874995952 ) ) ;
#30080 = CARTESIAN_POINT ( 'NONE',  ( -3.000416591977282496E-16, 15.64062500061459282, -34.90005215228797653 ) ) ;
#30081 = CARTESIAN_POINT ( 'NONE',  ( 5.690625000614516260, -3.027376345333610441, -5.243569643749999898 ) ) ;
#30082 = CARTESIAN_POINT ( 'NONE',  ( 28.17187500061451644, -5.492252693125287522, -1.008910452111647106E-15 ) ) ;
#30083 = CARTESIAN_POINT ( 'NONE',  ( 24.47812500061451502, -4.541064518000419881, 2.621784821874995952 ) ) ;
#30084 = CARTESIAN_POINT ( 'NONE',  ( 28.09687500061451715, -4.119189519843965641, -2.378215178125001383 ) ) ;
#30085 = CARTESIAN_POINT ( 'NONE',  ( 9.684375000614517504, -4.119189519843968306, 2.378215178124996054 ) ) ;
#30086 = CARTESIAN_POINT ( 'NONE',  ( 17.37187500061451573, -6.054752690667223547, -1.112240025338166033E-15 ) ) ;
#30087 = CARTESIAN_POINT ( 'NONE',  ( 18.94687500061451502, 6.054752690667223547, 3.707466751127219781E-16 ) ) ;
#30088 = CARTESIAN_POINT ( 'NONE',  ( 26.18437500061451573, 4.541064518000418104, 2.621784821874999949 ) ) ;
#30089 = CARTESIAN_POINT ( 'NONE',  ( -2.121784821874996840, 15.43437500061451928, 33.67503911421598417 ) ) ;
#30090 = CARTESIAN_POINT ( 'NONE',  ( 7.303125000614516082, 0.000000000000000000, 5.243569643749999010 ) ) ;
#30092 =( BOUNDED_CURVE ( )  B_SPLINE_CURVE ( 2, ( #62246, #56695, #16805, #60776, #38247, #43806, #28626 ),
 .UNSPECIFIED., .F., .F. ) 
 B_SPLINE_CURVE_WITH_KNOTS ( ( 3, 2, 2, 3 ),
 ( 0.7800000000000001377, 0.7833333333333334370, 0.7866666666666667362, 0.7900000000000001465 ),
 .UNSPECIFIED. ) 
 CURVE ( )  GEOMETRIC_REPRESENTATION_ITEM ( )  RATIONAL_B_SPLINE_CURVE ( ( 0.9999999999999955591, 0.8660254037844431485, 1.000000000000000000, 0.8660254037844387076, 1.000000000000000000, 0.8660254037844342667, 1.000000000000004441 ) ) 
 REPRESENTATION_ITEM ( '' )  );
#30091 = CARTESIAN_POINT ( 'NONE',  ( -1.071796769724491005, 19.00759618943233775, 26.00000000000000355 ) ) ;
#30093 = CARTESIAN_POINT ( 'NONE',  ( 4.884375000614518569, 6.421520780324663323E-16, -5.243569643749999010 ) ) ;
#30094 = CARTESIAN_POINT ( 'NONE',  ( 34.99999999999999289, 2.500000000000000444, 3.499999999999999112 ) ) ;
#30095 = CARTESIAN_POINT ( 'NONE',  ( 4.040625000614517681, 6.054752690667223547, 3.707466751127219781E-16 ) ) ;
#30096 = CARTESIAN_POINT ( 'NONE',  ( 9.309375000614517504, -4.541064518000417216, -2.621784821875001281 ) ) ;
#30097 =( NAMED_UNIT ( * ) SI_UNIT ( $, .STERADIAN. ) SOLID_ANGLE_UNIT ( ) );
#30098 = CARTESIAN_POINT ( 'NONE',  ( 17.62500000122903288, -5.773502691896255534, -1.060575238724906372E-15 ) ) ;
#30099 = CARTESIAN_POINT ( 'NONE',  ( 4.434375000614519280, 6.421520780324663323E-16, -5.243569643749999010 ) ) ;
#30100 = CARTESIAN_POINT ( 'NONE',  ( 7.865625000614516971, -6.054752690667223547, -1.112240025338166033E-15 ) ) ;
#30101 = CARTESIAN_POINT ( 'NONE',  ( 2.828200636599751609E-16, 13.00624999877096677, 25.38119784648299415 ) ) ;
#30102 = CARTESIAN_POINT ( 'NONE',  ( 23.45625000122903359, -4.330127018922190985, -2.500000000000001332 ) ) ;
#30103 = CARTESIAN_POINT ( 'NONE',  ( 17.70937500061451431, 0.000000000000000000, 5.243569643749999010 ) ) ;
#30104 = CARTESIAN_POINT ( 'NONE',  ( 45.00000000000000000, 9.426999614876460059E-14, 7.499999999999999112 ) ) ;
#30105 = ORIENTED_EDGE ( 'NONE', *, *, #26979, .F. ) ;
#30106 = CARTESIAN_POINT ( 'NONE',  ( 23.84062500061451928, 6.054752690667223547, 3.707466751127219781E-16 ) ) ;
#30107 = CARTESIAN_POINT ( 'NONE',  ( 10.60312500061451679, -4.541064518000417216, -2.621784821875001281 ) ) ;
#30108 = CARTESIAN_POINT ( 'NONE',  ( 25.99687500061451928, -3.027376345333610441, -5.243569643749999898 ) ) ;
#30109 = CARTESIAN_POINT ( 'NONE',  ( 10.90312500061451928, 0.000000000000000000, 5.243569643749999010 ) ) ;
#30110 = CARTESIAN_POINT ( 'NONE',  ( 23.15625000122903288, 4.330127018922192761, -2.499999999999997780 ) ) ;
#30111 = CARTESIAN_POINT ( 'NONE',  ( 10.46250000122903323, -4.330127018922190985, -2.500000000000001332 ) ) ;
#30112 = CARTESIAN_POINT ( 'NONE',  ( 25.56562500061452070, 3.027376345333613106, -5.243569643749998122 ) ) ;
#30113 = CARTESIAN_POINT ( 'NONE',  ( -4.243569643749997233, 12.19062500061451715, -27.54997392385601174 ) ) ;
#30114 = CARTESIAN_POINT ( 'NONE',  ( 13.61250000122903359, -4.330127018922190985, -2.500000000000001332 ) ) ;
#30115 = CARTESIAN_POINT ( 'NONE',  ( 20.99062500061451431, -3.027376345333610441, -5.243569643749999898 ) ) ;
#30116 = VECTOR ( 'NONE', #31365, 1000.000000000000000 ) ;
#30117 = CARTESIAN_POINT ( 'NONE',  ( 21.36562500061451431, -6.054752690667223547, -1.112240025338166033E-15 ) ) ;
#30118 = CARTESIAN_POINT ( 'NONE',  ( 29.78437500061451715, 4.119189519843966529, 2.378215178124999607 ) ) ;
#30119 = CARTESIAN_POINT ( 'NONE',  ( 21.18749999999999645, -2.886751345948125991, -5.000000000000000000 ) ) ;
#30120 = CARTESIAN_POINT ( 'NONE',  ( 14.21250000122903323, 4.330127018922192761, -2.499999999999997780 ) ) ;
#30121 = VECTOR ( 'NONE', #33268, 1000.000000000000000 ) ;
#30122 = CARTESIAN_POINT ( 'NONE',  ( 10.56562500061451715, -6.054752690667223547, -1.112240025338166033E-15 ) ) ;
#30123 = CARTESIAN_POINT ( 'NONE',  ( 13.26562500061451644, -6.054752690667223547, -1.112240025338166033E-15 ) ) ;
#30124 = AXIS2_PLACEMENT_3D ( 'NONE', #3100, #70691, #9008 ) ;
#30125 = CARTESIAN_POINT ( 'NONE',  ( 25.57500000122903216, 2.886751345948126879, 4.999999999999999112 ) ) ;
#30126 = VECTOR ( 'NONE', #69072, 1000.000000000000000 ) ;
#30127 = CARTESIAN_POINT ( 'NONE',  ( 21.83437500061451786, -4.541064518000419881, 2.621784821874995952 ) ) ;
#30128 = CARTESIAN_POINT ( 'NONE',  ( 25.46249999999999858, 2.886751345948140646, 4.999999999999974243 ) ) ;
#30129 = EDGE_CURVE ( 'NONE', #63662, #56329, #71920, .T. ) ;
#30130 = CARTESIAN_POINT ( 'NONE',  ( 8.775000001229033231, 2.886751345948129099, -4.999999999999998224 ) ) ;
#30131 = CARTESIAN_POINT ( 'NONE',  ( 7.959375000614516971, -4.541064518000417216, -2.621784821875001281 ) ) ;
#30132 = CARTESIAN_POINT ( 'NONE',  ( 26.82187500061451857, -6.054752690667223547, -1.112240025338166033E-15 ) ) ;
#30133 = EDGE_CURVE ( 'NONE', #49995, #11143, #29229, .T. ) ;
#30134 = CARTESIAN_POINT ( 'NONE',  ( 3.384375000614517237, -4.541064518000419881, 2.621784821874995952 ) ) ;
#30135 = CARTESIAN_POINT ( 'NONE',  ( 22.37812500061451360, 6.421520780324663323E-16, -5.243569643749999010 ) ) ;
#30136 = CARTESIAN_POINT ( 'NONE',  ( 27.49687500061451217, 6.054752690667223547, 3.707466751127219781E-16 ) ) ;
#30137 = CARTESIAN_POINT ( 'NONE',  ( -7.967954043666661671E-16, 17.14062499938548356, 34.33755215474603517 ) ) ;
#30138 = CARTESIAN_POINT ( 'NONE',  ( 19.40625000122902932, -4.330127018922190985, -2.500000000000001332 ) ) ;
#30139 = CARTESIAN_POINT ( 'NONE',  ( 8.109375000614518214, 4.541064518000418104, -2.621784821874998173 ) ) ;
#30140 = CARTESIAN_POINT ( 'NONE',  ( 16.82812500061451644, -4.541064518000419881, 2.621784821874995952 ) ) ;
#30141 = ORIENTED_EDGE ( 'NONE', *, *, #11564, .T. ) ;
#30142 = CARTESIAN_POINT ( 'NONE',  ( 2.867942972713479755, -4.095717654485441450, 3.274159358307527690 ) ) ;
#30143 = CARTESIAN_POINT ( 'NONE',  ( 27.51562500061451644, 3.027376345333611329, 5.243569643749999010 ) ) ;
#30144 = CARTESIAN_POINT ( 'NONE',  ( 4.696875000614518569, -3.027376345333614438, 5.243569643749998122 ) ) ;
#30145 = CARTESIAN_POINT ( 'NONE',  ( 27.61875000122903145, 2.886751345948142866, -4.999999999999973355 ) ) ;
#30146 = CARTESIAN_POINT ( 'NONE',  ( 16.64999999999999858, -4.330127018922190985, -2.500000000000001332 ) ) ;
#30147 = CARTESIAN_POINT ( 'NONE',  ( 20.65312500061451573, 4.541064518000418104, -2.621784821874998173 ) ) ;
#30148 = ORIENTED_EDGE ( 'NONE', *, *, #53983, .T. ) ;
#30149 = CARTESIAN_POINT ( 'NONE',  ( 24.52499999999999858, 4.330127018922191873, 2.499999999999999556 ) ) ;
#30150 = CARTESIAN_POINT ( 'NONE',  ( 25.54687500061451644, -3.027376345333610441, -5.243569643749999898 ) ) ;
#30151 = ORIENTED_EDGE ( 'NONE', *, *, #32136, .F. ) ;
#30152 = CARTESIAN_POINT ( 'NONE',  ( 13.34062500061451750, -3.027376345333610441, -5.243569643749999898 ) ) ;
#30153 = CARTESIAN_POINT ( 'NONE',  ( 5.053125000614517859, 0.000000000000000000, 5.243569643749999010 ) ) ;
#30154 = CARTESIAN_POINT ( 'NONE',  ( 15.49687500061451573, -4.119189519843965641, -2.378215178125001383 ) ) ;
#30155 = CARTESIAN_POINT ( 'NONE',  ( 3.421875000614516882, -6.054752690667223547, -1.112240025338166033E-15 ) ) ;
#30156 = CARTESIAN_POINT ( 'NONE',  ( 15.00000000122903465, -2.886751345948125991, -5.000000000000000000 ) ) ;
#30157 = VECTOR ( 'NONE', #44585, 1000.000000000000000 ) ;
#30158 = CARTESIAN_POINT ( 'NONE',  ( 20.66250000000000142, -5.773502691896255534, -1.060575238724906372E-15 ) ) ;
#30159 = CARTESIAN_POINT ( 'NONE',  ( 29.55000000000000071, 0.000000000000000000, 4.999999999999998224 ) ) ;
#30160 = CARTESIAN_POINT ( 'NONE',  ( 3.684375000614518836, 4.541064518000418104, 2.621784821874999949 ) ) ;
#30161 = CARTESIAN_POINT ( 'NONE',  ( 8.821875000614518569, -6.054752690667223547, -1.112240025338166033E-15 ) ) ;
#30162 = CARTESIAN_POINT ( 'NONE',  ( 18.94687500061451502, 6.054752690667223547, 3.707466751127219781E-16 ) ) ;
#30163 = CARTESIAN_POINT ( 'NONE',  ( 11.60625000122903216, 0.000000000000000000, 4.999999999999998224 ) ) ;
#30164 = ORIENTED_EDGE ( 'NONE', *, *, #46331, .F. ) ;
#30165 = CARTESIAN_POINT ( 'NONE',  ( 28.37812500061451715, 4.541064518000418104, 2.621784821874999949 ) ) ;
#30166 = CARTESIAN_POINT ( 'NONE',  ( 29.82187500061451502, 3.027376345333611329, 5.243569643749999010 ) ) ;
#30167 = CIRCLE ( 'NONE', #47847, 1.500000000000000444 ) ;
#30169 = ADVANCED_FACE ( 'NONE', ( #26116 ), #25754, .T. ) ;
#30168 = CARTESIAN_POINT ( 'NONE',  ( 3.834375000614519635, -4.541064518000419881, 2.621784821874995952 ) ) ;
#30170 = CARTESIAN_POINT ( 'NONE',  ( 15.82499999999999929, 6.123233995736764310E-16, -4.999999999999998224 ) ) ;
#30171 = CARTESIAN_POINT ( 'NONE',  ( 13.34062500061451750, -3.027376345333610441, -5.243569643749999898 ) ) ;
#30172 = CARTESIAN_POINT ( 'NONE',  ( 1.071796769724491893, 13.94509619066136707, 33.99999999999999289 ) ) ;
#30173 = CARTESIAN_POINT ( 'NONE',  ( 8.268750001229030033, 2.886751345948073588, -5.000000000000094147 ) ) ;
#30174 = CARTESIAN_POINT ( 'NONE',  ( 19.53750000122903430, 6.123233995736764310E-16, -4.999999999999998224 ) ) ;
#30175 = CARTESIAN_POINT ( 'NONE',  ( 3.038088735723376566, 9.529008066655457299, 24.82235102052792541 ) ) ;
#30176 = CARTESIAN_POINT ( 'NONE',  ( 18.34687500061451715, -2.746126346562642428, -4.756430356249999214 ) ) ;
#30177 = CARTESIAN_POINT ( 'NONE',  ( 8.203125000614518214, 0.000000000000000000, 5.243569643749999010 ) ) ;
#30178 = CARTESIAN_POINT ( 'NONE',  ( 24.27187500061452141, 3.027376345333613106, -5.243569643749998122 ) ) ;
#30179 = CARTESIAN_POINT ( 'NONE',  ( 26.96250000122903145, 0.000000000000000000, 4.999999999999998224 ) ) ;
#30180 = CARTESIAN_POINT ( 'NONE',  ( 27.38437500061451857, 6.421520780324663323E-16, -5.243569643749999010 ) ) ;
#30181 = CARTESIAN_POINT ( 'NONE',  ( 7.425000000000000711, 4.330127018922191873, 2.499999999999999556 ) ) ;
#30182 = CARTESIAN_POINT ( 'NONE',  ( 3.999999999999998668, 13.17500000122903359, 27.69059892324149175 ) ) ;
#30183 = CARTESIAN_POINT ( 'NONE',  ( 15.06562500061451537, -6.054752690667223547, -1.112240025338166033E-15 ) ) ;
#30184 = CARTESIAN_POINT ( 'NONE',  ( 6.450000001229034829, -2.886751345948125991, -5.000000000000000000 ) ) ;
#30185 = AXIS2_PLACEMENT_3D ( 'NONE', #4910, #9354, #48882 ) ;
#30186 = CARTESIAN_POINT ( 'NONE',  ( 12.38437500061451857, -4.541064518000419881, 2.621784821874995952 ) ) ;
#30187 = CARTESIAN_POINT ( 'NONE',  ( 45.00000000000000000, 0.000000000000000000, 0.000000000000000000 ) ) ;
#30188 = ORIENTED_EDGE ( 'NONE', *, *, #17491, .F. ) ;
#30189 = CARTESIAN_POINT ( 'NONE',  ( 11.84062500061451750, -3.027376345333614438, 5.243569643749998122 ) ) ;
#30190 = AXIS2_PLACEMENT_3D ( 'NONE', #72399, #9254, #55053 ) ;
#30191 = CARTESIAN_POINT ( 'NONE',  ( -1.626862140677534273E-15, 19.53124999877096357, 34.00000000000000000 ) ) ;
#30192 = CARTESIAN_POINT ( 'NONE',  ( 23.73750000122903359, 4.330127018922191873, 2.499999999999999556 ) ) ;
#30193 = CARTESIAN_POINT ( 'NONE',  ( 11.93437500061451573, -4.541064518000419881, 2.621784821874995952 ) ) ;
#30194 = CARTESIAN_POINT ( 'NONE',  ( 14.69062500061451537, -3.027376345333610441, -5.243569643749999898 ) ) ;
#30195 = CARTESIAN_POINT ( 'NONE',  ( 19.70625000122903359, 0.000000000000000000, 4.999999999999998224 ) ) ;
#30196 = CARTESIAN_POINT ( 'NONE',  ( 24.79687500061451999, 6.054752690667223547, 3.707466751127219781E-16 ) ) ;
#30197 = CARTESIAN_POINT ( 'NONE',  ( 8.512499999999999289, -5.773502691896255534, -1.060575238724906372E-15 ) ) ;
#30198 = CARTESIAN_POINT ( 'NONE',  ( 7.575000000000001954, -4.330127018922194537, 2.499999999999995559 ) ) ;
#30199 = CARTESIAN_POINT ( 'NONE',  ( 0.000000000000000000, 20.00000000000000000, 30.00000000000000000 ) ) ;
#30200 = CARTESIAN_POINT ( 'NONE',  ( -4.243569643749999898, 17.57187500061451502, -32.45002607614398471 ) ) ;
#30201 = CARTESIAN_POINT ( 'NONE',  ( 15.68437500061451573, 6.421520780324663323E-16, -5.243569643749999010 ) ) ;
#30202 = CARTESIAN_POINT ( 'NONE',  ( 17.81250000122903288, 4.330127018922192761, -2.499999999999997780 ) ) ;
#30203 = CARTESIAN_POINT ( 'NONE',  ( 13.24687500061451750, -3.027376345333614438, 5.243569643749998122 ) ) ;
#30204 = CARTESIAN_POINT ( 'NONE',  ( -4.243569643749999898, 10.37187500061451750, 27.54997392385601529 ) ) ;
#30205 = CARTESIAN_POINT ( 'NONE',  ( 20.47500000122903074, 2.886751345948129099, -4.999999999999998224 ) ) ;
#30206 = CARTESIAN_POINT ( 'NONE',  ( 13.45312500061451466, 4.541064518000418104, -2.621784821874998173 ) ) ;
#30207 = VERTEX_POINT ( 'NONE', #59346 ) ;
#30208 = VERTEX_POINT ( 'NONE', #37561 ) ;
#30209 = CARTESIAN_POINT ( 'NONE',  ( 17.51249999999999929, -5.773502691896255534, -1.060575238724906372E-15 ) ) ;
#30210 = CARTESIAN_POINT ( 'NONE',  ( 11.93437500061451573, -4.541064518000419881, 2.621784821874995952 ) ) ;
#30211 = CARTESIAN_POINT ( 'NONE',  ( 1.095284332908920577, 4.886121113889973167, 26.14314022704991203 ) ) ;
#30212 = CARTESIAN_POINT ( 'NONE',  ( 12.93750000122903465, 4.330127018922191873, 2.499999999999999556 ) ) ;
#30213 = CARTESIAN_POINT ( 'NONE',  ( 21.37500000122902932, 2.886751345948129099, -4.999999999999998224 ) ) ;
#30214 = CARTESIAN_POINT ( 'NONE',  ( 18.02812500061451573, 4.541064518000418104, 2.621784821874999949 ) ) ;
#30215 = CARTESIAN_POINT ( 'NONE',  ( 23.80312500061451786, 4.541064518000418104, -2.621784821874998173 ) ) ;
#30216 = CARTESIAN_POINT ( 'NONE',  ( 29.13750000122903216, 4.330127018922191873, 2.499999999999999556 ) ) ;
#30217 = CARTESIAN_POINT ( 'NONE',  ( 28.01249999999999574, 2.886751345948129099, -4.999999999999998224 ) ) ;
#30218 = CARTESIAN_POINT ( 'NONE',  ( 3.756430356250000546, 12.67812499938548143, 27.83122392262697886 ) ) ;
#30219 = AXIS2_PLACEMENT_3D ( 'NONE', #26024, #48933, #21202 ) ;
#30220 = CARTESIAN_POINT ( 'NONE',  ( 28.57499999999999929, 4.330127018922191873, 2.499999999999999556 ) ) ;
#30221 = CARTESIAN_POINT ( 'NONE',  ( 27.60937500061451644, 0.000000000000000000, 5.243569643749999010 ) ) ;
#30222 = CARTESIAN_POINT ( 'NONE',  ( 4.003764151685233585, -2.995052564723633903, -4.167540328934556726 ) ) ;
#30223 = CARTESIAN_POINT ( 'NONE',  ( 4.243569643749999898, 15.09687500061451892, -27.54997392385601529 ) ) ;
#30224 = CARTESIAN_POINT ( 'NONE',  ( 3.262500001229035718, -4.330127018922190985, -2.500000000000001332 ) ) ;
#30225 = CARTESIAN_POINT ( 'NONE',  ( 6.899999999999999467, 4.330127018922192761, -2.499999999999997780 ) ) ;
#30226 = EDGE_CURVE ( 'NONE', #829, #57985, #72603, .T. ) ;
#30227 = CARTESIAN_POINT ( 'NONE',  ( 2.929078911596073365, -4.327287789770789317, 2.992056976644557942 ) ) ;
#30228 = CARTESIAN_POINT ( 'NONE',  ( 10.09687500061451715, -3.027376345333614438, 5.243569643749998122 ) ) ;
#30229 = CARTESIAN_POINT ( 'NONE',  ( 29.61562500061451431, 3.027376345333613106, -5.243569643749998122 ) ) ;
#30230 = CARTESIAN_POINT ( 'NONE',  ( 1.626862140677534273E-15, 10.66249999999999964, 34.00000000000000000 ) ) ;
#30231 = CARTESIAN_POINT ( 'NONE',  ( -5.191270968837354616, 8.550562458943611333, -26.96705733337210376 ) ) ;
#30232 = DIRECTION ( 'NONE',  ( 0.000000000000000000, 0.000000000000000000, 1.000000000000000000 ) ) ;
#30233 = CARTESIAN_POINT ( 'NONE',  ( 7.246875000614518392, 6.054752690667223547, 3.707466751127219781E-16 ) ) ;
#30234 = CARTESIAN_POINT ( 'NONE',  ( 11.89687500061451608, -3.027376345333614438, 5.243569643749998122 ) ) ;
#30235 = CARTESIAN_POINT ( 'NONE',  ( 7.087499999999999467, -2.886751345948129988, 4.999999999999997335 ) ) ;
#30236 = CARTESIAN_POINT ( 'NONE',  ( 4.243569643749999898, 14.62812500061459531, 30.00000000000000000 ) ) ;
#30237 = CARTESIAN_POINT ( 'NONE',  ( 45.00000000000000000, 0.000000000000000000, 4.999999999999998224 ) ) ;
#30238 = CARTESIAN_POINT ( 'NONE',  ( 7.087499999999999467, -2.886751345948129988, 4.999999999999997335 ) ) ;
#30239 = CARTESIAN_POINT ( 'NONE',  ( 14.33437500061451431, 5.492252693125287522, 3.363034840372157021E-16 ) ) ;
#30240 = CARTESIAN_POINT ( 'NONE',  ( 19.11562500061451431, -6.054752690667223547, -1.112240025338166033E-15 ) ) ;
#30241 = CARTESIAN_POINT ( 'NONE',  ( 13.49062500061451608, 6.054752690667223547, 3.707466751127219781E-16 ) ) ;
#30242 = CARTESIAN_POINT ( 'NONE',  ( 23.82187500061451502, 4.119189519843966529, 2.378215178124999607 ) ) ;
#30243 = CARTESIAN_POINT ( 'NONE',  ( 10.13437500061451679, -4.541064518000419881, 2.621784821874995952 ) ) ;
#30244 = CARTESIAN_POINT ( 'NONE',  ( 25.83749999999999858, 5.773502691896255534, 3.535250795749688894E-16 ) ) ;
#30245 = CARTESIAN_POINT ( 'NONE',  ( 22.76250000122903216, 4.330127018922192761, -2.499999999999997780 ) ) ;
#30246 = CARTESIAN_POINT ( 'NONE',  ( 17.13749999999999929, -2.886751345948159742, -4.999999999999942268 ) ) ;
#30247 = CARTESIAN_POINT ( 'NONE',  ( 12.23437500061451821, 4.541064518000418104, 2.621784821874999949 ) ) ;
#30248 = CARTESIAN_POINT ( 'NONE',  ( 27.45937500061451786, 4.541064518000418104, -2.621784821874998173 ) ) ;
#30249 = AXIS2_PLACEMENT_3D ( 'NONE', #66100, #15478, #65364 ) ;
#30250 = CARTESIAN_POINT ( 'NONE',  ( 3.346875000614518036, -3.027376345333614438, 5.243569643749998122 ) ) ;
#30251 = CARTESIAN_POINT ( 'NONE',  ( 24.37500000122903288, -5.773502691896255534, -1.060575238724906372E-15 ) ) ;
#30252 = CARTESIAN_POINT ( 'NONE',  ( 20.03437500061451715, -4.541064518000419881, 2.621784821874995952 ) ) ;
#30253 = CARTESIAN_POINT ( 'NONE',  ( 11.37187500061451750, 3.027376345333611329, 5.243569643749999010 ) ) ;
#30254 = CARTESIAN_POINT ( 'NONE',  ( 3.756430356250000546, 19.54062499938548214, 27.83122392262697886 ) ) ;
#30255 = CARTESIAN_POINT ( 'NONE',  ( 23.81250000000000000, -5.773502691896255534, -1.060575238724906372E-15 ) ) ;
#30256 = CARTESIAN_POINT ( 'NONE',  ( 1.878215178124997609, 20.21562499938548285, 33.25316411605952993 ) ) ;
#30257 = CARTESIAN_POINT ( 'NONE',  ( 2.121784821875001281, 11.00937500061451857, -26.32496088578401938 ) ) ;
#30258 = CARTESIAN_POINT ( 'NONE',  ( 27.90937500061451715, 4.119189519843966529, -2.378215178124998275 ) ) ;
#30259 = CARTESIAN_POINT ( 'NONE',  ( 15.25312500061451715, 4.541064518000418104, -2.621784821874998173 ) ) ;
#30260 = CARTESIAN_POINT ( 'NONE',  ( 5.475000000000000533, 6.123233995736764310E-16, -4.999999999999998224 ) ) ;
#30261 = CARTESIAN_POINT ( 'NONE',  ( 6.937500001229033764, 6.123233995736764310E-16, -4.999999999999998224 ) ) ;
#30262 = CARTESIAN_POINT ( 'NONE',  ( -3.999999999999997335, 13.28749999999999964, -27.69059892324149530 ) ) ;
#30263 = CARTESIAN_POINT ( 'NONE',  ( 15.18750000000000000, -2.886751345948129988, 4.999999999999997335 ) ) ;
#30264 = CARTESIAN_POINT ( 'NONE',  ( 4.243569643749999010, 10.16562500061451857, 27.54997392385601174 ) ) ;
#30265 = CARTESIAN_POINT ( 'NONE',  ( 14.81250000122903288, 0.000000000000000000, 4.999999999999998224 ) ) ;
#30266 = CARTESIAN_POINT ( 'NONE',  ( 24.27187500061452141, 3.027376345333613106, -5.243569643749998122 ) ) ;
#30267 = CARTESIAN_POINT ( 'NONE',  ( 1.592000809091587073E-14, 16.28750000000000142, -34.00000000000000000 ) ) ;
#30268 = EDGE_LOOP ( 'NONE', ( #63748, #25160, #52739, #26298 ) ) ;
#30269 = CARTESIAN_POINT ( 'NONE',  ( 18.70312500061451644, -4.541064518000417216, -2.621784821875001281 ) ) ;
#30270 = CARTESIAN_POINT ( 'NONE',  ( 4.865625000614517859, 3.027376345333613106, -5.243569643749998122 ) ) ;
#30271 = CARTESIAN_POINT ( 'NONE',  ( 19.05937500061451928, 0.000000000000000000, 5.243569643749999010 ) ) ;
#30272 = CARTESIAN_POINT ( 'NONE',  ( 3.487500000000000711, -2.886751345948129988, 4.999999999999997335 ) ) ;
#30273 = CARTESIAN_POINT ( 'NONE',  ( 6.440625000614517148, -3.027376345333614438, 5.243569643749998122 ) ) ;
#30274 = CARTESIAN_POINT ( 'NONE',  ( 20.69062500061451715, 6.054752690667223547, 3.707466751127219781E-16 ) ) ;
#30275 = EDGE_CURVE ( 'NONE', #6226, #65099, #36467, .T. ) ;
#30276 = CARTESIAN_POINT ( 'NONE',  ( -4.243569643749997233, 14.44062500061451715, 32.45002607614398471 ) ) ;
#30277 = CARTESIAN_POINT ( 'NONE',  ( 19.76250000122903216, 0.000000000000000000, 4.999999999999998224 ) ) ;
#30278 = CARTESIAN_POINT ( 'NONE',  ( 13.39687500061451608, -2.746126346562641984, -4.756430356249999214 ) ) ;
#30279 = CARTESIAN_POINT ( 'NONE',  ( 9.028125000614517504, 4.541064518000418104, 2.621784821874999949 ) ) ;
#30280 = CARTESIAN_POINT ( 'NONE',  ( 3.871875000614519280, -6.054752690667223547, -1.112240025338166033E-15 ) ) ;
#30281 = CARTESIAN_POINT ( 'NONE',  ( 29.54062500061451502, -3.027376345333610441, -5.243569643749999898 ) ) ;
#30282 = CARTESIAN_POINT ( 'NONE',  ( 22.54687500061451999, 6.054752690667223547, 3.707466751127219781E-16 ) ) ;
#30283 = CARTESIAN_POINT ( 'NONE',  ( 15.36562500061451608, 3.027376345333611329, 5.243569643749999010 ) ) ;
#30284 = CARTESIAN_POINT ( 'NONE',  ( 24.00000000122902932, -2.886751345948125991, -5.000000000000000000 ) ) ;
#30285 = ADVANCED_BREP_SHAPE_REPRESENTATION ( '', ( #20659, #23765 ), #24934 ) ;
#30286 = CARTESIAN_POINT ( 'NONE',  ( 24.51562500061451289, -6.054752690667223547, -1.112240025338166033E-15 ) ) ;
#30287 = CARTESIAN_POINT ( 'NONE',  ( 19.05937500061451928, 0.000000000000000000, 5.243569643749999010 ) ) ;
#30288 = CARTESIAN_POINT ( 'NONE',  ( 15.59062500061451573, -3.027376345333610441, -5.243569643749999898 ) ) ;
#30289 = CARTESIAN_POINT ( 'NONE',  ( -2.121784821874999949, 16.63437500061451857, 26.32496088578401938 ) ) ;
#30290 = CARTESIAN_POINT ( 'NONE',  ( 20.80312500061451431, 0.000000000000000000, 5.243569643749999010 ) ) ;
#30291 = LINE ( 'NONE', #56904, #59739 ) ;
#30292 = ORIENTED_EDGE ( 'NONE', *, *, #17585, .F. ) ;
#30293 = CARTESIAN_POINT ( 'NONE',  ( 24.71250000000000213, -5.773502691896255534, -1.060575238724906372E-15 ) ) ;
#30294 = CARTESIAN_POINT ( 'NONE',  ( -1.999999999999997113, 10.17500000000000249, -26.53589838486224295 ) ) ;
#30295 = CARTESIAN_POINT ( 'NONE',  ( -7.967954043666661671E-16, 19.84062499938548285, 34.33755215474603517 ) ) ;
#30296 = CARTESIAN_POINT ( 'NONE',  ( 25.71562500061451573, 3.027376345333611329, 5.243569643749999010 ) ) ;
#30297 = CARTESIAN_POINT ( 'NONE',  ( 6.628125000614517148, 6.421520780324663323E-16, -5.243569643749999010 ) ) ;
#30298 = CARTESIAN_POINT ( 'NONE',  ( 18.63750000122903216, 6.123233995736764310E-16, -4.999999999999998224 ) ) ;
#30299 =( BOUNDED_CURVE ( )  B_SPLINE_CURVE ( 2, ( #32089, #64968, #9555, #26925, #71984, #54261, #65330 ),
 .UNSPECIFIED., .F., .F. ) 
 B_SPLINE_CURVE_WITH_KNOTS ( ( 3, 2, 2, 3 ),
 ( 0.7199999999999999734, 0.7233333333333333837, 0.7266666666666666829, 0.7299999999999999822 ),
 .UNSPECIFIED. ) 
 CURVE ( )  GEOMETRIC_REPRESENTATION_ITEM ( )  RATIONAL_B_SPLINE_CURVE ( ( 1.000000000000000000, 0.8660254037844387076, 1.000000000000000000, 0.8660254037844387076, 1.000000000000000000, 0.8660254037844387076, 1.000000000000000000 ) ) 
 REPRESENTATION_ITEM ( '' )  );
#30300 = CARTESIAN_POINT ( 'NONE',  ( 24.59062500061451573, -3.027376345333610441, -5.243569643749999898 ) ) ;
#30301 = CARTESIAN_POINT ( 'NONE',  ( 26.43750000000000000, -2.886751345948129988, 4.999999999999997335 ) ) ;
#30302 = CARTESIAN_POINT ( 'NONE',  ( -2.828200636599751609E-16, 15.05000000122903536, -34.61880215351700230 ) ) ;
#30303 = FACE_OUTER_BOUND ( 'NONE', #38018, .T. ) ;
#30304 = CARTESIAN_POINT ( 'NONE',  ( 10.75312500061451715, 4.541064518000418104, -2.621784821874998173 ) ) ;
#30305 = VERTEX_POINT ( 'NONE', #9127 ) ;
#30306 = CARTESIAN_POINT ( 'NONE',  ( 26.01562500061451289, 3.027376345333613106, -5.243569643749998122 ) ) ;
#30307 = CARTESIAN_POINT ( 'NONE',  ( 8.465625000614515727, 3.027376345333613106, -5.243569643749998122 ) ) ;
#30308 = AXIS2_PLACEMENT_3D ( 'NONE', #47565, #30932, #53473 ) ;
#30309 = CARTESIAN_POINT ( 'NONE',  ( 14.74687500061451573, -2.746126346562642428, -4.756430356249999214 ) ) ;
#30310 = CARTESIAN_POINT ( 'NONE',  ( 13.12500000000000178, 6.123233995736764310E-16, -4.999999999999998224 ) ) ;
#30311 = ADVANCED_FACE ( 'NONE', ( #58985 ), #31663, .F. ) ;
#30312 = CARTESIAN_POINT ( 'NONE',  ( 13.46249999999999858, -5.773502691896255534, -1.060575238724906372E-15 ) ) ;
#30313 = EDGE_CURVE ( 'NONE', #2494, #38561, #37214, .T. ) ;
#30314 =( BOUNDED_CURVE ( )  B_SPLINE_CURVE ( 2, ( #57906, #35024, #7315, #29845, #69385, #1424, #35383, #68295, #23573 ),
 .UNSPECIFIED., .F., .F. ) 
 B_SPLINE_CURVE_WITH_KNOTS ( ( 3, 2, 2, 2, 3 ),
 ( 0.2083333333333333426, 0.2129629629629629650, 0.2222222222222222099, 0.2314814814814814825, 0.2361111111111111049 ),
 .UNSPECIFIED. ) 
 CURVE ( )  GEOMETRIC_REPRESENTATION_ITEM ( )  RATIONAL_B_SPLINE_CURVE ( ( 0.9330127018922194093, 0.9330127018922195203, 1.000000000000000000, 0.8660254037844387076, 1.000000000000000000, 0.8660254037844387076, 1.000000000000000000, 0.9330127018922194093, 0.9330127018922194093 ) ) 
 REPRESENTATION_ITEM ( '' )  );
#30315 = CARTESIAN_POINT ( 'NONE',  ( 14.29687500061451821, -3.027376345333610441, -5.243569643749999898 ) ) ;
#30316 = CARTESIAN_POINT ( 'NONE',  ( 8.400000001229035007, 5.773502691896255534, 3.535250795749688894E-16 ) ) ;
#30317 = CARTESIAN_POINT ( 'NONE',  ( 18.08437500061451431, 4.541064518000418104, 2.621784821874999949 ) ) ;
#30318 = CARTESIAN_POINT ( 'NONE',  ( 16.87500000000000000, 4.330127018922191873, 2.499999999999999556 ) ) ;
#30319 = CARTESIAN_POINT ( 'NONE',  ( 7.921875000614517326, -6.054752690667223547, -1.112240025338166033E-15 ) ) ;
#30320 = CARTESIAN_POINT ( 'NONE',  ( 9.001249775931846008E-16, 11.36562500061451786, -25.09994784771203058 ) ) ;
#30321 = CARTESIAN_POINT ( 'NONE',  ( 24.60000000000000142, 0.000000000000000000, 4.999999999999998224 ) ) ;
#30322 = CARTESIAN_POINT ( 'NONE',  ( 22.35937500061451644, 2.746126346562645981, -4.756430356249997438 ) ) ;
#30323 = CYLINDRICAL_SURFACE ( 'NONE', #46578, 4.999999999999998224 ) ;
#30324 = CARTESIAN_POINT ( 'NONE',  ( 25.41562500061451146, -6.054752690667223547, -1.112240025338166033E-15 ) ) ;
#30325 = CARTESIAN_POINT ( 'NONE',  ( 21.11250000122903359, 0.000000000000000000, 4.999999999999998224 ) ) ;
#30326 = CARTESIAN_POINT ( 'NONE',  ( 26.10937500061451644, 4.541064518000418104, -2.621784821874998173 ) ) ;
#30327 = CARTESIAN_POINT ( 'NONE',  ( 29.33437500061451431, 4.541064518000418104, 2.621784821874999949 ) ) ;
#30328 = CARTESIAN_POINT ( 'NONE',  ( 22.19999999999999574, 4.330127018922192761, -2.499999999999997780 ) ) ;
#30329 = CARTESIAN_POINT ( 'NONE',  ( 6.215625000614517504, 3.027376345333613106, -5.243569643749998122 ) ) ;
#30330 = B_SPLINE_CURVE_WITH_KNOTS ( 'NONE', 3,
 ( #9731, #49630, #4568, #4928, #27098, #44463, #48897, #37801, #61067, #65882 ),
 .UNSPECIFIED., .F., .F.,
 ( 4, 3, 3, 4 ),
 ( 4.336808689942017255E-19, 0.0001572269111698576115, 0.0003144536816620901835, 0.0005496948180016699662 ),
 .UNSPECIFIED. ) ;
#30331 = CARTESIAN_POINT ( 'NONE',  ( 22.02187500061451431, 4.119189519843966529, 2.378215178124999607 ) ) ;
#30332 =( BOUNDED_CURVE ( )  B_SPLINE_CURVE ( 1, ( #12861, #40958 ),
 .UNSPECIFIED., .F., .F. ) 
 B_SPLINE_CURVE_WITH_KNOTS ( ( 2, 2 ),
 ( 0.000000000000000000, 1.000000000000000000 ),
 .UNSPECIFIED. ) 
 CURVE ( )  GEOMETRIC_REPRESENTATION_ITEM ( )  RATIONAL_B_SPLINE_CURVE ( ( 0.9401540970596797830, 0.9401540970596797830 ) ) 
 REPRESENTATION_ITEM ( '' )  );
#30333 = CARTESIAN_POINT ( 'NONE',  ( 16.17187500061451644, 3.027376345333613106, -5.243569643749998122 ) ) ;
#30334 = CARTESIAN_POINT ( 'NONE',  ( 9.009375000614515017, 2.746126346562643317, 4.756430356249998326 ) ) ;
#30335 = CARTESIAN_POINT ( 'NONE',  ( 3.890625000614517326, -3.027376345333610441, -5.243569643749999898 ) ) ;
#30336 = CARTESIAN_POINT ( 'NONE',  ( 7.284375000614518036, 4.541064518000418104, 2.621784821874999949 ) ) ;
#30337 = CARTESIAN_POINT ( 'NONE',  ( 18.00937500061451502, 4.541064518000418104, -2.621784821874998173 ) ) ;
#30338 = CARTESIAN_POINT ( 'NONE',  ( -0.2655188809381071047, 25.54316770519904267, 26.00000000000000355 ) ) ;
#30339 = CARTESIAN_POINT ( 'NONE',  ( 27.37500000000000000, -4.330127018922194537, 2.499999999999995559 ) ) ;
#30340 = CARTESIAN_POINT ( 'NONE',  ( 28.17187500061451644, -6.054752690667223547, -1.112240025338166033E-15 ) ) ;
#30341 = CARTESIAN_POINT ( 'NONE',  ( 26.45625000122903003, 0.000000000000000000, 4.999999999999998224 ) ) ;
#30342 = CARTESIAN_POINT ( 'NONE',  ( 3.328125000614516438, -4.541064518000419881, 2.621784821874995952 ) ) ;
#30343 = ORIENTED_EDGE ( 'NONE', *, *, #69330, .F. ) ;
#30344 = CARTESIAN_POINT ( 'NONE',  ( 11.58750000000000036, -2.886751345948129988, 4.999999999999997335 ) ) ;
#30345 = CARTESIAN_POINT ( 'NONE',  ( 11.59687500061451537, 4.119189519843966529, -2.378215178124998275 ) ) ;
#30346 = CARTESIAN_POINT ( 'NONE',  ( 21.06562500061451715, 3.027376345333613106, -5.243569643749998122 ) ) ;
#30347 = CARTESIAN_POINT ( 'NONE',  ( 12.03749999999999964, -2.886751345948129988, 4.999999999999997335 ) ) ;
#30348 = CARTESIAN_POINT ( 'NONE',  ( 8.362500001229031810, 4.330127018922192761, -2.499999999999997780 ) ) ;
#30349 = CARTESIAN_POINT ( 'NONE',  ( 5.653125000614517504, -4.541064518000417216, -2.621784821875001281 ) ) ;
#30350 = CARTESIAN_POINT ( 'NONE',  ( 20.85000000000000142, 4.330127018922192761, -2.499999999999997780 ) ) ;
#30351 = CARTESIAN_POINT ( 'NONE',  ( 21.74062500061451431, -3.027376345333614438, 5.243569643749998122 ) ) ;
#30352 = CARTESIAN_POINT ( 'NONE',  ( 24.41250000122903430, -4.330127018922190985, -2.500000000000001332 ) ) ;
#30353 = CARTESIAN_POINT ( 'NONE',  ( 3.756430356250000102, 20.29062499938548569, 30.00000000000000000 ) ) ;
#30354 = CARTESIAN_POINT ( 'NONE',  ( 5.924999999999999822, 6.123233995736764310E-16, -4.999999999999998224 ) ) ;
#30355 = ORIENTED_EDGE ( 'NONE', *, *, #336, .T. ) ;
#30356 = CARTESIAN_POINT ( 'NONE',  ( 18.44062500061451715, 6.054752690667223547, 3.707466751127219781E-16 ) ) ;
#30357 = CARTESIAN_POINT ( 'NONE',  ( 27.02812500061451573, 4.541064518000418104, 2.621784821874999949 ) ) ;
#30358 = CARTESIAN_POINT ( 'NONE',  ( 26.44687500061451502, -3.027376345333610441, -5.243569643749999898 ) ) ;
#30359 = CARTESIAN_POINT ( 'NONE',  ( 14.95312500061451644, 0.000000000000000000, 5.243569643749999010 ) ) ;
#30360 = CARTESIAN_POINT ( 'NONE',  ( 29.46562500061451573, -6.054752690667223547, -1.112240025338166033E-15 ) ) ;
#30361 = CARTESIAN_POINT ( 'NONE',  ( 9.703125000614514661, -4.541064518000417216, -2.621784821875001281 ) ) ;
#30362 = CARTESIAN_POINT ( 'NONE',  ( 30.00000000000000000, 0.000000000000000000, 4.999999999999998224 ) ) ;
#30363 = AXIS2_PLACEMENT_3D ( 'NONE', #17854, #40060, #51137 ) ;
#30364 = CARTESIAN_POINT ( 'NONE',  ( 27.26250000122903216, 4.330127018922192761, -2.499999999999997780 ) ) ;
#30365 = CARTESIAN_POINT ( 'NONE',  ( 18.38437500061451857, 5.824947211148865298E-16, -4.756430356249998326 ) ) ;
#30366 = CARTESIAN_POINT ( 'NONE',  ( 17.57812500061451644, 4.541064518000418104, 2.621784821874999949 ) ) ;
#30367 = CARTESIAN_POINT ( 'NONE',  ( -1.243387493232115393E-14, 15.31250000000000000, 26.00000000000000000 ) ) ;
#30368 = CARTESIAN_POINT ( 'NONE',  ( 28.99687500061451573, -3.027376345333614438, 5.243569643749998122 ) ) ;
#30369 = CARTESIAN_POINT ( 'NONE',  ( 11.52187500061451608, -6.054752690667223547, -1.112240025338166033E-15 ) ) ;
#30370 = CARTESIAN_POINT ( 'NONE',  ( 10.65937500061451715, -4.541064518000417216, -2.621784821875001281 ) ) ;
#30371 = CARTESIAN_POINT ( 'NONE',  ( 18.72187500061451360, -6.054752690667223547, -1.112240025338166033E-15 ) ) ;
#30372 = ORIENTED_EDGE ( 'NONE', *, *, #6970, .T. ) ;
#30373 = CARTESIAN_POINT ( 'NONE',  ( 3.046343057529203424, 3.964819538874875704, 3.046343057529141696 ) ) ;
#30374 = CARTESIAN_POINT ( 'NONE',  ( 22.22812500061451502, -4.541064518000419881, 2.621784821874995952 ) ) ;
#30375 = CARTESIAN_POINT ( 'NONE',  ( 16.50937500061451502, -4.541064518000417216, -2.621784821875001281 ) ) ;
#30376 = CARTESIAN_POINT ( 'NONE',  ( 21.62812500061451360, 4.541064518000418104, 2.621784821874999949 ) ) ;
#30377 = CARTESIAN_POINT ( 'NONE',  ( 8.484601909799253346E-16, 14.26250000000000107, 34.61880215351700230 ) ) ;
#30378 = CARTESIAN_POINT ( 'NONE',  ( 3.046875000614519990, -3.027376345333610441, -5.243569643749999898 ) ) ;
#30379 = CARTESIAN_POINT ( 'NONE',  ( 9.000000001229034652, -2.886751345948129988, 4.999999999999997335 ) ) ;
#30380 = ORIENTED_EDGE ( 'NONE', *, *, #45595, .T. ) ;
#30381 = CARTESIAN_POINT ( 'NONE',  ( 4.275000001229035895, 2.886751345948129099, -4.999999999999998224 ) ) ;
#30382 = CARTESIAN_POINT ( 'NONE',  ( 3.999999999999999112, 18.42500000000000071, -30.00000000000000000 ) ) ;
#30383 = CARTESIAN_POINT ( 'NONE',  ( 25.01250000122903216, 4.330127018922192761, -2.499999999999997780 ) ) ;
#30384 = CARTESIAN_POINT ( 'NONE',  ( -3.756430356250001434, 13.46562499938548285, 32.16877607737301048 ) ) ;
#30385 = CARTESIAN_POINT ( 'NONE',  ( 9.046875000614518214, 6.054752690667223547, 3.707466751127219781E-16 ) ) ;
#30386 = CARTESIAN_POINT ( 'NONE',  ( 65.00000000000000000, -7.332543590861121174, -5.218601775200084170 ) ) ;
#30387 = CARTESIAN_POINT ( 'NONE',  ( 16.00312500061451715, -4.541064518000417216, -2.621784821875001281 ) ) ;
#30388 = CARTESIAN_POINT ( 'NONE',  ( 10.50937500061451679, 0.000000000000000000, 5.243569643749999010 ) ) ;
#30389 = CARTESIAN_POINT ( 'NONE',  ( 2.990625000614519191, -3.027376345333610441, -5.243569643749999898 ) ) ;
#30390 = CARTESIAN_POINT ( 'NONE',  ( 18.23437500061451999, -4.541064518000419881, 2.621784821874995952 ) ) ;
#30391 = CARTESIAN_POINT ( 'NONE',  ( 7.396875000614519635, -3.027376345333614438, 5.243569643749998122 ) ) ;
#30392 = CARTESIAN_POINT ( 'NONE',  ( 1.999999999999998668, 17.60000000000000142, -33.46410161513775705 ) ) ;
#30393 = CARTESIAN_POINT ( 'NONE',  ( 8.690625000614515372, -3.027376345333614438, 5.243569643749998122 ) ) ;
#30394 = CARTESIAN_POINT ( 'NONE',  ( 18.77812500061451573, 6.421520780324663323E-16, -5.243569643749999010 ) ) ;
#30395 = VERTEX_POINT ( 'NONE', #605 ) ;
#30396 = EDGE_CURVE ( 'NONE', #4240, #67801, #44348, .T. ) ;
#30397 = CARTESIAN_POINT ( 'NONE',  ( 14.87812500061451537, 4.541064518000418104, 2.621784821874999949 ) ) ;
#30398 = CARTESIAN_POINT ( 'NONE',  ( 10.86562500061451431, 3.027376345333611329, 5.243569643749999010 ) ) ;
#30399 = CARTESIAN_POINT ( 'NONE',  ( 22.80937500061451573, -4.119189519843965641, -2.378215178125001383 ) ) ;
#30400 = CARTESIAN_POINT ( 'NONE',  ( 12.07499999999999929, -4.330127018922194537, 2.499999999999995559 ) ) ;
#30401 = CARTESIAN_POINT ( 'NONE',  ( 6.300000001229033586, -2.886751345948129988, 4.999999999999997335 ) ) ;
#30402 = EDGE_CURVE ( 'NONE', #71147, #39806, #61916, .T. ) ;
#30403 = CARTESIAN_POINT ( 'NONE',  ( 13.95937500061451786, 4.541064518000418104, -2.621784821874998173 ) ) ;
#30404 = CARTESIAN_POINT ( 'NONE',  ( 16.76250000122903216, -4.330127018922190985, -2.500000000000001332 ) ) ;
#30405 = CARTESIAN_POINT ( 'NONE',  ( 25.27499999999999858, 6.123233995736764310E-16, -4.999999999999998224 ) ) ;
#30406 = CARTESIAN_POINT ( 'NONE',  ( 9.001249775931846008E-16, 18.56562500061451715, -25.09994784771203058 ) ) ;
#30407 = CARTESIAN_POINT ( 'NONE',  ( 16.16250000122903430, 0.000000000000000000, 4.999999999999998224 ) ) ;
#30408 = CARTESIAN_POINT ( 'NONE',  ( -1.487416814333745711E-14, 14.82500000122903572, -26.00000000000000000 ) ) ;
#30409 = VECTOR ( 'NONE', #50814, 1000.000000000000000 ) ;
#30410 = CARTESIAN_POINT ( 'NONE',  ( 9.525000001229035007, -5.773502691896255534, -1.060575238724906372E-15 ) ) ;
#30411 = CARTESIAN_POINT ( 'NONE',  ( 1.071796769724476572, 14.39509619066136636, 34.00000000000000000 ) ) ;
#30412 = CARTESIAN_POINT ( 'NONE',  ( 18.98437500061451644, 4.541064518000418104, 2.621784821874999949 ) ) ;
#30413 = ADVANCED_FACE ( 'NONE', ( #60816 ), #56731, .F. ) ;
#30414 = CARTESIAN_POINT ( 'NONE',  ( 29.88749999999999929, 5.773502691896255534, 3.535250795749688894E-16 ) ) ;
#30415 = CARTESIAN_POINT ( 'NONE',  ( 13.94062500061451892, 6.054752690667223547, 3.707466751127219781E-16 ) ) ;
#30416 = CARTESIAN_POINT ( 'NONE',  ( 10.40625000122903288, -4.330127018922190985, -2.500000000000001332 ) ) ;
#30417 = CARTESIAN_POINT ( 'NONE',  ( 22.99687500061451573, 6.054752690667223547, 3.707466751127219781E-16 ) ) ;
#30418 = CARTESIAN_POINT ( 'NONE',  ( 16.28437500061451715, -2.746126346562646425, 4.756430356249996549 ) ) ;
#30419 = CARTESIAN_POINT ( 'NONE',  ( 9.440625000614517148, 6.054752690667223547, 3.707466751127219781E-16 ) ) ;
#30420 = CARTESIAN_POINT ( 'NONE',  ( 16.50937500061451502, -4.541064518000417216, -2.621784821875001281 ) ) ;
#30421 = EDGE_LOOP ( 'NONE', ( #63254, #49792, #29183, #25982 ) ) ;
#30422 = CARTESIAN_POINT ( 'NONE',  ( 26.63437500061451857, 4.541064518000418104, 2.621784821874999949 ) ) ;
#30423 = CARTESIAN_POINT ( 'NONE',  ( 28.41562500061451502, 3.027376345333611329, 5.243569643749999010 ) ) ;
#30424 = CARTESIAN_POINT ( 'NONE',  ( 16.82812500061451644, -4.541064518000419881, 2.621784821874995952 ) ) ;
#30425 = CARTESIAN_POINT ( 'NONE',  ( 18.78749999999999787, -2.886751345948096681, 5.000000000000054179 ) ) ;
#30426 = DIRECTION ( 'NONE',  ( -1.000000000000000000, -0.000000000000000000, -0.000000000000000000 ) ) ;
#30427 = CARTESIAN_POINT ( 'NONE',  ( 9.825000000000001066, -4.330127018922194537, 2.499999999999995559 ) ) ;
#30428 = CARTESIAN_POINT ( 'NONE',  ( 19.95000000122903572, -2.886751345948125991, -5.000000000000000000 ) ) ;
#30429 = CARTESIAN_POINT ( 'NONE',  ( -6.275039685470489619E-15, 17.97500000122903074, -26.00000000000000355 ) ) ;
#30430 = CARTESIAN_POINT ( 'NONE',  ( 11.48437500061451821, -2.746126346562642428, -4.756430356249999214 ) ) ;
#30431 = ORIENTED_EDGE ( 'NONE', *, *, #47837, .T. ) ;
#30432 = CARTESIAN_POINT ( 'NONE',  ( 18.14999999999999858, 4.330127018922192761, -2.499999999999997780 ) ) ;
#30433 = CARTESIAN_POINT ( 'NONE',  ( 19.23749999999999716, -2.886751345948129988, 4.999999999999997335 ) ) ;
#30434 = CARTESIAN_POINT ( 'NONE',  ( 18.23437500061451999, -4.541064518000419881, 2.621784821874995952 ) ) ;
#30435 = CARTESIAN_POINT ( 'NONE',  ( 13.86562500061451431, 3.027376345333613106, -5.243569643749998122 ) ) ;
#30436 = ORIENTED_EDGE ( 'NONE', *, *, #30396, .F. ) ;
#30437 = CARTESIAN_POINT ( 'NONE',  ( 5.000000000000000000, 39.99999999999999289, 45.00000000000000000 ) ) ;
#30438 = CARTESIAN_POINT ( 'NONE',  ( 7.040625000614517681, -3.027376345333610441, -5.243569643749999898 ) ) ;
#30439 = CARTESIAN_POINT ( 'NONE',  ( 10.38750000000000107, -2.886751345948126435, -5.000000000000000000 ) ) ;
#30440 = CARTESIAN_POINT ( 'NONE',  ( 12.71250000000000036, 2.886751345948129099, -4.999999999999998224 ) ) ;
#30441 = CARTESIAN_POINT ( 'NONE',  ( 28.05937500061451217, -5.492252693125287522, -1.008910452111647106E-15 ) ) ;
#30442 = CARTESIAN_POINT ( 'NONE',  ( -2.121784821874996840, 14.92812500061451608, 33.67503911421598417 ) ) ;
#30443 = CARTESIAN_POINT ( 'NONE',  ( 27.51562500061451644, 3.027376345333611329, 5.243569643749999010 ) ) ;
#30444 = CARTESIAN_POINT ( 'NONE',  ( 8.099999999999999645, -4.330127018922190985, -2.500000000000001332 ) ) ;
#30445 = CARTESIAN_POINT ( 'NONE',  ( -1.878215178124999163, 18.19062499938548427, 26.74683588394047007 ) ) ;
#30446 = CARTESIAN_POINT ( 'NONE',  ( 23.25937500061451857, -4.541064518000417216, -2.621784821875001281 ) ) ;
#30447 = EDGE_LOOP ( 'NONE', ( #20095, #42840, #2720, #42111 ) ) ;
#30448 = CARTESIAN_POINT ( 'NONE',  ( 20.95312500061451999, -4.541064518000417216, -2.621784821875001281 ) ) ;
#30449 = CARTESIAN_POINT ( 'NONE',  ( 22.92187500061451644, 3.027376345333613106, -5.243569643749998122 ) ) ;
#30450 = CARTESIAN_POINT ( 'NONE',  ( 4.243569643749999898, 15.52812500061459389, -30.00000000000000000 ) ) ;
#30451 = CARTESIAN_POINT ( 'NONE',  ( 6.665625000614515905, 3.027376345333613106, -5.243569643749998122 ) ) ;
#30452 = CARTESIAN_POINT ( 'NONE',  ( 26.85937500061451644, -4.119189519843965641, -2.378215178125001383 ) ) ;
#30453 = CARTESIAN_POINT ( 'NONE',  ( 24.32812500061451289, 4.541064518000418104, 2.621784821874999949 ) ) ;
#30454 = CARTESIAN_POINT ( 'NONE',  ( 10.32187500061451679, 2.746126346562645981, -4.756430356249997438 ) ) ;
#30455 = CARTESIAN_POINT ( 'NONE',  ( 1.878215178125000495, 17.21562499938548285, 26.74683588394047007 ) ) ;
#30456 = CARTESIAN_POINT ( 'NONE',  ( 17.44687500061451857, -3.027376345333610441, -5.243569643749999898 ) ) ;
#30457 = CARTESIAN_POINT ( 'NONE',  ( 24.27187500061452141, 3.027376345333613106, -5.243569643749998122 ) ) ;
#30458 = CARTESIAN_POINT ( 'NONE',  ( -4.243569643749999898, 14.45937500061451964, 30.00000000000000000 ) ) ;
#30459 = CARTESIAN_POINT ( 'NONE',  ( 6.703125000614516438, 4.541064518000418104, -2.621784821874998173 ) ) ;
#30460 = CARTESIAN_POINT ( 'NONE',  ( 29.46562500061451573, -6.054752690667223547, -1.112240025338166033E-15 ) ) ;
#30461 = CARTESIAN_POINT ( 'NONE',  ( 3.346875000614518036, -3.027376345333614438, 5.243569643749998122 ) ) ;
#30462 = CARTESIAN_POINT ( 'NONE',  ( -3.999999999999999112, 14.93750000000000355, 27.69059892324149530 ) ) ;
#30463 = CARTESIAN_POINT ( 'NONE',  ( 4.715625000614516615, -6.054752690667223547, -1.112240025338166033E-15 ) ) ;
#30464 = CARTESIAN_POINT ( 'NONE',  ( 8.859375000614518214, -4.541064518000417216, -2.621784821875001281 ) ) ;
#30465 = SURFACE_SIDE_STYLE ('',( #18633 ) ) ;
#30466 = CARTESIAN_POINT ( 'NONE',  ( 16.98750000122903359, 4.330127018922191873, 2.499999999999999556 ) ) ;
#30467 = CARTESIAN_POINT ( 'NONE',  ( 2.859375000614519546, 0.000000000000000000, 5.243569643749999010 ) ) ;
#30468 = CARTESIAN_POINT ( 'NONE',  ( 5.465625000614517504, 3.027376345333611329, 5.243569643749999010 ) ) ;
#30469 = CYLINDRICAL_SURFACE ( 'NONE', #68202, 4.000000000000000000 ) ;
#30470 = CARTESIAN_POINT ( 'NONE',  ( 21.80625000122903145, 4.330127018922192761, -2.499999999999997780 ) ) ;
#30471 = CARTESIAN_POINT ( 'NONE',  ( 17.03437500061451715, 6.421520780324663323E-16, -5.243569643749999010 ) ) ;
#30472 = CARTESIAN_POINT ( 'NONE',  ( 1.999999999999997335, 19.11874999877096570, 33.46410161513775705 ) ) ;
#30473 = ORIENTED_EDGE ( 'NONE', *, *, #53326, .F. ) ;
#30474 = CARTESIAN_POINT ( 'NONE',  ( 22.75312500061451360, -4.541064518000417216, -2.621784821875001281 ) ) ;
#30475 = CARTESIAN_POINT ( 'NONE',  ( 9.553125000614517859, 0.000000000000000000, 5.243569643749999010 ) ) ;
#30476 = CARTESIAN_POINT ( 'NONE',  ( 25.84687500061451715, -3.027376345333614438, 5.243569643749998122 ) ) ;
#30477 = CARTESIAN_POINT ( 'NONE',  ( 10.67812500061451608, 6.421520780324663323E-16, -5.243569643749999010 ) ) ;
#30478 = CARTESIAN_POINT ( 'NONE',  ( 20.36249999999999716, 2.886751345948095793, -5.000000000000055067 ) ) ;
#30479 =( BOUNDED_CURVE ( )  B_SPLINE_CURVE ( 3, ( #23908, #22817, #307, #46095 ),
 .UNSPECIFIED., .F., .F. ) 
 B_SPLINE_CURVE_WITH_KNOTS ( ( 4, 4 ),
 ( 1.570796326794896558, 3.141592653589793116 ),
 .UNSPECIFIED. ) 
 CURVE ( )  GEOMETRIC_REPRESENTATION_ITEM ( )  RATIONAL_B_SPLINE_CURVE ( ( 1.000000000000000000, 0.8047378541243649375, 0.8047378541243649375, 1.000000000000000000 ) ) 
 REPRESENTATION_ITEM ( '' )  );
#30480 = CARTESIAN_POINT ( 'NONE',  ( 9.412500001229034297, 0.000000000000000000, 4.999999999999998224 ) ) ;
#30481 = CARTESIAN_POINT ( 'NONE',  ( 25.49062500061451786, -3.027376345333610441, -5.243569643749999898 ) ) ;
#30482 = CARTESIAN_POINT ( 'NONE',  ( 2.121784821874999061, 10.65312500061451750, -33.67503911421598417 ) ) ;
#30483 = CARTESIAN_POINT ( 'NONE',  ( 12.11250000122903181, 0.000000000000000000, 4.999999999999998224 ) ) ;
#30484 = CARTESIAN_POINT ( 'NONE',  ( 22.49062500061451431, 6.054752690667223547, 3.707466751127219781E-16 ) ) ;
#30485 = CARTESIAN_POINT ( 'NONE',  ( 17.57812500061451644, 4.541064518000418104, 2.621784821874999949 ) ) ;
#30486 = CARTESIAN_POINT ( 'NONE',  ( 6.534375000614517148, -4.541064518000419881, 2.621784821874995952 ) ) ;
#30487 = EDGE_CURVE ( 'NONE', #29484, #48852, #59415, .T. ) ;
#30488 = CARTESIAN_POINT ( 'NONE',  ( 18.11250000000000071, 2.886751345948129099, -4.999999999999998224 ) ) ;
#30489 = CARTESIAN_POINT ( 'NONE',  ( 12.86250000122903359, 4.330127018922192761, -2.499999999999997780 ) ) ;
#30490 = CARTESIAN_POINT ( 'NONE',  ( 9.890625000614516438, 6.054752690667223547, 3.707466751127219781E-16 ) ) ;
#30491 = CARTESIAN_POINT ( 'NONE',  ( 13.34062500061451750, -3.027376345333610441, -5.243569643749999898 ) ) ;
#30492 = CARTESIAN_POINT ( 'NONE',  ( 24.11250000122903359, 4.330127018922192761, -2.499999999999997780 ) ) ;
#30493 = CARTESIAN_POINT ( 'NONE',  ( 20.82187500061451857, 3.027376345333611329, 5.243569643749999010 ) ) ;
#30494 = CARTESIAN_POINT ( 'NONE',  ( 21.45937500061451786, -4.541064518000417216, -2.621784821875001281 ) ) ;
#30495 = CARTESIAN_POINT ( 'NONE',  ( 30.00000000000000000, 0.000000000000000000, 4.999999999999998224 ) ) ;
#30496 = CARTESIAN_POINT ( 'NONE',  ( 8.362500001229031810, 4.330127018922192761, -2.499999999999997780 ) ) ;
#30497 = CARTESIAN_POINT ( 'NONE',  ( 6.984375000614516438, -4.541064518000419881, 2.621784821874995952 ) ) ;
#30498 = CARTESIAN_POINT ( 'NONE',  ( 25.47187500061451715, -6.054752690667223547, -1.112240025338166033E-15 ) ) ;
#30499 = CARTESIAN_POINT ( 'NONE',  ( 4.584099534023079237, 1.997112472210624379, -4.621249760862988332 ) ) ;
#30500 = CARTESIAN_POINT ( 'NONE',  ( 20.76562500061451644, 3.027376345333611329, 5.243569643749999010 ) ) ;
#30501 = CARTESIAN_POINT ( 'NONE',  ( 27.72187500061451715, -6.054752690667223547, -1.112240025338166033E-15 ) ) ;
#30502 = CARTESIAN_POINT ( 'NONE',  ( 2.655984681222220721E-16, 16.91562499938548214, 25.66244784525396483 ) ) ;
#30503 = CARTESIAN_POINT ( 'NONE',  ( 7.950000000000001954, 0.000000000000000000, 4.999999999999998224 ) ) ;
#30504 = LINE ( 'NONE', #42683, #34807 ) ;
#30505 = CARTESIAN_POINT ( 'NONE',  ( 6.571875000614517681, -6.054752690667223547, -1.112240025338166033E-15 ) ) ;
#30506 = CARTESIAN_POINT ( 'NONE',  ( 16.75312500061451715, 0.000000000000000000, 5.243569643749999010 ) ) ;
#30507 = VERTEX_POINT ( 'NONE', #40491 ) ;
#30508 = CARTESIAN_POINT ( 'NONE',  ( 22.98750000000000071, -2.886751345948092684, -5.000000000000057732 ) ) ;
#30509 = CARTESIAN_POINT ( 'NONE',  ( 25.22812500061451502, 4.541064518000418104, 2.621784821874999949 ) ) ;
#30510 = CARTESIAN_POINT ( 'NONE',  ( 4.209375000614516971, 0.000000000000000000, 5.243569643749999010 ) ) ;
#30511 = CARTESIAN_POINT ( 'NONE',  ( 10.31250000122903288, 0.000000000000000000, 4.999999999999998224 ) ) ;
#30512 = LINE ( 'NONE', #64116, #53656 ) ;
#30513 = CARTESIAN_POINT ( 'NONE',  ( 17.10000000000000142, -4.330127018922190985, -2.500000000000001332 ) ) ;
#30514 = CARTESIAN_POINT ( 'NONE',  ( 20.16562500061451146, 3.027376345333613106, -5.243569643749998122 ) ) ;
#30515 = ORIENTED_EDGE ( 'NONE', *, *, #10064, .F. ) ;
#30516 = CARTESIAN_POINT ( 'NONE',  ( 24.11249999999999716, 2.886751345948126879, 4.999999999999999112 ) ) ;
#30517 =( BOUNDED_CURVE ( )  B_SPLINE_CURVE ( 2, ( #38057, #60953, #32525, #10718, #49883, #43982, #60213 ),
 .UNSPECIFIED., .F., .F. ) 
 B_SPLINE_CURVE_WITH_KNOTS ( ( 3, 2, 2, 3 ),
 ( 0.4833333333333333925, 0.4861111111111111605, 0.4888888888888888729, 0.4916666666666666408 ),
 .UNSPECIFIED. ) 
 CURVE ( )  GEOMETRIC_REPRESENTATION_ITEM ( )  RATIONAL_B_SPLINE_CURVE ( ( 0.9999999999999973355, 0.8660254037844413721, 1.000000000000000000, 0.8660254037844387076, 1.000000000000000000, 0.8660254037844387076, 1.000000000000000000 ) ) 
 REPRESENTATION_ITEM ( '' )  );
#30518 = CARTESIAN_POINT ( 'NONE',  ( 25.17187500061451644, 3.027376345333613106, -5.243569643749998122 ) ) ;
#30519 = VERTEX_POINT ( 'NONE', #63006 ) ;
#30520 = CARTESIAN_POINT ( 'NONE',  ( 3.015485575276906527, -3.988347017152381824, -3.404139683571346442 ) ) ;
#30521 = CARTESIAN_POINT ( 'NONE',  ( 11.99062500061451608, -3.027376345333610441, -5.243569643749999898 ) ) ;
#30522 = CARTESIAN_POINT ( 'NONE',  ( 6.253125000614517148, 4.541064518000418104, -2.621784821874998173 ) ) ;
#30523 = CARTESIAN_POINT ( 'NONE',  ( 16.54687500061451644, 4.119189519843966529, -2.378215178124998275 ) ) ;
#30524 = CARTESIAN_POINT ( 'NONE',  ( 29.50312500061451360, -4.541064518000417216, -2.621784821875001281 ) ) ;
#30525 = CARTESIAN_POINT ( 'NONE',  ( 14.58750000122903323, 6.123233995736764310E-16, -4.999999999999998224 ) ) ;
#30526 = CARTESIAN_POINT ( 'NONE',  ( 19.20000000000000284, 0.000000000000000000, 4.999999999999998224 ) ) ;
#30527 = CARTESIAN_POINT ( 'NONE',  ( 26.39999999999999858, 0.000000000000000000, 4.999999999999998224 ) ) ;
#30528 = CARTESIAN_POINT ( 'NONE',  ( 3.346875000614518036, -3.027376345333614438, 5.243569643749998122 ) ) ;
#30529 = CARTESIAN_POINT ( 'NONE',  ( 9.684375000614517504, -4.541064518000419881, 2.621784821874995952 ) ) ;
#30530 = CARTESIAN_POINT ( 'NONE',  ( 20.07187500061451857, -6.054752690667223547, -1.112240025338166033E-15 ) ) ;
#30531 = CARTESIAN_POINT ( 'NONE',  ( -3.999999999999997335, 13.85000000122903607, 32.30940107675850470 ) ) ;
#30532 = VERTEX_POINT ( 'NONE', #58537 ) ;
#30533 = CARTESIAN_POINT ( 'NONE',  ( 28.67812500061451431, 6.421520780324663323E-16, -5.243569643749999010 ) ) ;
#30534 = CARTESIAN_POINT ( 'NONE',  ( 3.337499999999999911, 5.773502691896255534, 3.535250795749688894E-16 ) ) ;
#30535 = CARTESIAN_POINT ( 'NONE',  ( 4.884375000614518569, 6.421520780324663323E-16, -5.243569643749999010 ) ) ;
#30536 = CARTESIAN_POINT ( 'NONE',  ( 17.32499999999999929, 4.330127018922191873, 2.499999999999999556 ) ) ;
#30537 = CARTESIAN_POINT ( 'NONE',  ( 13.75312500061451715, -4.541064518000417216, -2.621784821875001281 ) ) ;
#30538 = CARTESIAN_POINT ( 'NONE',  ( 50.00000000000000000, -7.332543590861121174, -5.218601775200084170 ) ) ;
#30539 = DIRECTION ( 'NONE',  ( -1.000000000000000000, -0.000000000000000000, -0.000000000000000000 ) ) ;
#30540 = CARTESIAN_POINT ( 'NONE',  ( 18.30000000122903359, 5.773502691896255534, 3.535250795749688894E-16 ) ) ;
#30541 = CARTESIAN_POINT ( 'NONE',  ( 3.203127373816012646, 9.474626018533117033, 24.92290371183301900 ) ) ;
#30542 = CARTESIAN_POINT ( 'NONE',  ( 18.15937500061451715, 0.000000000000000000, 4.756430356249998326 ) ) ;
#30543 = CARTESIAN_POINT ( 'NONE',  ( 7.565625000614518036, 3.027376345333613106, -5.243569643749998122 ) ) ;
#30544 = CARTESIAN_POINT ( 'NONE',  ( 23.44687500061451502, 6.054752690667223547, 3.707466751127219781E-16 ) ) ;
#30545 = CARTESIAN_POINT ( 'NONE',  ( 4.243569643749999898, 19.18437500061451928, 30.00000000000000000 ) ) ;
#30546 = CARTESIAN_POINT ( 'NONE',  ( 23.25937500061451857, -4.541064518000417216, -2.621784821875001281 ) ) ;
#30547 = CARTESIAN_POINT ( 'NONE',  ( 6.825000000000001066, 6.123233995736764310E-16, -4.999999999999998224 ) ) ;
#30548 = CARTESIAN_POINT ( 'NONE',  ( -1.999999999999997113, 10.28750000122903430, 33.46410161513775705 ) ) ;
#30549 = CARTESIAN_POINT ( 'NONE',  ( 13.64062500061451644, -3.027376345333614438, 5.243569643749998122 ) ) ;
#30550 = CARTESIAN_POINT ( 'NONE',  ( 5.812500001229035540, 0.000000000000000000, 4.999999999999998224 ) ) ;
#30551 = ADVANCED_FACE ( 'NONE', ( #52294 ), #1695, .F. ) ;
#30552 = CARTESIAN_POINT ( 'NONE',  ( 11.37187500061451750, 3.027376345333611329, 5.243569643749999010 ) ) ;
#30553 = CARTESIAN_POINT ( 'NONE',  ( -1.839935159944503518, 4.656359355287978730, -26.43822482402454455 ) ) ;
#30554 = ORIENTED_EDGE ( 'NONE', *, *, #60483, .T. ) ;
#30555 = CARTESIAN_POINT ( 'NONE',  ( 12.59062500061451573, 6.054752690667223547, 3.707466751127219781E-16 ) ) ;
#30556 = CARTESIAN_POINT ( 'NONE',  ( 3.433818815427341686, -3.634411862891160361, -3.779699544484016016 ) ) ;
#30557 = CARTESIAN_POINT ( 'NONE',  ( 24.03750000122903430, 6.123233995736764310E-16, -4.999999999999998224 ) ) ;
#30558 = CARTESIAN_POINT ( 'NONE',  ( 10.32187500061451679, 3.027376345333613106, -5.243569643749998122 ) ) ;
#30559 = CARTESIAN_POINT ( 'NONE',  ( 14.01562500061451644, 3.027376345333611329, 5.243569643749999010 ) ) ;
#30560 = CARTESIAN_POINT ( 'NONE',  ( 29.41875000122902861, 2.886751345948129099, -4.999999999999998224 ) ) ;
#30561 = CARTESIAN_POINT ( 'NONE',  ( 24.04687500061451644, -3.027376345333614438, 5.243569643749998122 ) ) ;
#30562 = CARTESIAN_POINT ( 'NONE',  ( 0.6522972858965978560, 20.64114861271052348, 33.69936173848522998 ) ) ;
#30563 = CARTESIAN_POINT ( 'NONE',  ( 45.00000000000000000, 0.000000000000000000, 0.000000000000000000 ) ) ;
#30564 = CARTESIAN_POINT ( 'NONE',  ( -1.071796769724490117, 19.45759618943232994, 26.00000000000000000 ) ) ;
#30565 = CARTESIAN_POINT ( 'NONE',  ( 2.121784821875001281, 15.05937500061451928, -26.32496088578401938 ) ) ;
#30566 = CARTESIAN_POINT ( 'NONE',  ( 14.59687500061452070, -3.027376345333614438, 5.243569643749998122 ) ) ;
#30567 = CARTESIAN_POINT ( 'NONE',  ( 18.30000000122903359, 5.773502691896255534, 3.535250795749688894E-16 ) ) ;
#30568 = CARTESIAN_POINT ( 'NONE',  ( 13.17187500061451999, 3.027376345333611329, 5.243569643749999010 ) ) ;
#30569 = CARTESIAN_POINT ( 'NONE',  ( 4.243569643749999898, 17.77812500061451928, -30.00000000000000000 ) ) ;
#30570 = CARTESIAN_POINT ( 'NONE',  ( 20.40000000122903145, -2.886751345948125991, -5.000000000000000000 ) ) ;
#30571 = CARTESIAN_POINT ( 'NONE',  ( 12.55312500061451786, 4.541064518000418104, -2.621784821874998173 ) ) ;
#30572 = ORIENTED_EDGE ( 'NONE', *, *, #42868, .T. ) ;
#30573 = VERTEX_POINT ( 'NONE', #70005 ) ;
#30574 = CARTESIAN_POINT ( 'NONE',  ( 19.08750000000000213, 5.773502691896255534, 3.535250795749688894E-16 ) ) ;
#30575 = CARTESIAN_POINT ( 'NONE',  ( 1.626862140677534273E-15, 17.52500000122903145, -26.00000000000000355 ) ) ;
#30576 = CARTESIAN_POINT ( 'NONE',  ( 11.40937500061451892, 0.000000000000000000, 5.243569643749999010 ) ) ;
#30577 = DIRECTION ( 'NONE',  ( -1.000000000000000000, -0.000000000000000000, -0.000000000000000000 ) ) ;
#30578 = CARTESIAN_POINT ( 'NONE',  ( 13.35000000122903430, 5.773502691896255534, 3.535250795749688894E-16 ) ) ;
#30579 = CARTESIAN_POINT ( 'NONE',  ( 20.55000000122903359, 5.773502691896255534, 3.535250795749688894E-16 ) ) ;
#30580 = CARTESIAN_POINT ( 'NONE',  ( 16.52812500061451573, 6.421520780324663323E-16, -5.243569643749999010 ) ) ;
#30581 = CARTESIAN_POINT ( 'NONE',  ( 21.14062500061451289, 6.054752690667223547, 3.707466751127219781E-16 ) ) ;
#30582 = CARTESIAN_POINT ( 'NONE',  ( 28.12500000122902932, 2.886751345948129099, -4.999999999999998224 ) ) ;
#30583 = CARTESIAN_POINT ( 'NONE',  ( 26.96249999999999858, -5.773502691896255534, -1.060575238724906372E-15 ) ) ;
#30584 = CARTESIAN_POINT ( 'NONE',  ( -3.756430356249999214, 12.82812499938548534, 27.83122392262697531 ) ) ;
#30585 = CARTESIAN_POINT ( 'NONE',  ( 29.66249999999999432, -5.773502691896255534, -1.060575238724906372E-15 ) ) ;
#30586 = CARTESIAN_POINT ( 'NONE',  ( 27.15937500061451360, 0.000000000000000000, 5.243569643749999010 ) ) ;
#30587 = CARTESIAN_POINT ( 'NONE',  ( 1.071796769724491893, 14.28259618943233455, -26.00000000000000355 ) ) ;
#30588 = CARTESIAN_POINT ( 'NONE',  ( -4.243569643749997233, 16.29687500061451644, -27.54997392385601174 ) ) ;
#30589 = ADVANCED_FACE ( 'NONE', ( #19375 ), #67016, .T. ) ;
#30590 = CARTESIAN_POINT ( 'NONE',  ( 3.000000001229032875, 5.773502691896255534, 3.535250795749688894E-16 ) ) ;
#30591 = CARTESIAN_POINT ( 'NONE',  ( 5.662500000000000533, 2.886751345948126879, 4.999999999999999112 ) ) ;
#30592 = CARTESIAN_POINT ( 'NONE',  ( 9.234375000614518214, -4.541064518000419881, 2.621784821874995952 ) ) ;
#30593 = CARTESIAN_POINT ( 'NONE',  ( 28.15312500061451573, -4.541064518000417216, -2.621784821875001281 ) ) ;
#30594 = CARTESIAN_POINT ( 'NONE',  ( -1.487416814333745711E-14, 14.82500000122903572, 34.00000000000000000 ) ) ;
#30595 = CYLINDRICAL_SURFACE ( 'NONE', #63325, 4.999999999999998224 ) ;
#30596 = CARTESIAN_POINT ( 'NONE',  ( 8.287499999999999645, 5.773502691896255534, 3.535250795749688401E-16 ) ) ;
#30597 = CARTESIAN_POINT ( 'NONE',  ( 6.871875000614517504, 3.027376345333611329, 5.243569643749999010 ) ) ;
#30598 = CARTESIAN_POINT ( 'NONE',  ( 11.97187500061451892, -6.054752690667223547, -1.112240025338166033E-15 ) ) ;
#30599 = CARTESIAN_POINT ( 'NONE',  ( 3.562500000000000444, -5.773502691896255534, -1.060575238724906372E-15 ) ) ;
#30600 = CARTESIAN_POINT ( 'NONE',  ( -4.243569643749998122, 13.99062500061459602, 32.45002607614398471 ) ) ;
#30601 = CARTESIAN_POINT ( 'NONE',  ( 3.999999999999998668, 18.01249999999999929, 27.69059892324149530 ) ) ;
#30602 = CARTESIAN_POINT ( 'NONE',  ( 7.050000000000000711, 0.000000000000000000, 4.999999999999998224 ) ) ;
#30603 = CARTESIAN_POINT ( 'NONE',  ( 14.44687500061451502, 0.000000000000000000, 4.756430356249998326 ) ) ;
#30604 = CARTESIAN_POINT ( 'NONE',  ( 19.45312500061451644, 0.000000000000000000, 5.243569643749999010 ) ) ;
#30605 = CARTESIAN_POINT ( 'NONE',  ( 14.09062500061451750, -3.027376345333614438, 5.243569643749998122 ) ) ;
#30606 = CARTESIAN_POINT ( 'NONE',  ( 24.42187500061451289, -4.119189519843968306, 2.378215178124996054 ) ) ;
#30607 = CARTESIAN_POINT ( 'NONE',  ( 10.54687500061451644, -3.027376345333614438, 5.243569643749998122 ) ) ;
#30608 = CARTESIAN_POINT ( 'NONE',  ( 25.42500000000000071, 4.330127018922191873, 2.499999999999999556 ) ) ;
#30609 = CARTESIAN_POINT ( 'NONE',  ( 22.53750000122903430, -4.330127018922194537, 2.499999999999995559 ) ) ;
#30610 = CARTESIAN_POINT ( 'NONE',  ( 9.234375000614518214, -4.541064518000419881, 2.621784821874995952 ) ) ;
#30611 = CARTESIAN_POINT ( 'NONE',  ( 25.39687500061451431, -3.027376345333614438, 5.243569643749998122 ) ) ;
#30612 = CARTESIAN_POINT ( 'NONE',  ( 30.00000000000000000, 6.123233995736764310E-16, -4.999999999999998224 ) ) ;
#30613 = CARTESIAN_POINT ( 'NONE',  ( 3.242103837493086330E-14, 12.80000000122903536, -34.00000000000000000 ) ) ;
#30614 = CARTESIAN_POINT ( 'NONE',  ( 19.69687500061451857, -3.027376345333610441, -5.243569643749999898 ) ) ;
#30615 = CARTESIAN_POINT ( 'NONE',  ( 12.04687500061451821, -3.027376345333610441, -5.243569643749999898 ) ) ;
#30616 = CARTESIAN_POINT ( 'NONE',  ( -1.878215178124999163, 20.10312499938548569, 26.74683588394047007 ) ) ;
#30617 = CARTESIAN_POINT ( 'NONE',  ( 22.57499999999999929, 6.123233995736764310E-16, -4.999999999999998224 ) ) ;
#30618 = CARTESIAN_POINT ( 'NONE',  ( 2.750808005852812599, 20.68304698139313658, 33.32934212547041142 ) ) ;
#30619 = CARTESIAN_POINT ( 'NONE',  ( -2.121784821874999949, 12.13437500061451857, -33.67503911421598417 ) ) ;
#30620 = CARTESIAN_POINT ( 'NONE',  ( 24.49687500061451573, -2.746126346562646425, 4.756430356249996549 ) ) ;
#30621 = CARTESIAN_POINT ( 'NONE',  ( 14.99062500061451786, -3.027376345333614438, 5.243569643749998122 ) ) ;
#30622 = CARTESIAN_POINT ( 'NONE',  ( 4.687500000000000000, 5.773502691896255534, 3.535250795749688894E-16 ) ) ;
#30623 = DIRECTION ( 'NONE',  ( 0.000000000000000000, 0.000000000000000000, 1.000000000000000000 ) ) ;
#30624 = CARTESIAN_POINT ( 'NONE',  ( 13.64999999999999858, 4.330127018922192761, -2.499999999999997780 ) ) ;
#30625 = CARTESIAN_POINT ( 'NONE',  ( -2.000000000000000000, 19.58750000122903501, 26.53589838486224650 ) ) ;
#30626 = CARTESIAN_POINT ( 'NONE',  ( 13.20000000122903394, -2.886751345948125991, -5.000000000000000000 ) ) ;
#30627 = CARTESIAN_POINT ( 'NONE',  ( 24.30937500061451573, 4.541064518000418104, -2.621784821874998173 ) ) ;
#30628 = CYLINDRICAL_SURFACE ( 'NONE', #51316, 15.00000000000000000 ) ;
#30629 = EDGE_LOOP ( 'NONE', ( #6752, #48827, #30006, #13414 ) ) ;
#30630 = CARTESIAN_POINT ( 'NONE',  ( 19.41562500061451146, 3.027376345333611329, 5.243569643749999010 ) ) ;
#30631 = CARTESIAN_POINT ( 'NONE',  ( 4.378125000614518925, 6.421520780324663323E-16, -5.243569643749999010 ) ) ;
#30632 = CARTESIAN_POINT ( 'NONE',  ( 20.18437500061451573, 6.421520780324663323E-16, -5.243569643749999010 ) ) ;
#30633 = CARTESIAN_POINT ( 'NONE',  ( 29.25937500061451502, 4.541064518000418104, -2.621784821874998173 ) ) ;
#30634 = CARTESIAN_POINT ( 'NONE',  ( 4.190625000614518925, -3.027376345333614438, 5.243569643749998122 ) ) ;
#30635 = CARTESIAN_POINT ( 'NONE',  ( 21.74062500061451431, -3.027376345333614438, 5.243569643749998122 ) ) ;
#30636 = CARTESIAN_POINT ( 'NONE',  ( -4.243569643749999898, 14.85312500061451679, 30.00000000000000000 ) ) ;
#30637 = CARTESIAN_POINT ( 'NONE',  ( 19.57500000122903216, 2.886751345948129099, -4.999999999999998224 ) ) ;
#30638 = CARTESIAN_POINT ( 'NONE',  ( 12.79687500061451821, -2.746126346562646425, 4.756430356249996549 ) ) ;
#30639 = CARTESIAN_POINT ( 'NONE',  ( 8.203125000614518214, 0.000000000000000000, 5.243569643749999010 ) ) ;
#30640 = CARTESIAN_POINT ( 'NONE',  ( 3.346875000614518036, -3.027376345333614438, 5.243569643749998122 ) ) ;
#30641 = CARTESIAN_POINT ( 'NONE',  ( 2.859375000614519546, 0.000000000000000000, 5.243569643749999010 ) ) ;
#30642 = ADVANCED_FACE ( 'NONE', ( #59228 ), #53707, .F. ) ;
#30643 = CARTESIAN_POINT ( 'NONE',  ( 22.62187500061451573, 3.027376345333611329, 5.243569643749999010 ) ) ;
#30644 = CARTESIAN_POINT ( 'NONE',  ( 14.61562500061451608, -6.054752690667223547, -1.112240025338166033E-15 ) ) ;
#30645 = CARTESIAN_POINT ( 'NONE',  ( 24.93750000122903288, 6.123233995736764310E-16, -4.999999999999998224 ) ) ;
#30646 = CARTESIAN_POINT ( 'NONE',  ( 25.94062500061451715, -3.027376345333610441, -5.243569643749999898 ) ) ;
#30647 = CARTESIAN_POINT ( 'NONE',  ( 19.73437500061451644, 6.421520780324663323E-16, -5.243569643749999010 ) ) ;
#30648 = CARTESIAN_POINT ( 'NONE',  ( 14.01562500061451644, 3.027376345333611329, 5.243569643749999010 ) ) ;
#30649 = CARTESIAN_POINT ( 'NONE',  ( -2.121784821874999949, 17.08437500061451786, 26.32496088578401938 ) ) ;
#30650 = CARTESIAN_POINT ( 'NONE',  ( 19.37812500061451715, 4.541064518000418104, 2.621784821874999949 ) ) ;
#30651 = CARTESIAN_POINT ( 'NONE',  ( 23.30625000122903145, 0.000000000000000000, 4.999999999999998224 ) ) ;
#30652 = ORIENTED_EDGE ( 'NONE', *, *, #30487, .T. ) ;
#30653 = CARTESIAN_POINT ( 'NONE',  ( 25.23749999999999716, -2.886751345948125991, -5.000000000000000000 ) ) ;
#30654 = CARTESIAN_POINT ( 'NONE',  ( 8.484601909799253346E-16, 11.11250000000000071, -25.38119784648299770 ) ) ;
#30655 = CARTESIAN_POINT ( 'NONE',  ( 3.756430356250000546, 19.09062499938548640, 27.83122392262697886 ) ) ;
#30656 = CARTESIAN_POINT ( 'NONE',  ( 27.17812500061451786, -4.541064518000419881, 2.621784821874995952 ) ) ;
#30657 = CARTESIAN_POINT ( 'NONE',  ( 7.790625000614518569, -3.027376345333614438, 5.243569643749998122 ) ) ;
#30658 = CARTESIAN_POINT ( 'NONE',  ( 19.95000000122903572, -2.886751345948125991, -5.000000000000000000 ) ) ;
#30659 = CARTESIAN_POINT ( 'NONE',  ( 25.34062500061451217, -3.027376345333614438, 5.243569643749998122 ) ) ;
#30660 = CARTESIAN_POINT ( 'NONE',  ( 24.48749999999999716, 5.773502691896255534, 3.535250795749688894E-16 ) ) ;
#30661 = CARTESIAN_POINT ( 'NONE',  ( -1.999999999999997113, 15.68750000122903465, -26.53589838486224295 ) ) ;
#30662 = CARTESIAN_POINT ( 'NONE',  ( 28.07812500061451289, -4.541064518000419881, 2.621784821874995952 ) ) ;
#30663 = CARTESIAN_POINT ( 'NONE',  ( 10.71562500061451928, 3.027376345333613106, -5.243569643749998122 ) ) ;
#30664 = ORIENTED_EDGE ( 'NONE', *, *, #26043, .F. ) ;
#30665 = CARTESIAN_POINT ( 'NONE',  ( 26.39062500061451644, -3.027376345333610441, -5.243569643749999898 ) ) ;
#30666 = CARTESIAN_POINT ( 'NONE',  ( 5.015625000614518214, 3.027376345333611329, 5.243569643749999010 ) ) ;
#30667 = CARTESIAN_POINT ( 'NONE',  ( 14.63437500061451679, -4.119189519843968306, 2.378215178124996054 ) ) ;
#30668 = DIRECTION ( 'NONE',  ( 0.000000000000000000, 0.000000000000000000, -1.000000000000000000 ) ) ;
#30669 = CARTESIAN_POINT ( 'NONE',  ( 12.18750000000000000, -2.886751345948125991, -5.000000000000000000 ) ) ;
#30670 =( BOUNDED_CURVE ( )  B_SPLINE_CURVE ( 2, ( #38616, #16067, #11266, #67068, #61139, #62231, #66693, #55602, #72958 ),
 .UNSPECIFIED., .F., .F. ) 
 B_SPLINE_CURVE_WITH_KNOTS ( ( 3, 2, 2, 2, 3 ),
 ( 0.8369565217391304879, 0.8405797101449274944, 0.8478260869565217295, 0.8550724637681159646, 0.8586956521739130821 ),
 .UNSPECIFIED. ) 
 CURVE ( )  GEOMETRIC_REPRESENTATION_ITEM ( )  RATIONAL_B_SPLINE_CURVE ( ( 0.9330127018922192983, 0.9330127018922202975, 1.000000000000000000, 0.8660254037844387076, 1.000000000000000000, 0.8660254037844387076, 1.000000000000000000, 0.9330127018922194093, 0.9330127018922194093 ) ) 
 REPRESENTATION_ITEM ( '' )  );
#30671 = CARTESIAN_POINT ( 'NONE',  ( 13.35937500061451821, -4.541064518000417216, -2.621784821875001281 ) ) ;
#30672 = CARTESIAN_POINT ( 'NONE',  ( 9.450000001229033941, -2.886751345948129988, 4.999999999999997335 ) ) ;
#30673 = CARTESIAN_POINT ( 'NONE',  ( 17.48437500061451999, 6.421520780324663323E-16, -5.243569643749999010 ) ) ;
#30674 = CARTESIAN_POINT ( 'NONE',  ( 14.84999999999999964, -4.330127018922190985, -2.500000000000001332 ) ) ;
#30675 = CARTESIAN_POINT ( 'NONE',  ( 8.334375000614516082, -4.541064518000419881, 2.621784821874995952 ) ) ;
#30676 = CARTESIAN_POINT ( 'NONE',  ( -2.121784821874996840, 11.77812500061451750, -26.32496088578401583 ) ) ;
#30677 = CARTESIAN_POINT ( 'NONE',  ( 20.24999999999999645, -4.330127018922190985, -2.500000000000001332 ) ) ;
#30678 = CARTESIAN_POINT ( 'NONE',  ( 23.89687500061451431, 0.000000000000000000, 4.756430356249998326 ) ) ;
#30679 = EDGE_CURVE ( 'NONE', #32129, #5008, #52541, .T. ) ;
#30680 = CARTESIAN_POINT ( 'NONE',  ( 23.99062500061451786, -3.027376345333614438, 5.243569643749998122 ) ) ;
#30681 = CARTESIAN_POINT ( 'NONE',  ( -5.810221930991193690E-16, 11.78749999999999964, 26.00000000000000355 ) ) ;
#30682 = EDGE_CURVE ( 'NONE', #14158, #31771, #52305, .T. ) ;
#30683 = CARTESIAN_POINT ( 'NONE',  ( -1.071796769724487453, 17.32009619066136707, 26.00000000000000000 ) ) ;
#30684 = CARTESIAN_POINT ( 'NONE',  ( 25.09687500061451715, -3.027376345333610441, -5.243569643749999898 ) ) ;
#30685 = CARTESIAN_POINT ( 'NONE',  ( 28.05937500061451573, 0.000000000000000000, 5.243569643749999010 ) ) ;
#30686 = CARTESIAN_POINT ( 'NONE',  ( 4.078125000614517326, 4.541064518000418104, 2.621784821874999949 ) ) ;
#30687 = CARTESIAN_POINT ( 'NONE',  ( 21.45937500061451075, 2.746126346562645981, -4.756430356249997438 ) ) ;
#30688 = CARTESIAN_POINT ( 'NONE',  ( 16.73437500061451644, 4.541064518000418104, 2.621784821874999949 ) ) ;
#30689 = CARTESIAN_POINT ( 'NONE',  ( 9.496875000614517504, 0.000000000000000000, 4.756430356249998326 ) ) ;
#30690 = CARTESIAN_POINT ( 'NONE',  ( 3.965625000614515727, 3.027376345333613106, -5.243569643749998122 ) ) ;
#30691 = CARTESIAN_POINT ( 'NONE',  ( 7.246875000614518392, 6.054752690667223547, 3.707466751127219781E-16 ) ) ;
#30692 = CARTESIAN_POINT ( 'NONE',  ( 19.24687500061452283, -3.027376345333610441, -5.243569643749999898 ) ) ;
#30693 = CARTESIAN_POINT ( 'NONE',  ( -2.007927870956448313, 25.40597574392634428, 26.53059533024969241 ) ) ;
#30694 = CARTESIAN_POINT ( 'NONE',  ( 26.62500000000000000, 6.123233995736764310E-16, -4.999999999999998224 ) ) ;
#30695 = CARTESIAN_POINT ( 'NONE',  ( 26.93437500061451573, 6.421520780324663323E-16, -5.243569643749999010 ) ) ;
#30696 = CARTESIAN_POINT ( 'NONE',  ( 14.36250000122903359, 0.000000000000000000, 4.999999999999998224 ) ) ;
#30697 = VERTEX_POINT ( 'NONE', #71803 ) ;
#30698 = CARTESIAN_POINT ( 'NONE',  ( 7.987500000000000711, -2.886751345948129988, 4.999999999999997335 ) ) ;
#30699 = CARTESIAN_POINT ( 'NONE',  ( 8.446875000614515017, 4.119189519843966529, -2.378215178124998275 ) ) ;
#30700 = CARTESIAN_POINT ( 'NONE',  ( 22.75312500061451360, -4.541064518000417216, -2.621784821875001281 ) ) ;
#30701 = CARTESIAN_POINT ( 'NONE',  ( 12.26249999999999929, 2.886751345948129099, -4.999999999999998224 ) ) ;
#30702 = CARTESIAN_POINT ( 'NONE',  ( 8.737500001229033586, 6.123233995736764310E-16, -4.999999999999998224 ) ) ;
#30703 = CARTESIAN_POINT ( 'NONE',  ( 5.615625000614517859, -6.054752690667223547, -1.112240025338166033E-15 ) ) ;
#30704 = CARTESIAN_POINT ( 'NONE',  ( 21.22500000000000142, 6.123233995736764310E-16, -4.999999999999998224 ) ) ;
#30705 = CARTESIAN_POINT ( 'NONE',  ( 18.40312500061451573, 4.541064518000418104, -2.621784821874998173 ) ) ;
#30706 = CARTESIAN_POINT ( 'NONE',  ( 4.162909324394188815, -2.769634124722277768, 4.389987815956644113 ) ) ;
#30707 = CARTESIAN_POINT ( 'NONE',  ( 25.72500000122903074, -5.773502691896255534, -1.060575238724906372E-15 ) ) ;
#30708 = CARTESIAN_POINT ( 'NONE',  ( 1.878215178125000495, 18.56562499938548427, 26.74683588394047007 ) ) ;
#30709 = CARTESIAN_POINT ( 'NONE',  ( 4.125000000000000000, 6.123233995736764310E-16, -4.999999999999998224 ) ) ;
#30710 = ORIENTED_EDGE ( 'NONE', *, *, #57824, .F. ) ;
#30711 = CARTESIAN_POINT ( 'NONE',  ( 19.45312500061451644, 0.000000000000000000, 5.243569643749999010 ) ) ;
#30712 = CARTESIAN_POINT ( 'NONE',  ( 27.59062500061451573, -3.027376345333614438, 5.243569643749998122 ) ) ;
#30713 = CARTESIAN_POINT ( 'NONE',  ( 26.33437500061451431, -4.541064518000419881, 2.621784821874995952 ) ) ;
#30714 = CARTESIAN_POINT ( 'NONE',  ( 9.449999999999999289, -4.330127018922190985, -2.500000000000001332 ) ) ;
#30715 = CARTESIAN_POINT ( 'NONE',  ( 13.52812500061451750, 4.541064518000418104, 2.621784821874999949 ) ) ;
#30716 = CARTESIAN_POINT ( 'NONE',  ( 1.999999999999998668, 11.30000000000000071, 26.53589838486224650 ) ) ;
#30717 = CARTESIAN_POINT ( 'NONE',  ( 10.04062500061451502, -3.027376345333614438, 5.243569643749998122 ) ) ;
#30718 = DIRECTION ( 'NONE',  ( -1.000000000000000000, -0.000000000000000000, -0.000000000000000000 ) ) ;
#30719 = CARTESIAN_POINT ( 'NONE',  ( 2.121784821875001281, 12.35937500061451821, 33.67503911421598417 ) ) ;
#30720 =( BOUNDED_CURVE ( )  B_SPLINE_CURVE ( 2, ( #66346, #15724, #32732, #33815, #38643, #27560, #50091 ),
 .UNSPECIFIED., .F., .F. ) 
 B_SPLINE_CURVE_WITH_KNOTS ( ( 3, 2, 2, 3 ),
 ( 0.8416666666666667851, 0.8444444444444445530, 0.8472222222222222099, 0.8499999999999999778 ),
 .UNSPECIFIED. ) 
 CURVE ( )  GEOMETRIC_REPRESENTATION_ITEM ( )  RATIONAL_B_SPLINE_CURVE ( ( 0.9999999999999946709, 0.8660254037844440367, 1.000000000000000000, 0.8660254037844387076, 1.000000000000000000, 0.8660254037844387076, 1.000000000000000000 ) ) 
 REPRESENTATION_ITEM ( '' )  );
#30721 = CARTESIAN_POINT ( 'NONE',  ( 25.31250000122903288, -4.330127018922190985, -2.500000000000001332 ) ) ;
#30722 = CARTESIAN_POINT ( 'NONE',  ( 19.95937500061451786, 0.000000000000000000, 4.756430356249998326 ) ) ;
#30723 = CARTESIAN_POINT ( 'NONE',  ( 17.35312500061451502, -4.541064518000417216, -2.621784821875001281 ) ) ;
#30724 = CARTESIAN_POINT ( 'NONE',  ( 8.137500000000002842, -2.886751345948126435, -5.000000000000000000 ) ) ;
#30725 = EDGE_CURVE ( 'NONE', #15843, #68418, #38605, .T. ) ;
#30726 = CARTESIAN_POINT ( 'NONE',  ( 9.346875000614517148, -3.027376345333610441, -5.243569643749999898 ) ) ;
#30727 = CARTESIAN_POINT ( 'NONE',  ( 10.77187500061451786, 3.027376345333613106, -5.243569643749998122 ) ) ;
#30728 = CARTESIAN_POINT ( 'NONE',  ( 17.67187500061451644, 3.027376345333611329, 5.243569643749999010 ) ) ;
#30729 = ORIENTED_EDGE ( 'NONE', *, *, #61885, .T. ) ;
#30730 = CARTESIAN_POINT ( 'NONE',  ( 15.29999999999999893, -4.330127018922190985, -2.500000000000001332 ) ) ;
#30731 = CARTESIAN_POINT ( 'NONE',  ( 22.15312500061451573, 0.000000000000000000, 5.243569643749999010 ) ) ;
#30732 = CARTESIAN_POINT ( 'NONE',  ( 17.03437500061451715, 6.421520780324663323E-16, -5.243569643749999010 ) ) ;
#30733 = CARTESIAN_POINT ( 'NONE',  ( 22.86562500061451431, 3.027376345333613106, -5.243569643749998122 ) ) ;
#30734 = CARTESIAN_POINT ( 'NONE',  ( -3.999999999999997335, 13.28749999999999964, 32.30940107675850470 ) ) ;
#30735 = CARTESIAN_POINT ( 'NONE',  ( 28.11562500061451431, -6.054752690667223547, -1.112240025338166033E-15 ) ) ;
#30736 = CARTESIAN_POINT ( 'NONE',  ( 7.687500001229033764, -4.330127018922194537, 2.499999999999995559 ) ) ;
#30737 = ORIENTED_EDGE ( 'NONE', *, *, #56475, .T. ) ;
#30738 = CARTESIAN_POINT ( 'NONE',  ( 4.987500001229032698, -4.330127018922194537, 2.499999999999995559 ) ) ;
#30739 = CARTESIAN_POINT ( 'NONE',  ( 3.999999999999998668, 17.11250000000000071, -32.30940107675850470 ) ) ;
#30740 = CARTESIAN_POINT ( 'NONE',  ( 23.81250000122903288, 0.000000000000000000, 4.999999999999998224 ) ) ;
#30741 = CARTESIAN_POINT ( 'NONE',  ( -4.000000000000000000, 20.31874999877096499, 30.00000000000000000 ) ) ;
#30742 = CARTESIAN_POINT ( 'NONE',  ( 8.221875000614518925, 3.027376345333611329, 5.243569643749999010 ) ) ;
#30743 = CARTESIAN_POINT ( 'NONE',  ( 1.999999999999998668, 15.35000000000000142, 26.53589838486224650 ) ) ;
#30744 = CARTESIAN_POINT ( 'NONE',  ( 15.17812500061451608, 6.421520780324663323E-16, -5.243569643749999010 ) ) ;
#30745 = CARTESIAN_POINT ( 'NONE',  ( 9.646875000614516082, -3.027376345333614438, 5.243569643749998122 ) ) ;
#30746 = CARTESIAN_POINT ( 'NONE',  ( 27.15000000122902790, -2.886751345948125991, -5.000000000000000000 ) ) ;
#30747 = CARTESIAN_POINT ( 'NONE',  ( 17.03437500061451715, 6.421520780324663323E-16, -5.243569643749999010 ) ) ;
#30748 = CARTESIAN_POINT ( 'NONE',  ( 4.696875000614518569, -3.027376345333614438, 5.243569643749998122 ) ) ;
#30749 = CARTESIAN_POINT ( 'NONE',  ( 1.999999999999997335, 18.72499999999999787, 33.46410161513775705 ) ) ;
#30750 = CARTESIAN_POINT ( 'NONE',  ( 4.415625000614518569, 3.027376345333613106, -5.243569643749998122 ) ) ;
#30751 = CARTESIAN_POINT ( 'NONE',  ( 18.55312500061451431, 0.000000000000000000, 5.243569643749999010 ) ) ;
#30752 =( BOUNDED_CURVE ( )  B_SPLINE_CURVE ( 2, ( #25355, #52704, #47901, #52344, #8730, #35346, #2110 ),
 .UNSPECIFIED., .F., .F. ) 
 B_SPLINE_CURVE_WITH_KNOTS ( ( 3, 2, 2, 3 ),
 ( 0.1083333333333333648, 0.1111111111111111327, 0.1138888888888889006, 0.1166666666666666824 ),
 .UNSPECIFIED. ) 
 CURVE ( )  GEOMETRIC_REPRESENTATION_ITEM ( )  RATIONAL_B_SPLINE_CURVE ( ( 0.9999999999999986677, 0.8660254037844400399, 1.000000000000000000, 0.8660254037844387076, 1.000000000000000000, 0.8660254037844380415, 1.000000000000000666 ) ) 
 REPRESENTATION_ITEM ( '' )  );
#30753 = ORIENTED_EDGE ( 'NONE', *, *, #68178, .F. ) ;
#30754 = CARTESIAN_POINT ( 'NONE',  ( 11.87812500061451537, -4.541064518000419881, 2.621784821874995952 ) ) ;
#30755 = CARTESIAN_POINT ( 'NONE',  ( 6.000000001229033764, -2.886751345948125991, -5.000000000000000000 ) ) ;
#30756 = CARTESIAN_POINT ( 'NONE',  ( 11.50312500061451892, -4.541064518000417216, -2.621784821875001281 ) ) ;
#30757 = CARTESIAN_POINT ( 'NONE',  ( 21.12187500061451573, 2.746126346562645981, -4.756430356249997438 ) ) ;
#30758 = CARTESIAN_POINT ( 'NONE',  ( 10.20000000000000107, 0.000000000000000000, 4.999999999999998224 ) ) ;
#30759 = CARTESIAN_POINT ( 'NONE',  ( 5.962500001229033231, -4.330127018922190985, -2.500000000000001332 ) ) ;
#30760 = CARTESIAN_POINT ( 'NONE',  ( 20.58750000000000213, -2.886751345948129988, 4.999999999999997335 ) ) ;
#30761 = CARTESIAN_POINT ( 'NONE',  ( 15.04687500061451644, -3.027376345333614438, 5.243569643749998122 ) ) ;
#30762 = CARTESIAN_POINT ( 'NONE',  ( 15.07500000122903394, 2.886751345948129099, -4.999999999999998224 ) ) ;
#30763 = CARTESIAN_POINT ( 'NONE',  ( 21.60000000000000142, -4.330127018922190985, -2.500000000000001332 ) ) ;
#30764 =( BOUNDED_CURVE ( )  B_SPLINE_CURVE ( 2, ( #10587, #73006, #5773, #44215, #66747, #16474, #22390 ),
 .UNSPECIFIED., .F., .F. ) 
 B_SPLINE_CURVE_WITH_KNOTS ( ( 3, 2, 2, 3 ),
 ( 0.4333333333333333481, 0.4361111111111111160, 0.4388888888888888840, 0.4416666666666666519 ),
 .UNSPECIFIED. ) 
 CURVE ( )  GEOMETRIC_REPRESENTATION_ITEM ( )  RATIONAL_B_SPLINE_CURVE ( ( 1.000000000000000000, 0.8660254037844387076, 1.000000000000000000, 0.8660254037844387076, 1.000000000000000000, 0.8660254037844387076, 1.000000000000000000 ) ) 
 REPRESENTATION_ITEM ( '' )  );
#30765 = CARTESIAN_POINT ( 'NONE',  ( 2.121784821875001281, 19.50312500061451360, -26.32496088578401938 ) ) ;
#30766 = CARTESIAN_POINT ( 'NONE',  ( 1.592000809091587073E-14, 15.95000000122903394, 26.00000000000000000 ) ) ;
#30767 = DIRECTION ( 'NONE',  ( -1.000000000000000000, -0.000000000000000000, -0.000000000000000000 ) ) ;
#30768 = FACE_OUTER_BOUND ( 'NONE', #21712, .T. ) ;
#30769 = FACE_OUTER_BOUND ( 'NONE', #19241, .T. ) ;
#30770 = CARTESIAN_POINT ( 'NONE',  ( 3.906976797710813631, -3.120192015497321059, -4.214200603120166200 ) ) ;
#30771 = CARTESIAN_POINT ( 'NONE',  ( 16.65937500061452070, 4.541064518000418104, -2.621784821874998173 ) ) ;
#30772 = EDGE_CURVE ( 'NONE', #17531, #56113, #31332, .T. ) ;
#30773 = CARTESIAN_POINT ( 'NONE',  ( 28.42499999999999716, 6.123233995736764310E-16, -4.999999999999998224 ) ) ;
#30774 = CARTESIAN_POINT ( 'NONE',  ( 11.50312500061451892, -4.541064518000417216, -2.621784821875001281 ) ) ;
#30775 = CARTESIAN_POINT ( 'NONE',  ( 29.63437500061451857, 5.492252693125287522, 3.363034840372157021E-16 ) ) ;
#30776 = CARTESIAN_POINT ( 'NONE',  ( 24.15937500061451715, -4.541064518000417216, -2.621784821875001281 ) ) ;
#30777 = CARTESIAN_POINT ( 'NONE',  ( 15.34687500061451537, 0.000000000000000000, 4.756430356249998326 ) ) ;
#30778 = CARTESIAN_POINT ( 'NONE',  ( 9.515625000614518214, 3.027376345333611329, 5.243569643749999010 ) ) ;
#30779 = CARTESIAN_POINT ( 'NONE',  ( 14.37187500061451928, 3.027376345333613106, -5.243569643749998122 ) ) ;
#30780 = ORIENTED_EDGE ( 'NONE', *, *, #3046, .F. ) ;
#30781 = CARTESIAN_POINT ( 'NONE',  ( 25.73437500061451644, 4.541064518000418104, 2.621784821874999949 ) ) ;
#30782 = CARTESIAN_POINT ( 'NONE',  ( 27.47812500061451502, 4.541064518000418104, 2.621784821874999949 ) ) ;
#30783 = CARTESIAN_POINT ( 'NONE',  ( 19.07812500061451644, -4.541064518000419881, 2.621784821874995952 ) ) ;
#30784 = CARTESIAN_POINT ( 'NONE',  ( 28.00312500061451715, 0.000000000000000000, 5.243569643749999010 ) ) ;
#30785 = CARTESIAN_POINT ( 'NONE',  ( 1.071796769724505438, 12.77990381179669832, -33.99999999999999289 ) ) ;
#30786 = CARTESIAN_POINT ( 'NONE',  ( 8.512499999999999289, -5.773502691896255534, -1.060575238724906372E-15 ) ) ;
#30787 = CARTESIAN_POINT ( 'NONE',  ( 18.60000000122903430, -2.886751345948125991, -5.000000000000000000 ) ) ;
#30788 = LINE ( 'NONE', #19689, #44338 ) ;
#30789 = CARTESIAN_POINT ( 'NONE',  ( 8.034375000614515372, 5.492252693125287522, 3.363034840372157021E-16 ) ) ;
#30790 = ORIENTED_EDGE ( 'NONE', *, *, #59478, .F. ) ;
#30791 = CARTESIAN_POINT ( 'NONE',  ( 15.86250000000000249, 2.886751345948129099, -4.999999999999998224 ) ) ;
#30792 = VECTOR ( 'NONE', #13975, 1000.000000000000000 ) ;
#30793 = CARTESIAN_POINT ( 'NONE',  ( 18.14999999999999858, 4.330127018922192761, -2.499999999999997780 ) ) ;
#30794 = CARTESIAN_POINT ( 'NONE',  ( 15.98437500061451821, -4.541064518000419881, 2.621784821874995952 ) ) ;
#30795 = CARTESIAN_POINT ( 'NONE',  ( 12.92812500061451786, 6.421520780324663323E-16, -5.243569643749999010 ) ) ;
#30796 = VERTEX_POINT ( 'NONE', #32269 ) ;
#30797 = CARTESIAN_POINT ( 'NONE',  ( -2.000000000000001776, 16.79374999877096641, 33.46410161513775705 ) ) ;
#30798 = CARTESIAN_POINT ( 'NONE',  ( 7.003125000614518036, -4.541064518000417216, -2.621784821875001281 ) ) ;
#30799 = CARTESIAN_POINT ( 'NONE',  ( 12.30000000000000249, 4.330127018922192761, -2.499999999999997780 ) ) ;
#30800 = CARTESIAN_POINT ( 'NONE',  ( 29.37187500061451573, -4.119189519843968306, 2.378215178124996054 ) ) ;
#30801 = CARTESIAN_POINT ( 'NONE',  ( -2.121784821874999949, 14.32812500061451644, 26.32496088578401938 ) ) ;
#30802 = CARTESIAN_POINT ( 'NONE',  ( 26.91562500061451146, 3.027376345333613106, -5.243569643749998122 ) ) ;
#30803 = CARTESIAN_POINT ( 'NONE',  ( 8.324999999999999289, 4.330127018922191873, 2.499999999999999556 ) ) ;
#30804 = CARTESIAN_POINT ( 'NONE',  ( 3.756430356250000546, 17.62812499938548427, 27.83122392262697886 ) ) ;
#30805 = CARTESIAN_POINT ( 'NONE',  ( 24.00937500061451502, 0.000000000000000000, 5.243569643749999010 ) ) ;
#30806 = CARTESIAN_POINT ( 'NONE',  ( 20.65312500061451573, 4.541064518000418104, -2.621784821874998173 ) ) ;
#30807 = CARTESIAN_POINT ( 'NONE',  ( -2.121784821874996840, 17.17812500061459602, -26.32496088578401583 ) ) ;
#30808 = CARTESIAN_POINT ( 'NONE',  ( 22.80000000122903359, 5.773502691896255534, 3.535250795749688894E-16 ) ) ;
#30809 = CARTESIAN_POINT ( 'NONE',  ( 7.490625000614516082, -3.027376345333610441, -5.243569643749999898 ) ) ;
#30810 = CARTESIAN_POINT ( 'NONE',  ( 27.08437500061451786, 4.119189519843966529, 2.378215178124999607 ) ) ;
#30811 = CARTESIAN_POINT ( 'NONE',  ( 23.46562500061451573, 3.027376345333611329, 5.243569643749999010 ) ) ;
#30812 = CARTESIAN_POINT ( 'NONE',  ( 9.346875000614517148, -2.746126346562642428, -4.756430356249999214 ) ) ;
#30813 = CARTESIAN_POINT ( 'NONE',  ( 2.655984681222220721E-16, 15.00312499938548427, 25.66244784525396483 ) ) ;
#30814 = CARTESIAN_POINT ( 'NONE',  ( 15.94687500061451502, -3.027376345333614438, 5.243569643749998122 ) ) ;
#30815 = CARTESIAN_POINT ( 'NONE',  ( 24.53437500061451715, -4.541064518000419881, 2.621784821874995952 ) ) ;
#30816 = CARTESIAN_POINT ( 'NONE',  ( 4.243569643749999898, 14.68437500061451750, 30.00000000000000000 ) ) ;
#30817 = CARTESIAN_POINT ( 'NONE',  ( 5.240625000614516971, -3.027376345333610441, -5.243569643749999898 ) ) ;
#30818 = CARTESIAN_POINT ( 'NONE',  ( 28.22812500061451502, 6.421520780324663323E-16, -5.243569643749999010 ) ) ;
#30819 = EDGE_CURVE ( 'NONE', #35463, #11388, #7705, .T. ) ;
#30820 = CARTESIAN_POINT ( 'NONE',  ( 29.57812500061451644, 6.421520780324663323E-16, -5.243569643749999010 ) ) ;
#30821 = DIRECTION ( 'NONE',  ( 0.000000000000000000, 0.000000000000000000, -1.000000000000000000 ) ) ;
#30822 = CARTESIAN_POINT ( 'NONE',  ( 3.807538167735159185, -3.240779705755961526, 4.122180188640082399 ) ) ;
#30823 = CARTESIAN_POINT ( 'NONE',  ( 2.878125000614517592, -4.541064518000419881, 2.621784821874995952 ) ) ;
#30824 = CARTESIAN_POINT ( 'NONE',  ( 7.921875000614517326, -6.054752690667223547, -1.112240025338166033E-15 ) ) ;
#30825 = CARTESIAN_POINT ( 'NONE',  ( 16.95000000122903216, 5.773502691896255534, 3.535250795749688894E-16 ) ) ;
#30826 = CARTESIAN_POINT ( 'NONE',  ( 3.234375000614516438, 4.541064518000418104, 2.621784821874999949 ) ) ;
#30827 = CARTESIAN_POINT ( 'NONE',  ( 4.828125000614518214, 6.421520780324663323E-16, -5.243569643749999010 ) ) ;
#30828 = CARTESIAN_POINT ( 'NONE',  ( 4.000000000000000000, 13.34374999877096712, 30.00000000000000000 ) ) ;
#30829 = CARTESIAN_POINT ( 'NONE',  ( 21.65625000122903288, -4.330127018922190985, -2.500000000000001332 ) ) ;
#30830 = CARTESIAN_POINT ( 'NONE',  ( 13.43437500061451750, 6.421520780324663323E-16, -5.243569643749999010 ) ) ;
#30831 = CARTESIAN_POINT ( 'NONE',  ( 27.52500000000000213, 6.123233995736764310E-16, -4.999999999999998224 ) ) ;
#30832 = VERTEX_POINT ( 'NONE', #15267 ) ;
#30833 = CARTESIAN_POINT ( 'NONE',  ( 22.71562500061451573, -6.054752690667223547, -1.112240025338166033E-15 ) ) ;
#30834 = CARTESIAN_POINT ( 'NONE',  ( 6.478125000614516793, -4.541064518000419881, 2.621784821874995952 ) ) ;
#30835 = CARTESIAN_POINT ( 'NONE',  ( 25.17187500061451644, 3.027376345333612662, -5.243569643749998122 ) ) ;
#30836 = CARTESIAN_POINT ( 'NONE',  ( 8.315625000614515372, -6.054752690667223547, -1.112240025338166033E-15 ) ) ;
#30837 = CARTESIAN_POINT ( 'NONE',  ( 3.504965621013899746, 3.565840152826760256, 3.504965621013765631 ) ) ;
#30838 = CARTESIAN_POINT ( 'NONE',  ( 10.12500000122903465, 2.886751345948129099, -4.999999999999998224 ) ) ;
#30839 = CARTESIAN_POINT ( 'NONE',  ( 25.30312500061451431, 0.000000000000000000, 5.243569643749999010 ) ) ;
#30840 = CARTESIAN_POINT ( 'NONE',  ( 4.243569643749999010, 10.61562500061451786, -32.45002607614398471 ) ) ;
#30841 = CARTESIAN_POINT ( 'NONE',  ( 9.562500001229032875, -4.330127018922190985, -2.500000000000001332 ) ) ;
#30842 = CARTESIAN_POINT ( 'NONE',  ( 23.27812500061451573, 6.421520780324663323E-16, -5.243569643749999010 ) ) ;
#30843 = CARTESIAN_POINT ( 'NONE',  ( 18.06562500061451715, 3.027376345333611329, 5.243569643749999010 ) ) ;
#30844 = CARTESIAN_POINT ( 'NONE',  ( 27.79687500061451999, -2.746126346562642428, -4.756430356249999214 ) ) ;
#30845 = CARTESIAN_POINT ( 'NONE',  ( 19.20000000000000284, 0.000000000000000000, 4.999999999999998224 ) ) ;
#30846 = CARTESIAN_POINT ( 'NONE',  ( 14.92500000122903181, -5.773502691896255534, -1.060575238724906372E-15 ) ) ;
#30847 = CARTESIAN_POINT ( 'NONE',  ( 11.16562500061451679, 3.027376345333613106, -5.243569643749998122 ) ) ;
#30848 = CARTESIAN_POINT ( 'NONE',  ( 12.55312500061451786, 4.541064518000418104, -2.621784821874998173 ) ) ;
#30849 = CARTESIAN_POINT ( 'NONE',  ( 23.62500000122902932, 2.886751345948129099, -4.999999999999998224 ) ) ;
#30850 = CARTESIAN_POINT ( 'NONE',  ( 23.03437500061451715, 4.541064518000418104, 2.621784821874999949 ) ) ;
#30851 = CARTESIAN_POINT ( 'NONE',  ( 21.87187500061451573, -6.054752690667223547, -1.112240025338166033E-15 ) ) ;
#30852 = CARTESIAN_POINT ( 'NONE',  ( 24.89999999999999858, 4.330127018922192761, -2.499999999999997780 ) ) ;
#30853 = CARTESIAN_POINT ( 'NONE',  ( 7.425000001229034474, 2.886751345948129099, -4.999999999999998224 ) ) ;
#30854 = CARTESIAN_POINT ( 'NONE',  ( 5.784375000614517148, 6.421520780324663323E-16, -5.243569643749999010 ) ) ;
#30855 = CARTESIAN_POINT ( 'NONE',  ( 22.73437500061451644, -4.541064518000419881, 2.621784821874995952 ) ) ;
#30856 = CARTESIAN_POINT ( 'NONE',  ( 26.70000000122903216, -2.886751345948142422, -4.999999999999970690 ) ) ;
#30857 = CARTESIAN_POINT ( 'NONE',  ( 21.77812500061451928, -4.541064518000419881, 2.621784821874995952 ) ) ;
#30858 = CARTESIAN_POINT ( 'NONE',  ( 25.02187500061451431, -6.054752690667223547, -1.112240025338166033E-15 ) ) ;
#30859 = CARTESIAN_POINT ( 'NONE',  ( 1.878215178125000495, 18.67812499938548143, 26.74683588394047007 ) ) ;
#30860 = CARTESIAN_POINT ( 'NONE',  ( 17.84999999999999787, 0.000000000000000000, 4.999999999999998224 ) ) ;
#30861 = CARTESIAN_POINT ( 'NONE',  ( 1.999999999999998668, 15.80000000000000071, 26.53589838486224650 ) ) ;
#30862 = CARTESIAN_POINT ( 'NONE',  ( 6.009375000614519458, 0.000000000000000000, 5.243569643749999010 ) ) ;
#30863 = CARTESIAN_POINT ( 'NONE',  ( 17.05312500061451786, 4.541064518000418104, -2.621784821874998173 ) ) ;
#30864 = VERTEX_POINT ( 'NONE', #9373 ) ;
#30865 = CARTESIAN_POINT ( 'NONE',  ( 25.23750000000000071, -2.886751345948142422, -4.999999999999970690 ) ) ;
#30866 = CARTESIAN_POINT ( 'NONE',  ( 25.37812500061451715, -4.541064518000419881, 2.621784821874995952 ) ) ;
#30867 = CARTESIAN_POINT ( 'NONE',  ( 5.034375000614519813, 4.541064518000418104, 2.621784821874999949 ) ) ;
#30868 = FACE_OUTER_BOUND ( 'NONE', #4339, .T. ) ;
#30869 = CARTESIAN_POINT ( 'NONE',  ( 15.22500000000000142, -4.330127018922194537, 2.499999999999995559 ) ) ;
#30870 = CARTESIAN_POINT ( 'NONE',  ( 19.97812500061451502, -4.541064518000419881, 2.621784821874995952 ) ) ;
#30871 = ORIENTED_EDGE ( 'NONE', *, *, #29228, .F. ) ;
#30872 = CARTESIAN_POINT ( 'NONE',  ( 23.62500000000000000, 4.330127018922191873, 2.499999999999999556 ) ) ;
#30873 = CARTESIAN_POINT ( 'NONE',  ( 27.42187500061451644, 3.027376345333613106, -5.243569643749998122 ) ) ;
#30874 = ORIENTED_EDGE ( 'NONE', *, *, #13440, .F. ) ;
#30875 = CARTESIAN_POINT ( 'NONE',  ( 0.6945846161026939525, 20.50052346155192495, 33.93923243933046763 ) ) ;
#30876 = CARTESIAN_POINT ( 'NONE',  ( 13.79062500061451502, -3.027376345333610441, -5.243569643749999898 ) ) ;
#30877 = CARTESIAN_POINT ( 'NONE',  ( 25.01250000122903216, 4.330127018922192761, -2.499999999999997780 ) ) ;
#30878 = CARTESIAN_POINT ( 'NONE',  ( 16.95937500061451431, 2.746126346562645981, -4.756430356249997438 ) ) ;
#30879 = CARTESIAN_POINT ( 'NONE',  ( 2.934375000614518392, -4.541064518000419881, 2.621784821874995952 ) ) ;
#30880 = CARTESIAN_POINT ( 'NONE',  ( 12.71250000122903145, -4.330127018922190985, -2.500000000000001332 ) ) ;
#30881 = CARTESIAN_POINT ( 'NONE',  ( 18.63749999999999929, 5.773502691896255534, 3.535250795749688894E-16 ) ) ;
#30882 = CARTESIAN_POINT ( 'NONE',  ( 26.36249999999999716, 2.886751345948126879, 4.999999999999999112 ) ) ;
#30883 = CARTESIAN_POINT ( 'NONE',  ( 65.00000000000000000, 0.000000000000000000, 0.000000000000000000 ) ) ;
#30884 = CARTESIAN_POINT ( 'NONE',  ( 6.721875000614518925, 3.027376345333613106, -5.243569643749998122 ) ) ;
#30885 = CARTESIAN_POINT ( 'NONE',  ( 18.19687500061451502, -3.027376345333614438, 5.243569643749998122 ) ) ;
#30886 = DIRECTION ( 'NONE',  ( 0.000000000000000000, 0.000000000000000000, 1.000000000000000000 ) ) ;
#30887 = ORIENTED_EDGE ( 'NONE', *, *, #69324, .T. ) ;
#30888 = CARTESIAN_POINT ( 'NONE',  ( 29.01562500061451644, -6.054752690667223547, -1.112240025338166033E-15 ) ) ;
#30889 = CARTESIAN_POINT ( 'NONE',  ( 3.750000000000000000, 4.330127018922192761, -2.499999999999997780 ) ) ;
#30890 = CARTESIAN_POINT ( 'NONE',  ( 3.684375000614518836, 4.541064518000418104, 2.621784821874999949 ) ) ;
#30891 = CARTESIAN_POINT ( 'NONE',  ( 15.86250000000000249, 2.886751345948129099, -4.999999999999998224 ) ) ;
#30892 = CARTESIAN_POINT ( 'NONE',  ( 12.66562500061451502, 3.027376345333611329, 5.243569643749999010 ) ) ;
#30893 = CARTESIAN_POINT ( 'NONE',  ( 16.38749999999999929, 5.773502691896255534, 3.535250795749688401E-16 ) ) ;
#30894 = CARTESIAN_POINT ( 'NONE',  ( 5.000000000001397105, 0.3395091859857997107, -5.050874639569527424 ) ) ;
#30895 = CARTESIAN_POINT ( 'NONE',  ( 17.58750000122903145, -4.330127018922194537, 2.499999999999995559 ) ) ;
#30896 = CARTESIAN_POINT ( 'NONE',  ( -5.810221930991193690E-16, 13.25000000122903465, 26.00000000000000355 ) ) ;
#30897 = CARTESIAN_POINT ( 'NONE',  ( 18.64687500061451786, -2.746126346562646425, 4.756430356249996549 ) ) ;
#30898 = CARTESIAN_POINT ( 'NONE',  ( 6.928125000614516082, -4.541064518000419881, 2.621784821874995952 ) ) ;
#30899 = CARTESIAN_POINT ( 'NONE',  ( 23.59687500061451715, -3.027376345333614438, 5.243569643749998122 ) ) ;
#30901 = CARTESIAN_POINT ( 'NONE',  ( 4.243569643749999010, 17.87187500061451573, 27.54997392385601174 ) ) ;
#30900 =( BOUNDED_CURVE ( )  B_SPLINE_CURVE ( 2, ( #55038, #65017, #71667, #19940, #21042, #65379, #37312 ),
 .UNSPECIFIED., .F., .F. ) 
 B_SPLINE_CURVE_WITH_KNOTS ( ( 3, 2, 2, 3 ),
 ( 0.7100000000000001865, 0.7133333333333334858, 0.7166666666666667851, 0.7199999999999999734 ),
 .UNSPECIFIED. ) 
 CURVE ( )  GEOMETRIC_REPRESENTATION_ITEM ( )  RATIONAL_B_SPLINE_CURVE ( ( 0.9999999999999911182, 0.8660254037844475894, 1.000000000000000000, 0.8660254037844387076, 1.000000000000000000, 0.8660254037844387076, 1.000000000000000000 ) ) 
 REPRESENTATION_ITEM ( '' )  );
#30902 = CARTESIAN_POINT ( 'NONE',  ( 24.23437500061451644, 6.421520780324663323E-16, -5.243569643749999010 ) ) ;
#30903 = CARTESIAN_POINT ( 'NONE',  ( 5.137500000000000178, 5.773502691896255534, 3.535250795749688894E-16 ) ) ;
#30904 = CARTESIAN_POINT ( 'NONE',  ( -3.999999999999999112, 10.21250000122903501, 30.00000000000000000 ) ) ;
#30905 = CARTESIAN_POINT ( 'NONE',  ( 12.81562500061451537, -6.054752690667223547, -1.112240025338166033E-15 ) ) ;
#30906 = CARTESIAN_POINT ( 'NONE',  ( 4.575000001229033941, -5.773502691896255534, -1.060575238724906372E-15 ) ) ;
#30907 = EDGE_CURVE ( 'NONE', #32393, #6086, #59852, .T. ) ;
#30908 = CARTESIAN_POINT ( 'NONE',  ( 8.709375000614517859, 0.000000000000000000, 5.243569643749999010 ) ) ;
#30909 = CARTESIAN_POINT ( 'NONE',  ( 45.00000000000000000, 0.000000000000000000, 0.000000000000000000 ) ) ;
#30910 = ORIENTED_EDGE ( 'NONE', *, *, #69831, .F. ) ;
#30911 = CARTESIAN_POINT ( 'NONE',  ( 12.10312500061451857, 4.541064518000418104, -2.621784821874998173 ) ) ;
#30912 = FACE_OUTER_BOUND ( 'NONE', #52615, .T. ) ;
#30913 = CARTESIAN_POINT ( 'NONE',  ( 22.83750000122903501, 4.330127018922191873, 2.499999999999999556 ) ) ;
#30914 = CARTESIAN_POINT ( 'NONE',  ( 10.47187500061451715, 3.027376345333611329, 5.243569643749999010 ) ) ;
#30915 = CARTESIAN_POINT ( 'NONE',  ( 12.29062500061451857, -3.027376345333614438, 5.243569643749998122 ) ) ;
#30916 = CARTESIAN_POINT ( 'NONE',  ( 27.20625000122903359, 4.330127018922192761, -2.499999999999997780 ) ) ;
#30917 = CARTESIAN_POINT ( 'NONE',  ( 21.04687500061451644, -3.027376345333610441, -5.243569643749999898 ) ) ;
#30918 = CARTESIAN_POINT ( 'NONE',  ( 1.592000809091587073E-14, 15.95000000122903394, 26.00000000000000000 ) ) ;
#30919 = CARTESIAN_POINT ( 'NONE',  ( 7.724999999999999645, 6.123233995736764310E-16, -4.999999999999998224 ) ) ;
#30920 = CARTESIAN_POINT ( 'NONE',  ( 3.249167837762792832, 3.800382659950008790, -3.347690552023643296 ) ) ;
#30921 = CARTESIAN_POINT ( 'NONE',  ( 9.001249775931846008E-16, 14.57187500061451679, -25.09994784771203058 ) ) ;
#30922 = CARTESIAN_POINT ( 'NONE',  ( 15.87187500061451573, 3.027376345333611329, 5.243569643749999010 ) ) ;
#30923 = CARTESIAN_POINT ( 'NONE',  ( 18.15000000122903501, -2.886751345948125991, -5.000000000000000000 ) ) ;
#30924 = CARTESIAN_POINT ( 'NONE',  ( 11.59687500061451892, -3.027376345333610441, -5.243569643749999898 ) ) ;
#30925 = CARTESIAN_POINT ( 'NONE',  ( 4.243569643749999010, 18.71562500061451217, -32.45002607614398471 ) ) ;
#30926 = CARTESIAN_POINT ( 'NONE',  ( 16.98750000122903359, 4.330127018922191873, 2.499999999999999556 ) ) ;
#30927 = CARTESIAN_POINT ( 'NONE',  ( 11.99062500061451608, -3.027376345333610441, -5.243569643749999898 ) ) ;
#30928 = ORIENTED_EDGE ( 'NONE', *, *, #22319, .T. ) ;
#30929 = CARTESIAN_POINT ( 'NONE',  ( 15.93750000000000000, 5.773502691896255534, 3.535250795749688894E-16 ) ) ;
#30930 = CARTESIAN_POINT ( 'NONE',  ( 17.92500000000000071, -4.330127018922194537, 2.499999999999995559 ) ) ;
#30931 = CARTESIAN_POINT ( 'NONE',  ( 12.72187500061451537, 3.027376345333611329, 5.243569643749999010 ) ) ;
#30932 = DIRECTION ( 'NONE',  ( 1.000000000000000000, 0.000000000000000000, 0.000000000000000000 ) ) ;
#30933 = CARTESIAN_POINT ( 'NONE',  ( 13.16250000122903430, -4.330127018922190985, -2.500000000000001332 ) ) ;
#30934 = CARTESIAN_POINT ( 'NONE',  ( 21.45000000122903216, 5.773502691896255534, 3.535250795749688894E-16 ) ) ;
#30935 = CARTESIAN_POINT ( 'NONE',  ( 17.54062500061451502, 6.054752690667223547, 3.707466751127219781E-16 ) ) ;
#30936 = CARTESIAN_POINT ( 'NONE',  ( 19.94062500061451715, -3.027376345333614438, 5.243569643749998122 ) ) ;
#30937 = CARTESIAN_POINT ( 'NONE',  ( 27.37500000122903288, 2.886751345948126879, 4.999999999999999112 ) ) ;
#30938 = CARTESIAN_POINT ( 'NONE',  ( 25.19999999999999929, -4.330127018922190985, -2.500000000000001332 ) ) ;
#30939 = LINE ( 'NONE', #71200, #43052 ) ;
#30940 = CARTESIAN_POINT ( 'NONE',  ( 7.921875000614517326, -5.492252693125287522, -1.008910452111647106E-15 ) ) ;
#30941 = CARTESIAN_POINT ( 'NONE',  ( 27.87187500061451573, 3.027376345333613106, -5.243569643749998122 ) ) ;
#30942 = CARTESIAN_POINT ( 'NONE',  ( 4.038036497978814587, -2.948822205205740676, -4.128098832493389381 ) ) ;
#30943 = CARTESIAN_POINT ( 'NONE',  ( -4.243569643749999898, 14.42187500061451644, -32.45002607614398471 ) ) ;
#30944 = CARTESIAN_POINT ( 'NONE',  ( 3.187500001229033764, -4.330127018922194537, 2.499999999999995559 ) ) ;
#30945 = CARTESIAN_POINT ( 'NONE',  ( 6.487499999999999822, 5.773502691896255534, 3.535250795749688894E-16 ) ) ;
#30946 =( BOUNDED_CURVE ( )  B_SPLINE_CURVE ( 2, ( #46315, #62573, #11969, #40411, #22682, #34493, #534, #6427, #68486 ),
 .UNSPECIFIED., .F., .F. ) 
 B_SPLINE_CURVE_WITH_KNOTS ( ( 3, 2, 2, 2, 3 ),
 ( 0.2638888888888888951, 0.2685185185185185452, 0.2777777777777777901, 0.2870370370370370350, 0.2916666666666666852 ),
 .UNSPECIFIED. ) 
 CURVE ( )  GEOMETRIC_REPRESENTATION_ITEM ( )  RATIONAL_B_SPLINE_CURVE ( ( 0.9330127018922194093, 0.9330127018922194093, 1.000000000000000000, 0.8660254037844387076, 1.000000000000000000, 0.8660254037844387076, 1.000000000000000000, 0.9330127018922189652, 0.9330127018922194093 ) ) 
 REPRESENTATION_ITEM ( '' )  );
#30947 = EDGE_CURVE ( 'NONE', #68526, #14829, #1416, .T. ) ;
#30948 = CARTESIAN_POINT ( 'NONE',  ( 2.737500001229034474, -4.330127018922194537, 2.499999999999995559 ) ) ;
#30949 = CARTESIAN_POINT ( 'NONE',  ( 7.209375000614519635, 4.541064518000418104, -2.621784821874998173 ) ) ;
#30950 = VECTOR ( 'NONE', #24867, 1000.000000000000000 ) ;
#30951 = B_SPLINE_CURVE_WITH_KNOTS ( 'NONE', 3,
 ( #56797, #1038, #28730, #51271, #50909, #674, #61986, #23181, #29462, #51998, #11387, #45735, #1399, #45368, #68994, #40552, #51637, #6571, #62713, #18353, #12107, #63069, #63439, #40926, #35001, #33906, #58972, #8745, #3213, #2124, #52717, #25369, #30553, #24635, #25742, #53450, #70071, #48279, #47913, #2840 ),
 .UNSPECIFIED., .F., .F.,
 ( 4, 2, 2, 2, 2, 2, 2, 2, 2, 2, 2, 2, 2, 2, 2, 2, 2, 2, 2, 4 ),
 ( 0.02627519828802198087, 0.02668902850173000482, 0.02710285871543802530, 0.02793051914285407319, 0.02958583999768617245, 0.03041350042510221341, 0.03124116085251825783, 0.03206882127993430226, 0.03248265149364232274, 0.03289648170735034322, 0.03331031192105836369, 0.03372414213476638417, 0.03455180256218243207, 0.03537946298959847302, 0.03620712341701451398, 0.03703478384443055493, 0.03786244427184659589, 0.03869010469926264378, 0.03910393491297066426, 0.03951776512667868474 ),
 .UNSPECIFIED. ) ;
#30952 = CARTESIAN_POINT ( 'NONE',  ( 27.51562500061451644, 3.027376345333611329, 5.243569643749999010 ) ) ;
#30954 = EDGE_CURVE ( 'NONE', #38626, #71147, #26602, .T. ) ;
#30953 = DIRECTION ( 'NONE',  ( 0.000000000000000000, 0.000000000000000000, 1.000000000000000000 ) ) ;
#30955 = CARTESIAN_POINT ( 'NONE',  ( 22.57499999999999929, 6.123233995736764310E-16, -4.999999999999998224 ) ) ;
#30956 = DIRECTION ( 'NONE',  ( 0.000000000000000000, 0.000000000000000000, -1.000000000000000000 ) ) ;
#30957 = CARTESIAN_POINT ( 'NONE',  ( 5.334375000614517859, 6.421520780324663323E-16, -5.243569643749999010 ) ) ;
#30958 = CARTESIAN_POINT ( 'NONE',  ( 10.05937500061451750, 0.000000000000000000, 5.243569643749999010 ) ) ;
#30959 = CARTESIAN_POINT ( 'NONE',  ( 3.825000000000001954, 4.330127018922191873, 2.499999999999999556 ) ) ;
#30960 = CARTESIAN_POINT ( 'NONE',  ( 4.243569643749999898, 15.07812500061459460, 30.00000000000000000 ) ) ;
#30962 = EDGE_CURVE ( 'NONE', #66791, #54370, #26362, .T. ) ;
#30961 = CARTESIAN_POINT ( 'NONE',  ( 1.294081214890646203, 25.48735787228381255, 26.20605842228508564 ) ) ;
#30963 = CARTESIAN_POINT ( 'NONE',  ( 7.312500000000000000, 2.886751345948129099, -4.999999999999998224 ) ) ;
#30964 = CARTESIAN_POINT ( 'NONE',  ( 14.78437500061451537, 5.492252693125287522, 3.363034840372157021E-16 ) ) ;
#30965 = CARTESIAN_POINT ( 'NONE',  ( 20.20312500061451644, 4.541064518000418104, -2.621784821874998173 ) ) ;
#30966 = CARTESIAN_POINT ( 'NONE',  ( 10.11562500061451608, -6.054752690667223547, -1.112240025338166033E-15 ) ) ;
#30967 = CARTESIAN_POINT ( 'NONE',  ( 23.03437500061451360, -2.746126346562646425, 4.756430356249996549 ) ) ;
#30968 = CARTESIAN_POINT ( 'NONE',  ( 8.596875000614518925, 6.054752690667223547, 3.707466751127219781E-16 ) ) ;
#30969 = CARTESIAN_POINT ( 'NONE',  ( 25.57499999999999929, -4.330127018922194537, 2.499999999999995559 ) ) ;
#30970 = CARTESIAN_POINT ( 'NONE',  ( 19.16250000122903430, 4.330127018922192761, -2.499999999999997780 ) ) ;
#30971 = CARTESIAN_POINT ( 'NONE',  ( 26.95312500061451644, 4.541064518000418104, -2.621784821874998173 ) ) ;
#30972 = CARTESIAN_POINT ( 'NONE',  ( 24.00000000000000000, 4.330127018922192761, -2.499999999999997780 ) ) ;
#30973 = CARTESIAN_POINT ( 'NONE',  ( 10.05937500061451750, 0.000000000000000000, 5.243569643749999010 ) ) ;
#30974 = CARTESIAN_POINT ( 'NONE',  ( 13.77187500061451786, -6.054752690667223547, -1.112240025338166033E-15 ) ) ;
#30975 = CARTESIAN_POINT ( 'NONE',  ( 27.68437500061451573, -4.541064518000419881, 2.621784821874995952 ) ) ;
#30976 = EDGE_CURVE ( 'NONE', #10804, #65099, #57478, .T. ) ;
#30977 = CARTESIAN_POINT ( 'NONE',  ( 23.32499999999999929, -4.330127018922194537, 2.499999999999995559 ) ) ;
#30978 = CARTESIAN_POINT ( 'NONE',  ( 1.071796769724489895, 13.67990381179670045, -34.00000000000000000 ) ) ;
#30979 = CARTESIAN_POINT ( 'NONE',  ( 19.88437500061451857, 4.541064518000418104, 2.621784821874999949 ) ) ;
#30980 = CARTESIAN_POINT ( 'NONE',  ( 12.19687500061451679, 6.054752690667223547, 3.707466751127219781E-16 ) ) ;
#30981 = CARTESIAN_POINT ( 'NONE',  ( 2.655984681222220721E-16, 20.06562499938548427, 25.66244784525396483 ) ) ;
#30982 = CARTESIAN_POINT ( 'NONE',  ( 22.19999999999999574, 4.330127018922192761, -2.499999999999997780 ) ) ;
#30983 = CARTESIAN_POINT ( 'NONE',  ( -2.000000000000001776, 14.59999999999999964, 33.46410161513775705 ) ) ;
#30984 = CARTESIAN_POINT ( 'NONE',  ( -4.243569643749999898, 12.17187500061451999, -32.45002607614398471 ) ) ;
#30985 = CARTESIAN_POINT ( 'NONE',  ( 23.78437500061451360, 5.824947211148865298E-16, -4.756430356249998326 ) ) ;
#30986 = CARTESIAN_POINT ( 'NONE',  ( 15.29062500061451679, 6.054752690667223547, 3.707466751127219781E-16 ) ) ;
#30987 = CARTESIAN_POINT ( 'NONE',  ( 4.462500000000001243, -5.773502691896255534, -1.060575238724906372E-15 ) ) ;
#30988 = CARTESIAN_POINT ( 'NONE',  ( 6.900000001229033231, -2.886751345948193048, -4.999999999999883649 ) ) ;
#30989 = CARTESIAN_POINT ( 'NONE',  ( 25.53749999999999787, -2.886751345948114000, 5.000000000000024869 ) ) ;
#30990 = CARTESIAN_POINT ( 'NONE',  ( 12.26249999999999929, 2.886751345948129099, -4.999999999999998224 ) ) ;
#30991 = CARTESIAN_POINT ( 'NONE',  ( -3.999999999999999556, 18.27500000122903501, 27.69059892324149530 ) ) ;
#30992 = CARTESIAN_POINT ( 'NONE',  ( 12.63750000122903394, -4.330127018922194537, 2.499999999999995559 ) ) ;
#30993 = CARTESIAN_POINT ( 'NONE',  ( 25.32187500061451857, 3.027376345333611329, 5.243569643749999010 ) ) ;
#30994 = CARTESIAN_POINT ( 'NONE',  ( 17.74687500061451928, -3.027376345333614438, 5.243569643749998122 ) ) ;
#30995 = CARTESIAN_POINT ( 'NONE',  ( 25.21875000122903288, -5.773502691896255534, -1.060575238724906372E-15 ) ) ;
#30996 = ORIENTED_EDGE ( 'NONE', *, *, #60294, .T. ) ;
#30997 = CARTESIAN_POINT ( 'NONE',  ( 19.07812500061451644, -4.541064518000419881, 2.621784821874995952 ) ) ;
#30998 = CARTESIAN_POINT ( 'NONE',  ( 3.965625000614515727, 3.027376345333613106, -5.243569643749998122 ) ) ;
#30999 = CARTESIAN_POINT ( 'NONE',  ( 17.82187500061451502, -6.054752690667223547, -1.112240025338166033E-15 ) ) ;
#31000 = CARTESIAN_POINT ( 'NONE',  ( 28.43437500061451573, 4.541064518000418104, 2.621784821874999949 ) ) ;
#31001 = CARTESIAN_POINT ( 'NONE',  ( 5.315625000614516260, 3.027376345333613106, -5.243569643749998122 ) ) ;
#31002 = CARTESIAN_POINT ( 'NONE',  ( 19.22812500061451502, 6.421520780324663323E-16, -5.243569643749999010 ) ) ;
#31003 = CARTESIAN_POINT ( 'NONE',  ( 4.243569643749999898, 15.04062500061451679, 32.45002607614398471 ) ) ;
#31004 = CARTESIAN_POINT ( 'NONE',  ( 16.65000000122903501, -2.886751345948129988, 4.999999999999997335 ) ) ;
#31005 = CARTESIAN_POINT ( 'NONE',  ( 12.60937500061451821, 4.119189519843966529, -2.378215178124998275 ) ) ;
#31006 = CARTESIAN_POINT ( 'NONE',  ( 6.890625000614516438, -3.027376345333614438, 5.243569643749998122 ) ) ;
#31007 = CARTESIAN_POINT ( 'NONE',  ( 3.234375000614516438, 4.541064518000418104, 2.621784821874999949 ) ) ;
#31008 = CARTESIAN_POINT ( 'NONE',  ( 23.29687500061451644, -3.027376345333610441, -5.243569643749999898 ) ) ;
#31009 = CARTESIAN_POINT ( 'NONE',  ( 13.52812500061451750, 4.541064518000418104, 2.621784821874999949 ) ) ;
#31010 = CARTESIAN_POINT ( 'NONE',  ( 25.01250000122903216, 4.330127018922192761, -2.499999999999997780 ) ) ;
#31011 = CARTESIAN_POINT ( 'NONE',  ( 24.10312500061451502, -4.541064518000417216, -2.621784821875001281 ) ) ;
#31012 = CARTESIAN_POINT ( 'NONE',  ( 19.24687500061452283, -3.027376345333610441, -5.243569643749999898 ) ) ;
#31013 = CARTESIAN_POINT ( 'NONE',  ( 15.92812500061451608, -4.541064518000419881, 2.621784821874995952 ) ) ;
#31014 = CARTESIAN_POINT ( 'NONE',  ( -4.243569643749999898, 15.77187500061451608, 27.54997392385601529 ) ) ;
#31015 = CARTESIAN_POINT ( 'NONE',  ( 19.82812500061451644, 4.541064518000418104, 2.621784821874999949 ) ) ;
#31016 = CARTESIAN_POINT ( 'NONE',  ( -4.000000000000000888, 17.71249999999999858, 32.30940107675850470 ) ) ;
#31017 = VERTEX_POINT ( 'NONE', #72893 ) ;
#31018 = CARTESIAN_POINT ( 'NONE',  ( 21.86250000000000071, 2.886751345948126879, 4.999999999999999112 ) ) ;
#31019 = CARTESIAN_POINT ( 'NONE',  ( -2.828200636599751609E-16, 11.78749999999999964, -34.61880215351700230 ) ) ;
#31020 = CARTESIAN_POINT ( 'NONE',  ( 12.67499999999999893, 6.123233995736764310E-16, -4.999999999999998224 ) ) ;
#31021 = CARTESIAN_POINT ( 'NONE',  ( 26.76562500061451644, -6.054752690667223547, -1.112240025338166033E-15 ) ) ;
#31022 = CARTESIAN_POINT ( 'NONE',  ( 8.953125000614518214, 4.541064518000418104, -2.621784821874998173 ) ) ;
#31023 = CARTESIAN_POINT ( 'NONE',  ( 20.96250000122903145, 4.330127018922192761, -2.499999999999997780 ) ) ;
#31024 = CARTESIAN_POINT ( 'NONE',  ( 24.55312500061451786, -4.541064518000417216, -2.621784821875001281 ) ) ;
#31025 = CARTESIAN_POINT ( 'NONE',  ( 24.86250000000000071, 2.886751345948129099, -4.999999999999998224 ) ) ;
#31026 = CARTESIAN_POINT ( 'NONE',  ( 27.06562500061451004, 3.027376345333611329, 5.243569643749999010 ) ) ;
#31027 = CARTESIAN_POINT ( 'NONE',  ( 8.053125000614516082, 4.541064518000418104, -2.621784821874998173 ) ) ;
#31028 = ORIENTED_EDGE ( 'NONE', *, *, #48081, .F. ) ;
#31029 = CARTESIAN_POINT ( 'NONE',  ( 23.54062500061451146, -3.027376345333614438, 5.243569643749998122 ) ) ;
#31030 = CARTESIAN_POINT ( 'NONE',  ( 5.203125000614518214, -4.541064518000417216, -2.621784821875001281 ) ) ;
#31031 = CARTESIAN_POINT ( 'NONE',  ( 13.28437500061451715, -4.119189519843968306, 2.378215178124996054 ) ) ;
#31032 = CARTESIAN_POINT ( 'NONE',  ( 2.878125000614517592, -4.541064518000419881, 2.621784821874995952 ) ) ;
#31033 = CARTESIAN_POINT ( 'NONE',  ( -3.000416591977282496E-16, 19.74687500061451928, -34.90005215228797653 ) ) ;
#31034 = CARTESIAN_POINT ( 'NONE',  ( 12.75000000000000178, 4.330127018922192761, -2.499999999999997780 ) ) ;
#31035 = CARTESIAN_POINT ( 'NONE',  ( 14.70937500061451786, -4.541064518000417216, -2.621784821875001281 ) ) ;
#31036 = CARTESIAN_POINT ( 'NONE',  ( 8.250000001229034652, -2.886751345948125991, -5.000000000000000000 ) ) ;
#31037 = CARTESIAN_POINT ( 'NONE',  ( 15.68437500061451573, 6.421520780324663323E-16, -5.243569643749999010 ) ) ;
#31038 = CARTESIAN_POINT ( 'NONE',  ( 16.01249999999999929, 2.886751345948126879, 4.999999999999999112 ) ) ;
#31039 = CARTESIAN_POINT ( 'NONE',  ( 7.209375000614519635, 4.541064518000418104, -2.621784821874998173 ) ) ;
#31040 = CARTESIAN_POINT ( 'NONE',  ( -3.000416591977282496E-16, 12.04062500061451857, -34.90005215228797653 ) ) ;
#31041 = CARTESIAN_POINT ( 'NONE',  ( 24.63749999999999929, -2.886751345948143310, 4.999999999999972466 ) ) ;
#31042 = CARTESIAN_POINT ( 'NONE',  ( 13.09687500061451892, 6.054752690667223547, 3.707466751127219781E-16 ) ) ;
#31043 = ORIENTED_EDGE ( 'NONE', *, *, #58697, .F. ) ;
#31044 = CARTESIAN_POINT ( 'NONE',  ( 22.26562500061451644, -6.054752690667223547, -1.112240025338166033E-15 ) ) ;
#31045 = CARTESIAN_POINT ( 'NONE',  ( 2.121784821875001281, 10.10937500061451821, 33.67503911421598417 ) ) ;
#31046 = CARTESIAN_POINT ( 'NONE',  ( 26.62500000000000000, 6.123233995736764310E-16, -4.999999999999998224 ) ) ;
#31047 = CARTESIAN_POINT ( 'NONE',  ( 26.82187500061451857, -6.054752690667223547, -1.112240025338166033E-15 ) ) ;
#31048 = EDGE_CURVE ( 'NONE', #5287, #62948, #43851, .T. ) ;
#31049 = CARTESIAN_POINT ( 'NONE',  ( 29.25937500061451502, 4.541064518000418104, -2.621784821874998173 ) ) ;
#31050 = CARTESIAN_POINT ( 'NONE',  ( 4.115625000614516082, 3.027376345333611329, 5.243569643749999010 ) ) ;
#31051 = CARTESIAN_POINT ( 'NONE',  ( 22.99687500061451573, 0.000000000000000000, 4.756430356249998326 ) ) ;
#31052 = CARTESIAN_POINT ( 'NONE',  ( 17.14687500061451786, 6.054752690667223547, 3.707466751127219781E-16 ) ) ;
#31053 = CARTESIAN_POINT ( 'NONE',  ( 8.109375000614518214, 2.746126346562643317, 4.756430356249998326 ) ) ;
#31054 = CARTESIAN_POINT ( 'NONE',  ( 3.515625000614516882, 3.027376345333613106, -5.243569643749998122 ) ) ;
#31055 = CARTESIAN_POINT ( 'NONE',  ( 5.221875000614519813, -6.054752690667223547, -1.112240025338166033E-15 ) ) ;
#31056 = CARTESIAN_POINT ( 'NONE',  ( 17.40937500061451715, -4.541064518000417216, -2.621784821875001281 ) ) ;
#31057 = CARTESIAN_POINT ( 'NONE',  ( -3.870849190549275232, 25.03400442039527007, 31.04151046405775105 ) ) ;
#31058 = CARTESIAN_POINT ( 'NONE',  ( 25.31250000000000000, 2.886751345948129099, -4.999999999999998224 ) ) ;
#31059 = CARTESIAN_POINT ( 'NONE',  ( 26.44687500061451502, -3.027376345333610441, -5.243569643749999898 ) ) ;
#31060 = FACE_OUTER_BOUND ( 'NONE', #30629, .T. ) ;
#31061 = CARTESIAN_POINT ( 'NONE',  ( 8.793750001229033941, 5.773502691896255534, 3.535250795749688401E-16 ) ) ;
#31062 = EDGE_LOOP ( 'NONE', ( #47745, #42971, #49479, #56614 ) ) ;
#31063 = CARTESIAN_POINT ( 'NONE',  ( 7.387500000000001066, 5.773502691896255534, 3.535250795749688894E-16 ) ) ;
#31064 = CARTESIAN_POINT ( 'NONE',  ( 8.896875000614517859, 4.119189519843966529, -2.378215178124998275 ) ) ;
#31065 = CARTESIAN_POINT ( 'NONE',  ( 22.19062500061451715, -3.027376345333614438, 5.243569643749998122 ) ) ;
#31066 = CARTESIAN_POINT ( 'NONE',  ( 12.30000000000000249, 4.330127018922192761, -2.499999999999997780 ) ) ;
#31067 = CARTESIAN_POINT ( 'NONE',  ( 8.925000001229033586, 2.886751345948126879, 4.999999999999999112 ) ) ;
#31068 = CARTESIAN_POINT ( 'NONE',  ( 6.703125000614516438, 4.541064518000418104, -2.621784821874998173 ) ) ;
#31069 = CARTESIAN_POINT ( 'NONE',  ( 21.03750000000000142, -2.886751345948129988, 4.999999999999997335 ) ) ;
#31070 = CARTESIAN_POINT ( 'NONE',  ( 18.06562500061451715, 3.027376345333611329, 5.243569643749999010 ) ) ;
#31071 = CARTESIAN_POINT ( 'NONE',  ( 7.556250001229035007, 0.000000000000000000, 4.999999999999998224 ) ) ;
#31072 = CARTESIAN_POINT ( 'NONE',  ( 22.46250000122903501, 0.000000000000000000, 4.999999999999998224 ) ) ;
#31073 = CARTESIAN_POINT ( 'NONE',  ( -1.878215178124999163, 19.09062499938548285, 26.74683588394047007 ) ) ;
#31074 = CARTESIAN_POINT ( 'NONE',  ( 4.687500000000000000, 5.773502691896255534, 3.535250795749688894E-16 ) ) ;
#31075 = EDGE_LOOP ( 'NONE', ( #19978, #67792, #22346, #25762 ) ) ;
#31076 = CARTESIAN_POINT ( 'NONE',  ( 19.30312500061451786, 4.541064518000418104, -2.621784821874998173 ) ) ;
#31077 = CARTESIAN_POINT ( 'NONE',  ( 26.12812500061451360, 4.541064518000418104, 2.621784821874999949 ) ) ;
#31078 = CARTESIAN_POINT ( 'NONE',  ( 24.75937500061451502, 4.541064518000418104, -2.621784821874998173 ) ) ;
#31079 = CARTESIAN_POINT ( 'NONE',  ( 8.812500000000000000, 2.886751345948126879, 4.999999999999999112 ) ) ;
#31080 = CARTESIAN_POINT ( 'NONE',  ( 12.77812500061451750, -4.541064518000419881, 2.621784821874995952 ) ) ;
#31081 = CARTESIAN_POINT ( 'NONE',  ( 27.92812500061451431, 4.541064518000418104, 2.621784821874999949 ) ) ;
#31082 = CARTESIAN_POINT ( 'NONE',  ( 9.665625000614515017, -6.054752690667223547, -1.112240025338166033E-15 ) ) ;
#31083 = CARTESIAN_POINT ( 'NONE',  ( 22.87500000000000000, -4.330127018922194537, 2.499999999999995559 ) ) ;
#31084 = CARTESIAN_POINT ( 'NONE',  ( -2.121784821874999949, 12.58437500061451786, 26.32496088578401938 ) ) ;
#31085 = EDGE_CURVE ( 'NONE', #5008, #32129, #67901, .T. ) ;
#31086 = CARTESIAN_POINT ( 'NONE',  ( 24.60000000122903430, 5.773502691896255534, 3.535250795749688894E-16 ) ) ;
#31087 = CARTESIAN_POINT ( 'NONE',  ( 18.64687500061451786, -2.746126346562646425, 4.756430356249996549 ) ) ;
#31088 = CARTESIAN_POINT ( 'NONE',  ( 13.34062500061451750, -3.027376345333610441, -5.243569643749999898 ) ) ;
#31089 = CARTESIAN_POINT ( 'NONE',  ( 11.48437500061451644, -4.541064518000419881, 2.621784821874995952 ) ) ;
#31090 = CARTESIAN_POINT ( 'NONE',  ( 8.596875000614518925, 6.054752690667223547, 3.707466751127219781E-16 ) ) ;
#31091 = CARTESIAN_POINT ( 'NONE',  ( 17.14687500061451786, 6.054752690667223547, 3.707466751127219781E-16 ) ) ;
#31092 = ORIENTED_EDGE ( 'NONE', *, *, #10308, .F. ) ;
#31093 = CARTESIAN_POINT ( 'NONE',  ( 0.000000000000000000, 12.50000000000000000, 26.00000000000000000 ) ) ;
#31094 = CARTESIAN_POINT ( 'NONE',  ( 21.74062500061451431, -3.027376345333614438, 5.243569643749998122 ) ) ;
#31095 = CARTESIAN_POINT ( 'NONE',  ( 17.07187500061451502, 3.027376345333613106, -5.243569643749998122 ) ) ;
#31096 = CARTESIAN_POINT ( 'NONE',  ( 20.87812500061451715, -4.541064518000419881, 2.621784821874995952 ) ) ;
#31097 = CARTESIAN_POINT ( 'NONE',  ( 3.999999999999998668, 11.71250000000000036, 27.69059892324149175 ) ) ;
#31098 = CARTESIAN_POINT ( 'NONE',  ( 26.54062500061451146, 6.054752690667223547, 3.707466751127219781E-16 ) ) ;
#31099 = CARTESIAN_POINT ( 'NONE',  ( 6.712500001229034119, 0.000000000000000000, 4.999999999999998224 ) ) ;
#31100 = ORIENTED_EDGE ( 'NONE', *, *, #26717, .F. ) ;
#31101 = CARTESIAN_POINT ( 'NONE',  ( 5.100000001229034297, -2.886751345948125991, -5.000000000000000000 ) ) ;
#31102 = CARTESIAN_POINT ( 'NONE',  ( 3.999999999999999112, 17.97500000000000142, -30.00000000000000000 ) ) ;
#31103 = CARTESIAN_POINT ( 'NONE',  ( 25.20000000122903216, -2.886751345948129988, 4.999999999999997335 ) ) ;
#31104 = CARTESIAN_POINT ( 'NONE',  ( 1.878215178125000495, 15.07812499938548179, 26.74683588394047007 ) ) ;
#31105 = CARTESIAN_POINT ( 'NONE',  ( 7.471875000614519813, -6.054752690667223547, -1.112240025338166033E-15 ) ) ;
#31106 = CARTESIAN_POINT ( 'NONE',  ( 4.897546610576117843, 1.006994139586731674, -5.145967878999484491 ) ) ;
#31107 = ADVANCED_FACE ( 'NONE', ( #16724 ), #1841, .T. ) ;
#31108 = CARTESIAN_POINT ( 'NONE',  ( 15.02812500061451750, -4.541064518000419881, 2.621784821874995952 ) ) ;
#31109 = CARTESIAN_POINT ( 'NONE',  ( 8.559375000614515727, 4.541064518000418104, -2.621784821874998173 ) ) ;
#31110 = CARTESIAN_POINT ( 'NONE',  ( 26.70000000122903572, -2.886751345948125991, -5.000000000000000000 ) ) ;
#31111 = CARTESIAN_POINT ( 'NONE',  ( 16.80937500061451573, 0.000000000000000000, 5.243569643749999010 ) ) ;
#31112 = CARTESIAN_POINT ( 'NONE',  ( 3.946875000614517681, -3.027376345333610441, -5.243569643749999898 ) ) ;
#31113 = FACE_OUTER_BOUND ( 'NONE', #22272, .T. ) ;
#31114 =( BOUNDED_CURVE ( )  B_SPLINE_CURVE ( 2, ( #4, #22511, #16961, #39514, #62042, #33955, #56495, #62020, #5872 ),
 .UNSPECIFIED., .F., .F. ) 
 B_SPLINE_CURVE_WITH_KNOTS ( ( 3, 2, 2, 2, 3 ),
 ( 0.5326086956521739468, 0.5362318840579710644, 0.5434782608695651884, 0.5507246376811594235, 0.5543478260869565410 ),
 .UNSPECIFIED. ) 
 CURVE ( )  GEOMETRIC_REPRESENTATION_ITEM ( )  RATIONAL_B_SPLINE_CURVE ( ( 0.9330127018922194093, 0.9330127018922194093, 1.000000000000000000, 0.8660254037844387076, 1.000000000000000000, 0.8660254037844387076, 1.000000000000000000, 0.9330127018922194093, 0.9330127018922194093 ) ) 
 REPRESENTATION_ITEM ( '' )  );
#31115 = CARTESIAN_POINT ( 'NONE',  ( 4.940625000614515372, 6.054752690667223547, 3.707466751127219781E-16 ) ) ;
#31116 = CARTESIAN_POINT ( 'NONE',  ( 15.36562500061451608, 3.027376345333611329, 5.243569643749999010 ) ) ;
#31117 = ORIENTED_EDGE ( 'NONE', *, *, #56957, .T. ) ;
#31118 = CARTESIAN_POINT ( 'NONE',  ( 13.07812500061451821, 4.541064518000418104, 2.621784821874999949 ) ) ;
#31119 = CARTESIAN_POINT ( 'NONE',  ( 5.250000001229035540, 5.773502691896255534, 3.535250795749688894E-16 ) ) ;
#31120 = CARTESIAN_POINT ( 'NONE',  ( 11.95312500061451644, -4.541064518000417216, -2.621784821875001281 ) ) ;
#31121 = CARTESIAN_POINT ( 'NONE',  ( 20.97187500061451715, -5.492252693125287522, -1.008910452111647106E-15 ) ) ;
#31122 = CARTESIAN_POINT ( 'NONE',  ( 10.23750000000000071, -2.886751345948129988, 4.999999999999997335 ) ) ;
#31123 = CARTESIAN_POINT ( 'NONE',  ( 6.225000001229036073, 2.886751345948126879, 4.999999999999999112 ) ) ;
#31124 = CARTESIAN_POINT ( 'NONE',  ( 19.23749999999999716, -2.886751345948129988, 4.999999999999997335 ) ) ;
#31125 = CARTESIAN_POINT ( 'NONE',  ( 15.15937500061451715, -4.541064518000417216, -2.621784821875001281 ) ) ;
#31126 = CARTESIAN_POINT ( 'NONE',  ( 17.02500000122903145, 2.886751345948126879, 4.999999999999999112 ) ) ;
#31127 = CARTESIAN_POINT ( 'NONE',  ( 22.16250000000000142, 2.886751345948129099, -4.999999999999998224 ) ) ;
#31128 = CARTESIAN_POINT ( 'NONE',  ( -2.121784821874996840, 19.42812500061451786, -26.32496088578401583 ) ) ;
#31129 = CARTESIAN_POINT ( 'NONE',  ( 3.211236255978536125, 3.832487665771286522, 3.578695418803822470 ) ) ;
#31130 = CARTESIAN_POINT ( 'NONE',  ( 3.999999999999998668, 16.00624999877096499, 32.30940107675850470 ) ) ;
#31131 = LINE ( 'NONE', #47761, #38295 ) ;
#31132 = CARTESIAN_POINT ( 'NONE',  ( 11.90625000122903465, 4.330127018922192761, -2.499999999999997780 ) ) ;
#31133 = CARTESIAN_POINT ( 'NONE',  ( -3.486133158594716510E-16, 13.00624999877096855, 26.00000000000000355 ) ) ;
#31134 = CARTESIAN_POINT ( 'NONE',  ( 15.00937500061451679, 0.000000000000000000, 5.243569643749999010 ) ) ;
#31135 = CARTESIAN_POINT ( 'NONE',  ( 29.55000000000000071, 0.000000000000000000, 4.999999999999998224 ) ) ;
#31136 = CARTESIAN_POINT ( 'NONE',  ( 11.84062500061451750, -3.027376345333614438, 5.243569643749998122 ) ) ;
#31137 = CARTESIAN_POINT ( 'NONE',  ( 7.968750001229034652, 2.886751345948126879, 4.999999999999999112 ) ) ;
#31138 = CARTESIAN_POINT ( 'NONE',  ( 23.14687500061451786, -3.027376345333614438, 5.243569643749998122 ) ) ;
#31139 = CARTESIAN_POINT ( 'NONE',  ( 16.77187500061451431, -4.119189519843968306, 2.378215178124996054 ) ) ;
#31140 = CARTESIAN_POINT ( 'NONE',  ( 11.05312500061451608, -4.541064518000417216, -2.621784821875001281 ) ) ;
#31141 = CARTESIAN_POINT ( 'NONE',  ( 14.10937500061451644, 0.000000000000000000, 5.243569643749999010 ) ) ;
#31142 = ORIENTED_EDGE ( 'NONE', *, *, #34302, .T. ) ;
#31143 = CARTESIAN_POINT ( 'NONE',  ( 24.57187500061451502, -6.054752690667223547, -1.112240025338166033E-15 ) ) ;
#31144 = CARTESIAN_POINT ( 'NONE',  ( 27.21562500061451928, -6.054752690667223547, -1.112240025338166033E-15 ) ) ;
#31145 = CARTESIAN_POINT ( 'NONE',  ( 28.64999999999999858, 0.000000000000000000, 4.999999999999998224 ) ) ;
#31146 =( BOUNDED_CURVE ( )  B_SPLINE_CURVE ( 2, ( #1858, #41725, #8113, #52452, #46548, #2569, #25089 ),
 .UNSPECIFIED., .F., .F. ) 
 B_SPLINE_CURVE_WITH_KNOTS ( ( 3, 2, 2, 3 ),
 ( 0.5999999999999999778, 0.6027777777777777457, 0.6055555555555555136, 0.6083333333333332815 ),
 .UNSPECIFIED. ) 
 CURVE ( )  GEOMETRIC_REPRESENTATION_ITEM ( )  RATIONAL_B_SPLINE_CURVE ( ( 1.000000000000000000, 0.8660254037844387076, 1.000000000000000000, 0.8660254037844387076, 1.000000000000000000, 0.8660254037844387076, 1.000000000000000000 ) ) 
 REPRESENTATION_ITEM ( '' )  );
#31147 = CARTESIAN_POINT ( 'NONE',  ( 7.200000000000001954, -4.330127018922190985, -2.500000000000001332 ) ) ;
#31148 = CARTESIAN_POINT ( 'NONE',  ( 16.80000000122903359, -2.886751345948125991, -5.000000000000000000 ) ) ;
#31149 = PLANE ( 'NONE',  #61989 ) ;
#31150 = CARTESIAN_POINT ( 'NONE',  ( 7.734375000614518214, -2.746126346562646425, 4.756430356249996549 ) ) ;
#31151 = ORIENTED_EDGE ( 'NONE', *, *, #40764, .T. ) ;
#31152 = CARTESIAN_POINT ( 'NONE',  ( 16.23750000000000071, -2.886751345948125991, -5.000000000000000000 ) ) ;
#31153 = CARTESIAN_POINT ( 'NONE',  ( 18.78749999999999432, -2.886751345948129988, 4.999999999999997335 ) ) ;
#31154 = CARTESIAN_POINT ( 'NONE',  ( 13.04062500061451502, 6.054752690667223547, 3.707466751127219781E-16 ) ) ;
#31155 = ORIENTED_EDGE ( 'NONE', *, *, #18371, .T. ) ;
#31156 = LINE ( 'NONE', #3091, #11251 ) ;
#31157 = CARTESIAN_POINT ( 'NONE',  ( -2.121784821874999949, 16.63437500061451857, -33.67503911421598417 ) ) ;
#31158 = CARTESIAN_POINT ( 'NONE',  ( 6.478125000614516793, -4.541064518000419881, 2.621784821874995952 ) ) ;
#31159 = CARTESIAN_POINT ( 'NONE',  ( 3.756430356250000546, 13.12812499938548427, 27.83122392262697886 ) ) ;
#31160 = CARTESIAN_POINT ( 'NONE',  ( 13.27500000000000213, 4.330127018922191873, 2.499999999999999556 ) ) ;
#31161 = CARTESIAN_POINT ( 'NONE',  ( 28.09687500061451715, -4.119189519843965641, -2.378215178125001383 ) ) ;
#31162 = ORIENTED_EDGE ( 'NONE', *, *, #62210, .F. ) ;
#31163 = CARTESIAN_POINT ( 'NONE',  ( -4.243569643749999898, 16.20312500061451644, 30.00000000000000000 ) ) ;
#31164 = CARTESIAN_POINT ( 'NONE',  ( 27.89062500061451289, 6.054752690667223547, 3.707466751127219781E-16 ) ) ;
#31165 = CARTESIAN_POINT ( 'NONE',  ( 8.962500000000002132, -5.773502691896255534, -1.060575238724906372E-15 ) ) ;
#31166 = CARTESIAN_POINT ( 'NONE',  ( 1.878215178124997609, 18.41562499938548214, 33.25316411605952993 ) ) ;
#31167 = CARTESIAN_POINT ( 'NONE',  ( 24.23437500061451644, 6.421520780324663323E-16, -5.243569643749999010 ) ) ;
#31168 = CARTESIAN_POINT ( 'NONE',  ( 18.14062500061451644, -3.027376345333614438, 5.243569643749998122 ) ) ;
#31169 = CARTESIAN_POINT ( 'NONE',  ( -4.243569643749998122, 13.54062500061459140, -27.54997392385601174 ) ) ;
#31170 = CARTESIAN_POINT ( 'NONE',  ( 23.81250000122903288, 0.000000000000000000, 4.999999999999998224 ) ) ;
#31171 = CARTESIAN_POINT ( 'NONE',  ( 4.678125000614516971, -4.541064518000419881, 2.621784821874995952 ) ) ;
#31172 = CARTESIAN_POINT ( 'NONE',  ( 26.82187500061451857, -5.492252693125287522, -1.008910452111647106E-15 ) ) ;
#31173 = CARTESIAN_POINT ( 'NONE',  ( 21.70312500061451644, 0.000000000000000000, 5.243569643749999010 ) ) ;
#31174 = CARTESIAN_POINT ( 'NONE',  ( 9.909375000614517148, 4.119189519843966529, -2.378215178124998275 ) ) ;
#31175 = CARTESIAN_POINT ( 'NONE',  ( 1.878215178124997609, 16.16562499938548569, 33.25316411605952993 ) ) ;
#31176 = CARTESIAN_POINT ( 'NONE',  ( 18.42187500061451644, 3.027376345333613106, -5.243569643749998122 ) ) ;
#31177 = CARTESIAN_POINT ( 'NONE',  ( 15.98437500061451821, -4.541064518000419881, 2.621784821874995952 ) ) ;
#31178 = CARTESIAN_POINT ( 'NONE',  ( 23.97187500061451360, 3.027376345333611329, 5.243569643749999010 ) ) ;
#31179 = CARTESIAN_POINT ( 'NONE',  ( -4.243569643749998122, 13.14687500061451786, 32.45002607614398471 ) ) ;
#31180 = CARTESIAN_POINT ( 'NONE',  ( 4.415625000614518569, 3.027376345333613106, -5.243569643749998122 ) ) ;
#31181 = FACE_OUTER_BOUND ( 'NONE', #34868, .T. ) ;
#31182 =( BOUNDED_CURVE ( )  B_SPLINE_CURVE ( 2, ( #70968, #37351, #20341, #42894, #59873, #9278, #31812, #3744, #48806 ),
 .UNSPECIFIED., .F., .F. ) 
 B_SPLINE_CURVE_WITH_KNOTS ( ( 3, 2, 2, 2, 3 ),
 ( 0.07608695652173913526, 0.07971014492753622505, 0.08695652173913043237, 0.09420289855072463969, 0.09782608695652174335 ),
 .UNSPECIFIED. ) 
 CURVE ( )  GEOMETRIC_REPRESENTATION_ITEM ( )  RATIONAL_B_SPLINE_CURVE ( ( 0.9330127018922192983, 0.9330127018922194093, 1.000000000000000000, 0.8660254037844387076, 1.000000000000000000, 0.8660254037844387076, 1.000000000000000000, 0.9330127018922194093, 0.9330127018922194093 ) ) 
 REPRESENTATION_ITEM ( '' )  );
#31183 = CARTESIAN_POINT ( 'NONE',  ( 28.90312500061451217, 0.000000000000000000, 5.243569643749999010 ) ) ;
#31184 = FACE_OUTER_BOUND ( 'NONE', #61447, .T. ) ;
#31185 = CARTESIAN_POINT ( 'NONE',  ( 1.071796769724505438, 12.77990381179669832, 26.00000000000001421 ) ) ;
#31186 = CARTESIAN_POINT ( 'NONE',  ( 3.853125000614517681, -4.541064518000417216, -2.621784821875001281 ) ) ;
#31187 = CARTESIAN_POINT ( 'NONE',  ( 7.546875000614517326, -3.027376345333610441, -5.243569643749999898 ) ) ;
#31188 = SHAPE_DEFINITION_REPRESENTATION ( #34355, #33485 ) ;
#31189 = CARTESIAN_POINT ( 'NONE',  ( 15.15000000122903323, 5.773502691896255534, 3.535250795749688894E-16 ) ) ;
#31190 = CARTESIAN_POINT ( 'NONE',  ( 3.534375000614518036, 6.421520780324663323E-16, -5.243569643749999010 ) ) ;
#31191 = CARTESIAN_POINT ( 'NONE',  ( 11.85000000122903430, -2.886751345948125991, -5.000000000000000000 ) ) ;
#31192 = CARTESIAN_POINT ( 'NONE',  ( 4.640625000614518214, -3.027376345333614438, 5.243569643749998122 ) ) ;
#31193 = CARTESIAN_POINT ( 'NONE',  ( -2.000000000000001776, 14.09374999877096535, 33.46410161513775705 ) ) ;
#31194 = CARTESIAN_POINT ( 'NONE',  ( 20.15625000122903288, 0.000000000000000000, 4.999999999999998224 ) ) ;
#31195 = CARTESIAN_POINT ( 'NONE',  ( 13.20937500061451786, 0.000000000000000000, 5.243569643749999010 ) ) ;
#31196 = DIRECTION ( 'NONE',  ( 0.000000000000000000, 0.000000000000000000, -1.000000000000000000 ) ) ;
#31197 = VERTEX_POINT ( 'NONE', #37696 ) ;
#31198 = CARTESIAN_POINT ( 'NONE',  ( 22.60312500061451857, 0.000000000000000000, 5.243569643749999010 ) ) ;
#31199 = CARTESIAN_POINT ( 'NONE',  ( 7.378125000614518036, -4.541064518000419881, 2.621784821874995952 ) ) ;
#31200 = CARTESIAN_POINT ( 'NONE',  ( 25.58437500061451431, 6.421520780324663323E-16, -5.243569643749999010 ) ) ;
#31201 = CARTESIAN_POINT ( 'NONE',  ( 7.190625000614518036, 6.054752690667223547, 3.707466751127219781E-16 ) ) ;
#31202 = CYLINDRICAL_SURFACE ( 'NONE', #51011, 4.999999999999998224 ) ;
#31203 = CARTESIAN_POINT ( 'NONE',  ( 8.250000001229034652, -2.886751345948125991, -5.000000000000000000 ) ) ;
#31204 = CARTESIAN_POINT ( 'NONE',  ( 23.76562500061451644, 3.027376345333613106, -5.243569643749998122 ) ) ;
#31205 = CARTESIAN_POINT ( 'NONE',  ( 9.001249775931846008E-16, 11.36562500061451786, -25.09994784771203058 ) ) ;
#31206 = CARTESIAN_POINT ( 'NONE',  ( 9.900000001229033231, -2.886751345948129988, 4.999999999999997335 ) ) ;
#31207 =( BOUNDED_CURVE ( )  B_SPLINE_CURVE ( 2, ( #45129, #11141, #38494, #10417, #32948, #55125, #33670 ),
 .UNSPECIFIED., .F., .F. ) 
 B_SPLINE_CURVE_WITH_KNOTS ( ( 3, 2, 2, 3 ),
 ( 0.6900000000000000577, 0.6933333333333334680, 0.6966666666666668783, 0.7000000000000001776 ),
 .UNSPECIFIED. ) 
 CURVE ( )  GEOMETRIC_REPRESENTATION_ITEM ( )  RATIONAL_B_SPLINE_CURVE ( ( 0.9999999999999955591, 0.8660254037844431485, 1.000000000000000000, 0.8660254037844387076, 1.000000000000000000, 0.8660254037844298258, 1.000000000000008882 ) ) 
 REPRESENTATION_ITEM ( '' )  );
#31208 = CARTESIAN_POINT ( 'NONE',  ( 19.82812500061451644, 4.541064518000418104, 2.621784821874999949 ) ) ;
#31209 = CARTESIAN_POINT ( 'NONE',  ( 17.20312500061451644, 0.000000000000000000, 5.243569643749999010 ) ) ;
#31210 = CARTESIAN_POINT ( 'NONE',  ( 27.72187500061451715, -5.492252693125287522, -1.008910452111647106E-15 ) ) ;
#31211 = CARTESIAN_POINT ( 'NONE',  ( 18.78749999999999432, -2.886751345948129988, 4.999999999999997335 ) ) ;
#31212 = CARTESIAN_POINT ( 'NONE',  ( 12.78750000122903430, 6.123233995736764310E-16, -4.999999999999998224 ) ) ;
#31213 = CARTESIAN_POINT ( 'NONE',  ( 9.478125000614515017, 4.541064518000418104, 2.621784821874999949 ) ) ;
#31214 = CARTESIAN_POINT ( 'NONE',  ( 14.61562500061451608, -6.054752690667223547, -1.112240025338166033E-15 ) ) ;
#31215 = CARTESIAN_POINT ( 'NONE',  ( 22.46250000122903501, 0.000000000000000000, 4.999999999999998224 ) ) ;
#31216 = CARTESIAN_POINT ( 'NONE',  ( 22.58437500061451431, 4.541064518000418104, 2.621784821874999949 ) ) ;
#31217 = CARTESIAN_POINT ( 'NONE',  ( 20.85937500061451644, 0.000000000000000000, 5.243569643749999010 ) ) ;
#31218 = CARTESIAN_POINT ( 'NONE',  ( -3.999999999999999112, 18.53749999999999432, 27.69059892324149530 ) ) ;
#31219 = CARTESIAN_POINT ( 'NONE',  ( 7.200000001229035718, -2.886751345948129988, 4.999999999999997335 ) ) ;
#31220 = CARTESIAN_POINT ( 'NONE',  ( 6.384375000614516793, 4.541064518000418104, 2.621784821874999949 ) ) ;
#31221 = CARTESIAN_POINT ( 'NONE',  ( 23.48437500061451644, 4.541064518000418104, 2.621784821874999949 ) ) ;
#31222 = EDGE_CURVE ( 'NONE', #3749, #6439, #31596, .T. ) ;
#31223 = VECTOR ( 'NONE', #47978, 1000.000000000000000 ) ;
#31224 = CARTESIAN_POINT ( 'NONE',  ( 19.34062500061451573, 6.054752690667223547, 3.707466751127219781E-16 ) ) ;
#31225 = CARTESIAN_POINT ( 'NONE',  ( 23.70937500061451786, -4.541064518000417216, -2.621784821875001281 ) ) ;
#31226 = CARTESIAN_POINT ( 'NONE',  ( 1.878215178124997609, 18.52812499938548285, 33.25316411605952993 ) ) ;
#31227 = LINE ( 'NONE', #26795, #31493 ) ;
#31228 = CARTESIAN_POINT ( 'NONE',  ( 16.44375000122903074, 5.773502691896255534, 3.535250795749688401E-16 ) ) ;
#31229 = CARTESIAN_POINT ( 'NONE',  ( 6.271875000614517859, 3.027376345333613106, -5.243569643749998122 ) ) ;
#31230 = CARTESIAN_POINT ( 'NONE',  ( 17.39062500061451644, -3.027376345333610441, -5.243569643749999898 ) ) ;
#31231 = VECTOR ( 'NONE', #15869, 1000.000000000000000 ) ;
#31232 = ORIENTED_EDGE ( 'NONE', *, *, #19011, .T. ) ;
#31233 = FACE_OUTER_BOUND ( 'NONE', #21159, .T. ) ;
#31234 = CARTESIAN_POINT ( 'NONE',  ( 25.34062500061451217, -3.027376345333614438, 5.243569643749998122 ) ) ;
#31235 = CYLINDRICAL_SURFACE ( 'NONE', #2637, 4.000000000000000000 ) ;
#31236 = CARTESIAN_POINT ( 'NONE',  ( -2.498395430326213790E-14, 17.05624999877096926, 26.00000000000000000 ) ) ;
#31237 = CARTESIAN_POINT ( 'NONE',  ( 15.29999999999999893, -4.330127018922190985, -2.500000000000001332 ) ) ;
#31238 = CARTESIAN_POINT ( 'NONE',  ( 25.12500000122903288, 2.886751345948126879, 4.999999999999999112 ) ) ;
#31239 = CARTESIAN_POINT ( 'NONE',  ( 18.51562500061451289, 3.027376345333611329, 5.243569643749999010 ) ) ;
#31240 = EDGE_LOOP ( 'NONE', ( #25487, #34140, #7533, #60770 ) ) ;
#31241 = CARTESIAN_POINT ( 'NONE',  ( 22.05000000000000071, -4.330127018922190985, -2.500000000000001332 ) ) ;
#31242 = CARTESIAN_POINT ( 'NONE',  ( 24.72187500061451360, 3.027376345333613106, -5.243569643749998122 ) ) ;
#31243 = VERTEX_POINT ( 'NONE', #44721 ) ;
#31244 = DIRECTION ( 'NONE',  ( -1.000000000000000000, -0.000000000000000000, -0.000000000000000000 ) ) ;
#31245 = CARTESIAN_POINT ( 'NONE',  ( 12.74062500061451786, -3.027376345333614438, 5.243569643749998122 ) ) ;
#31246 = CARTESIAN_POINT ( 'NONE',  ( 3.403125000614518836, -4.541064518000417216, -2.621784821875001281 ) ) ;
#31247 = CARTESIAN_POINT ( 'NONE',  ( 17.18437500061451573, -2.746126346562646425, 4.756430356249996549 ) ) ;
#31248 = CARTESIAN_POINT ( 'NONE',  ( 26.20312500061451644, 0.000000000000000000, 5.243569643749999010 ) ) ;
#31249 = CARTESIAN_POINT ( 'NONE',  ( 11.92500000122903181, 2.886751345948129099, -4.999999999999998224 ) ) ;
#31250 = CARTESIAN_POINT ( 'NONE',  ( 19.98749999999999716, 5.773502691896255534, 3.535250795749688894E-16 ) ) ;
#31251 = CARTESIAN_POINT ( 'NONE',  ( 27.67499999999999716, 4.330127018922191873, 2.499999999999999556 ) ) ;
#31252 = CARTESIAN_POINT ( 'NONE',  ( 4.648177544792955741E-15, 14.13124999877096322, 33.99999999999999289 ) ) ;
#31253 = CARTESIAN_POINT ( 'NONE',  ( 5.896875000614518747, 6.054752690667223547, 3.707466751127219781E-16 ) ) ;
#31254 = CARTESIAN_POINT ( 'NONE',  ( 17.22187500061451715, 3.027376345333611329, 5.243569643749999010 ) ) ;
#31255 = PLANE ( 'NONE',  #34820 ) ;
#31256 = ORIENTED_EDGE ( 'NONE', *, *, #23957, .F. ) ;
#31257 = CARTESIAN_POINT ( 'NONE',  ( 29.57812500061451644, 6.421520780324663323E-16, -5.243569643749999010 ) ) ;
#31258 = CARTESIAN_POINT ( 'NONE',  ( 26.78437500061451360, -4.541064518000419881, 2.621784821874995952 ) ) ;
#31259 = CARTESIAN_POINT ( 'NONE',  ( -4.000000000000000888, 14.95624999877096428, 32.30940107675850470 ) ) ;
#31260 = CARTESIAN_POINT ( 'NONE',  ( 15.33750000000000036, -2.886751345948125991, -5.000000000000000000 ) ) ;
#31261 = CARTESIAN_POINT ( 'NONE',  ( 14.76562500061451821, 3.027376345333613106, -5.243569643749998122 ) ) ;
#31262 = CARTESIAN_POINT ( 'NONE',  ( -3.999999999999999112, 15.05000000000000071, -30.00000000000000000 ) ) ;
#31263 = CARTESIAN_POINT ( 'NONE',  ( 0.000000000000000000, 20.00000000000000000, 26.00000000000000000 ) ) ;
#31264 = CARTESIAN_POINT ( 'NONE',  ( -3.137519842735245283E-14, 11.56250000000000178, -26.00000000000000711 ) ) ;
#31265 = CARTESIAN_POINT ( 'NONE',  ( 19.12500000122903288, 2.886751345948129099, -4.999999999999998224 ) ) ;
#31266 = CARTESIAN_POINT ( 'NONE',  ( 15.11250000122903359, 4.330127018922192761, -2.499999999999997780 ) ) ;
#31267 = CARTESIAN_POINT ( 'NONE',  ( 16.43437500061451573, -4.119189519843968306, 2.378215178124996054 ) ) ;
#31268 = CARTESIAN_POINT ( 'NONE',  ( 7.753125000614518036, 0.000000000000000000, 5.243569643749999010 ) ) ;
#31269 = CARTESIAN_POINT ( 'NONE',  ( 25.24687500061451573, 6.054752690667223547, 3.707466751127219781E-16 ) ) ;
#31270 = CARTESIAN_POINT ( 'NONE',  ( -4.243569643749997233, 16.74687500061451928, 32.45002607614398471 ) ) ;
#31271 = CARTESIAN_POINT ( 'NONE',  ( 24.08437500061451786, -4.541064518000419881, 2.621784821874995952 ) ) ;
#31272 = CARTESIAN_POINT ( 'NONE',  ( 4.837500000000001243, -2.886751345948129988, 4.999999999999997335 ) ) ;
#31273 = CARTESIAN_POINT ( 'NONE',  ( -2.000000000000000000, 11.48750000122903359, 26.53589838486224650 ) ) ;
#31274 = CARTESIAN_POINT ( 'NONE',  ( 12.32812500061451821, -4.541064518000419881, 2.621784821874995952 ) ) ;
#31275 = CARTESIAN_POINT ( 'NONE',  ( 3.375000001229033320, 2.886751345948129099, -4.999999999999998224 ) ) ;
#31276 = CARTESIAN_POINT ( 'NONE',  ( 8.409375000614518925, -4.541064518000417216, -2.621784821875001281 ) ) ;
#31277 = CARTESIAN_POINT ( 'NONE',  ( 3.947751918878622757, -3.068428716296062841, 3.947751918878600108 ) ) ;
#31278 = ORIENTED_EDGE ( 'NONE', *, *, #34726, .T. ) ;
#31279 = VECTOR ( 'NONE', #29822, 1000.000000000000000 ) ;
#31280 = CARTESIAN_POINT ( 'NONE',  ( 10.26562500061451644, 3.027376345333613106, -5.243569643749998122 ) ) ;
#31281 = CARTESIAN_POINT ( 'NONE',  ( 14.67187500061451821, -6.054752690667223547, -1.112240025338166033E-15 ) ) ;
#31282 = LINE ( 'NONE', #7295, #68618 ) ;
#31283 = CARTESIAN_POINT ( 'NONE',  ( 20.70000000122903216, -2.886751345948129988, 4.999999999999997335 ) ) ;
#31284 = CARTESIAN_POINT ( 'NONE',  ( 10.73437500061451644, 6.421520780324663323E-16, -5.243569643749999010 ) ) ;
#31285 = CARTESIAN_POINT ( 'NONE',  ( 13.26562500061451644, -6.054752690667223547, -1.112240025338166033E-15 ) ) ;
#31286 = CARTESIAN_POINT ( 'NONE',  ( 28.25625000122903074, 0.000000000000000000, 4.999999999999998224 ) ) ;
#31287 = CARTESIAN_POINT ( 'NONE',  ( 20.74687500061451573, 6.054752690667223547, 3.707466751127219781E-16 ) ) ;
#31288 = CARTESIAN_POINT ( 'NONE',  ( -1.487416814333745711E-14, 15.72500000122903430, 34.00000000000000000 ) ) ;
#31289 = AXIS2_PLACEMENT_3D ( 'NONE', #23072, #50800, #17524 ) ;
#31290 = CARTESIAN_POINT ( 'NONE',  ( 23.81250000000000000, -5.773502691896255534, -1.060575238724906372E-15 ) ) ;
#31291 = FACE_OUTER_BOUND ( 'NONE', #2659, .T. ) ;
#31292 = CARTESIAN_POINT ( 'NONE',  ( 2.121784821874999061, 13.85937500061451821, -33.67503911421598417 ) ) ;
#31293 = CARTESIAN_POINT ( 'NONE',  ( 16.69687500061451502, 6.054752690667223547, 3.707466751127219781E-16 ) ) ;
#31294 = CARTESIAN_POINT ( 'NONE',  ( 15.26250000122903216, 0.000000000000000000, 4.999999999999998224 ) ) ;
#31295 = CARTESIAN_POINT ( 'NONE',  ( 12.34687500061452070, -3.027376345333614438, 5.243569643749998122 ) ) ;
#31296 = CARTESIAN_POINT ( 'NONE',  ( -4.243569643749997233, 18.04062500061451857, -27.54997392385601174 ) ) ;
#31297 = CARTESIAN_POINT ( 'NONE',  ( 17.40000000122903145, 5.773502691896255534, 3.535250795749688894E-16 ) ) ;
#31298 = CARTESIAN_POINT ( 'NONE',  ( 12.89062500061451821, -3.027376345333610441, -5.243569643749999898 ) ) ;
#31299 = ORIENTED_EDGE ( 'NONE', *, *, #44872, .F. ) ;
#31300 = AXIS2_PLACEMENT_3D ( 'NONE', #6162, #45328, #67864 ) ;
#31301 = CARTESIAN_POINT ( 'NONE',  ( 16.05000000000000071, 0.000000000000000000, 4.999999999999998224 ) ) ;
#31302 = CARTESIAN_POINT ( 'NONE',  ( 20.77500000000000213, 6.123233995736764310E-16, -4.999999999999998224 ) ) ;
#31303 = CARTESIAN_POINT ( 'NONE',  ( 9.271875000614519635, -6.054752690667223547, -1.112240025338166033E-15 ) ) ;
#31304 = CARTESIAN_POINT ( 'NONE',  ( 0.5593513097472442297, 4.976037924071838425, 26.02984368186838893 ) ) ;
#31305 = CARTESIAN_POINT ( 'NONE',  ( 11.73750000122903181, -4.330127018922194537, 2.499999999999995559 ) ) ;
#31306 = CARTESIAN_POINT ( 'NONE',  ( 21.22500000122903074, -5.773502691896255534, -1.060575238724906372E-15 ) ) ;
#31307 = CARTESIAN_POINT ( 'NONE',  ( 16.90312500061451573, -4.541064518000417216, -2.621784821875001281 ) ) ;
#31308 = CARTESIAN_POINT ( 'NONE',  ( 20.91562500061451502, -6.054752690667223547, -1.112240025338166033E-15 ) ) ;
#31309 = CARTESIAN_POINT ( 'NONE',  ( 27.90000000122903145, -2.886751345948129988, 4.999999999999997335 ) ) ;
#31310 = CARTESIAN_POINT ( 'NONE',  ( 4.303125000614516971, -4.541064518000417216, -2.621784821875001281 ) ) ;
#31311 = CARTESIAN_POINT ( 'NONE',  ( 24.78750000000000497, -2.886751345948125991, -5.000000000000000000 ) ) ;
#31312 = CARTESIAN_POINT ( 'NONE',  ( 0.000000000000000000, -10.00000000000000000, 0.000000000000000000 ) ) ;
#31313 = CARTESIAN_POINT ( 'NONE',  ( 28.31250000000000000, -5.773502691896255534, -1.060575238724906372E-15 ) ) ;
#31314 = CARTESIAN_POINT ( 'NONE',  ( 27.75937500061451502, -4.541064518000417216, -2.621784821875001281 ) ) ;
#31315 = CARTESIAN_POINT ( 'NONE',  ( -3.000416591977282496E-16, 14.34687500061451715, -34.90005215228797653 ) ) ;
#31316 = CARTESIAN_POINT ( 'NONE',  ( 3.300000001229034918, -2.886751345948125991, -5.000000000000000000 ) ) ;
#31317 = CARTESIAN_POINT ( 'NONE',  ( 3.787500000000002753, 5.773502691896255534, 3.535250795749688894E-16 ) ) ;
#31318 = EDGE_CURVE ( 'NONE', #64487, #53529, #28797, .T. ) ;
#31319 = DIRECTION ( 'NONE',  ( -0.000000000000000000, -1.000000000000000000, -0.000000000000000000 ) ) ;
#31320 = CARTESIAN_POINT ( 'NONE',  ( 6.909375000614518036, 0.000000000000000000, 5.243569643749999010 ) ) ;
#31321 = CARTESIAN_POINT ( 'NONE',  ( 25.11562500061451431, 3.027376345333613106, -5.243569643749998122 ) ) ;
#31322 = CARTESIAN_POINT ( 'NONE',  ( 14.43750000000000000, -2.886751345948126435, -5.000000000000000000 ) ) ;
#31323 = VECTOR ( 'NONE', #6854, 1000.000000000000000 ) ;
#31324 = CARTESIAN_POINT ( 'NONE',  ( -1.999999999999997113, 19.28750000122903430, 33.46410161513775705 ) ) ;
#31325 = CARTESIAN_POINT ( 'NONE',  ( 4.659375000614518925, 0.000000000000000000, 5.243569643749999010 ) ) ;
#31326 = CARTESIAN_POINT ( 'NONE',  ( 8.221875000614518925, 3.027376345333611329, 5.243569643749999010 ) ) ;
#31327 = CARTESIAN_POINT ( 'NONE',  ( 3.187500000000002220, -2.886751345948125991, -5.000000000000000000 ) ) ;
#31328 = AXIS2_PLACEMENT_3D ( 'NONE', #24071, #12628, #52157 ) ;
#31329 = CARTESIAN_POINT ( 'NONE',  ( -2.121784821874999949, 11.62812500061459531, 26.32496088578401938 ) ) ;
#31330 = CARTESIAN_POINT ( 'NONE',  ( 20.73750000122903359, -4.330127018922194537, 2.499999999999995559 ) ) ;
#31331 = CARTESIAN_POINT ( 'NONE',  ( 3.750000000000000000, 4.330127018922192761, -2.499999999999997780 ) ) ;
#31332 = CIRCLE ( 'NONE', #28964, 1.500000000000000444 ) ;
#31333 = CARTESIAN_POINT ( 'NONE',  ( 15.53437500061451360, -2.746126346562642428, -4.756430356249999214 ) ) ;
#31334 = ORIENTED_EDGE ( 'NONE', *, *, #3173, .T. ) ;
#31335 = CARTESIAN_POINT ( 'NONE',  ( 19.86562500061451786, 3.027376345333611329, 5.243569643749999010 ) ) ;
#31336 = CARTESIAN_POINT ( 'NONE',  ( 10.07812500061451644, -4.541064518000419881, 2.621784821874995952 ) ) ;
#31337 = CARTESIAN_POINT ( 'NONE',  ( 24.19687500061451502, 4.119189519843966529, -2.378215178124998275 ) ) ;
#31338 = CARTESIAN_POINT ( 'NONE',  ( 9.721875000614517148, -6.054752690667223547, -1.112240025338166033E-15 ) ) ;
#31339 = CARTESIAN_POINT ( 'NONE',  ( 26.96249999999999858, -5.773502691896255534, -1.060575238724906372E-15 ) ) ;
#31340 = CARTESIAN_POINT ( 'NONE',  ( 20.06250000122903643, 4.330127018922192761, -2.499999999999997780 ) ) ;
#31341 = CARTESIAN_POINT ( 'NONE',  ( 28.49062500061451431, -3.027376345333614438, 5.243569643749998122 ) ) ;
#31342 = CARTESIAN_POINT ( 'NONE',  ( 16.03125000122903288, 4.330127018922191873, 2.499999999999999556 ) ) ;
#31343 = VECTOR ( 'NONE', #9357, 1000.000000000000000 ) ;
#31344 = CARTESIAN_POINT ( 'NONE',  ( 8.409375000614518925, -4.541064518000417216, -2.621784821875001281 ) ) ;
#31345 = CARTESIAN_POINT ( 'NONE',  ( 14.25937500061451679, -4.541064518000417216, -2.621784821875001281 ) ) ;
#31346 = CARTESIAN_POINT ( 'NONE',  ( 26.10937500061451644, 4.541064518000418104, -2.621784821874998173 ) ) ;
#31347 = CARTESIAN_POINT ( 'NONE',  ( 8.587500001229035007, -4.330127018922194537, 2.499999999999995559 ) ) ;
#31348 = CARTESIAN_POINT ( 'NONE',  ( 12.93750000000000178, -2.886751345948129988, 4.999999999999997335 ) ) ;
#31349 = CARTESIAN_POINT ( 'NONE',  ( 20.40937500061451715, 0.000000000000000000, 5.243569643749999010 ) ) ;
#31350 = CARTESIAN_POINT ( 'NONE',  ( 12.30937500061451573, 0.000000000000000000, 5.243569643749999010 ) ) ;
#31351 = CARTESIAN_POINT ( 'NONE',  ( -3.756430356250001434, 13.80312499938548321, 32.16877607737301048 ) ) ;
#31352 = CARTESIAN_POINT ( 'NONE',  ( 24.48749999999999716, 5.773502691896255534, 3.535250795749688894E-16 ) ) ;
#31353 = CARTESIAN_POINT ( 'NONE',  ( -2.000000000000001776, 15.05000000000000071, 33.46410161513775705 ) ) ;
#31354 = CARTESIAN_POINT ( 'NONE',  ( 2.121784821874999061, 12.95937500061451786, -33.67503911421598417 ) ) ;
#31355 = CARTESIAN_POINT ( 'NONE',  ( 24.57187500061451502, -5.492252693125287522, -1.008910452111647106E-15 ) ) ;
#31356 = CARTESIAN_POINT ( 'NONE',  ( 14.65312500061451573, -4.541064518000417216, -2.621784821875001281 ) ) ;
#31357 = CARTESIAN_POINT ( 'NONE',  ( 3.862500000000001155, 2.886751345948126879, 4.999999999999999112 ) ) ;
#31358 = CARTESIAN_POINT ( 'NONE',  ( 45.00000000000000000, 6.123233995736764310E-16, -4.999999999999998224 ) ) ;
#31359 = CARTESIAN_POINT ( 'NONE',  ( 4.276577733362700862, 2.590537181842085257, -4.276577733362700862 ) ) ;
#31360 = CARTESIAN_POINT ( 'NONE',  ( 12.82499999999999929, 4.330127018922191873, 2.499999999999999556 ) ) ;
#31361 = CARTESIAN_POINT ( 'NONE',  ( -2.828200636599751609E-16, 18.65000000122903501, 25.38119784648299770 ) ) ;
#31362 = CARTESIAN_POINT ( 'NONE',  ( 10.98750000122903536, 6.123233995736764310E-16, -4.999999999999998224 ) ) ;
#31363 = CARTESIAN_POINT ( 'NONE',  ( 23.25937500061451857, -4.541064518000417216, -2.621784821875001281 ) ) ;
#31364 = CARTESIAN_POINT ( 'NONE',  ( 16.05937500061451573, -4.541064518000417216, -2.621784821875001281 ) ) ;
#31365 = DIRECTION ( 'NONE',  ( -0.000000000000000000, -1.000000000000000000, -0.000000000000000000 ) ) ;
#31366 = ORIENTED_EDGE ( 'NONE', *, *, #6059, .F. ) ;
#31367 = CARTESIAN_POINT ( 'NONE',  ( 17.65312500061451573, 0.000000000000000000, 5.243569643749999010 ) ) ;
#31368 = CARTESIAN_POINT ( 'NONE',  ( 3.440625000614518036, -3.027376345333610441, -5.243569643749999898 ) ) ;
#31369 = CARTESIAN_POINT ( 'NONE',  ( 16.77187500061451786, 3.027376345333611329, 5.243569643749999010 ) ) ;
#31370 = CARTESIAN_POINT ( 'NONE',  ( 29.07187500061451502, -6.054752690667223547, -1.112240025338166033E-15 ) ) ;
#31371 = CARTESIAN_POINT ( 'NONE',  ( 5.428125000614517859, 4.541064518000418104, 2.621784821874999949 ) ) ;
#31372 = CARTESIAN_POINT ( 'NONE',  ( 20.61562500061451431, 3.027376345333613106, -5.243569643749998122 ) ) ;
#31373 = CARTESIAN_POINT ( 'NONE',  ( 4.243569643749999898, 15.49062500061451786, 32.45002607614398471 ) ) ;
#31374 = CARTESIAN_POINT ( 'NONE',  ( 15.41250000122903252, -4.330127018922190985, -2.500000000000001332 ) ) ;
#31375 = CARTESIAN_POINT ( 'NONE',  ( 12.12187500061451573, 2.746126346562645981, -4.756430356249997438 ) ) ;
#31376 = CARTESIAN_POINT ( 'NONE',  ( 6.515625000614516438, -6.054752690667223547, -1.112240025338166033E-15 ) ) ;
#31377 = CARTESIAN_POINT ( 'NONE',  ( 3.459375000614519635, -4.541064518000417216, -2.621784821875001281 ) ) ;
#31378 = CARTESIAN_POINT ( 'NONE',  ( 4.000000000000000000, 18.95000000122903216, -27.69059892324149885 ) ) ;
#31379 = CARTESIAN_POINT ( 'NONE',  ( 23.59687500061451715, -3.027376345333614438, 5.243569643749998122 ) ) ;
#31380 = CARTESIAN_POINT ( 'NONE',  ( 14.72812500061451679, 6.421520780324663323E-16, -5.243569643749999010 ) ) ;
#31381 = CARTESIAN_POINT ( 'NONE',  ( 24.33750000122903145, -4.330127018922194537, 2.499999999999995559 ) ) ;
#31382 = CARTESIAN_POINT ( 'NONE',  ( 22.86562500061451431, 3.027376345333613106, -5.243569643749998122 ) ) ;
#31383 = CARTESIAN_POINT ( 'NONE',  ( 19.69687500061451857, -3.027376345333610441, -5.243569643749999898 ) ) ;
#31384 = CARTESIAN_POINT ( 'NONE',  ( 15.66562500061451857, 3.027376345333613106, -5.243569643749998122 ) ) ;
#31385 = CARTESIAN_POINT ( 'NONE',  ( -2.121784821874996840, 14.08437500061451786, 33.67503911421598417 ) ) ;
#31386 = AXIS2_PLACEMENT_3D ( 'NONE', #3131, #54832, #31196 ) ;
#31387 = CARTESIAN_POINT ( 'NONE',  ( 18.96562500061451573, 3.027376345333611329, 5.243569643749999010 ) ) ;
#31388 = CARTESIAN_POINT ( 'NONE',  ( 10.12500000000000178, 4.330127018922191873, 2.499999999999999556 ) ) ;
#31389 = ORIENTED_EDGE ( 'NONE', *, *, #67466, .T. ) ;
#31390 = EDGE_LOOP ( 'NONE', ( #54504, #12221, #54418, #45493 ) ) ;
#31391 = CARTESIAN_POINT ( 'NONE',  ( 22.98749999999999716, -2.886751345948125991, -5.000000000000000000 ) ) ;
#31392 = CARTESIAN_POINT ( 'NONE',  ( -1.999999999999997113, 10.62500000000000000, -26.53589838486224295 ) ) ;
#31393 = CARTESIAN_POINT ( 'NONE',  ( 27.25312500061451360, -4.541064518000417216, -2.621784821875001281 ) ) ;
#31394 = CARTESIAN_POINT ( 'NONE',  ( 7.303125000614516082, 0.000000000000000000, 5.243569643749999010 ) ) ;
#31395 = CARTESIAN_POINT ( 'NONE',  ( 20.13750000122903216, 4.330127018922191873, 2.499999999999999556 ) ) ;
#31396 = CARTESIAN_POINT ( 'NONE',  ( 24.06562500061451715, -6.054752690667223547, -1.112240025338166033E-15 ) ) ;
#31397 = CARTESIAN_POINT ( 'NONE',  ( 22.50000000000000000, -4.330127018922190985, -2.500000000000001332 ) ) ;
#31398 = CARTESIAN_POINT ( 'NONE',  ( 27.81562500061452070, 3.027376345333613106, -5.243569643749998122 ) ) ;
#31399 = CARTESIAN_POINT ( 'NONE',  ( 8.540625000614518569, 6.054752690667223547, 3.707466751127219781E-16 ) ) ;
#31400 =( BOUNDED_CURVE ( )  B_SPLINE_CURVE ( 2, ( #1627, #6432, #68493, #58106, #46685, #57026, #68139 ),
 .UNSPECIFIED., .F., .F. ) 
 B_SPLINE_CURVE_WITH_KNOTS ( ( 3, 2, 2, 3 ),
 ( 0.2583333333333333037, 0.2611111111111110716, 0.2638888888888888395, 0.2666666666666666075 ),
 .UNSPECIFIED. ) 
 CURVE ( )  GEOMETRIC_REPRESENTATION_ITEM ( )  RATIONAL_B_SPLINE_CURVE ( ( 1.000000000000002665, 0.8660254037844360431, 1.000000000000000000, 0.8660254037844387076, 1.000000000000000000, 0.8660254037844413721, 0.9999999999999973355 ) ) 
 REPRESENTATION_ITEM ( '' )  );
#31401 = ORIENTED_EDGE ( 'NONE', *, *, #43004, .T. ) ;
#31402 = CARTESIAN_POINT ( 'NONE',  ( 23.20312500061451644, -4.541064518000417216, -2.621784821875001281 ) ) ;
#31403 = CARTESIAN_POINT ( 'NONE',  ( 4.490625000614516971, 6.054752690667223547, 3.707466751127219781E-16 ) ) ;
#31404 = CARTESIAN_POINT ( 'NONE',  ( 13.02187500061451608, 2.746126346562645981, -4.756430356249997438 ) ) ;
#31405 = CARTESIAN_POINT ( 'NONE',  ( 3.028125000614518392, 6.421520780324663323E-16, -5.243569643749999010 ) ) ;
#31406 = CARTESIAN_POINT ( 'NONE',  ( -1.999999999999997113, 14.78750000122903252, -26.53589838486224295 ) ) ;
#31407 = EDGE_CURVE ( 'NONE', #17509, #29541, #18841, .T. ) ;
#31408 = CARTESIAN_POINT ( 'NONE',  ( -3.999999999999999112, 10.17500000122903359, 27.69059892324149885 ) ) ;
#31409 = CARTESIAN_POINT ( 'NONE',  ( 10.05000000000000071, 4.330127018922192761, -2.499999999999997780 ) ) ;
#31410 = CARTESIAN_POINT ( 'NONE',  ( 10.35937500061451644, 4.541064518000418104, -2.621784821874998173 ) ) ;
#31411 = CARTESIAN_POINT ( 'NONE',  ( 9.337500001229033231, 4.330127018922191873, 2.499999999999999556 ) ) ;
#31412 = CARTESIAN_POINT ( 'NONE',  ( 14.93437500061451750, 4.541064518000418104, 2.621784821874999949 ) ) ;
#31413 = CARTESIAN_POINT ( 'NONE',  ( 15.41250000000000142, 2.886751345948129099, -4.999999999999998224 ) ) ;
#31414 = CARTESIAN_POINT ( 'NONE',  ( 6.571875000614517681, -6.054752690667223547, -1.112240025338166033E-15 ) ) ;
#31415 = CARTESIAN_POINT ( 'NONE',  ( -2.121784821874996840, 9.978125000614518569, -26.32496088578401583 ) ) ;
#31416 = LINE ( 'NONE', #70203, #32410 ) ;
#31417 = CARTESIAN_POINT ( 'NONE',  ( 13.02187500061451608, 3.027376345333613106, -5.243569643749998122 ) ) ;
#31418 = CARTESIAN_POINT ( 'NONE',  ( 21.82500000122903572, 2.886751345948095793, -5.000000000000055067 ) ) ;
#31419 = CARTESIAN_POINT ( 'NONE',  ( 22.07812500061451644, 4.541064518000418104, 2.621784821874999949 ) ) ;
#31420 = CARTESIAN_POINT ( 'NONE',  ( -3.000416591977282496E-16, 11.19687500061451679, 25.09994784771203058 ) ) ;
#31421 = CARTESIAN_POINT ( 'NONE',  ( 26.51249999999999929, -5.773502691896255534, -1.060575238724906372E-15 ) ) ;
#31422 = CARTESIAN_POINT ( 'NONE',  ( 26.03437500061451715, 6.421520780324663323E-16, -5.243569643749999010 ) ) ;
#31423 = DIRECTION ( 'NONE',  ( -0.000000000000000000, -1.000000000000000000, -0.000000000000000000 ) ) ;
#31424 = CARTESIAN_POINT ( 'NONE',  ( 5.278125000614516615, 6.421520780324663323E-16, -5.243569643749999010 ) ) ;
#31425 = CARTESIAN_POINT ( 'NONE',  ( 21.94687500061451146, 4.119189519843966529, -2.378215178124998275 ) ) ;
#31426 = CARTESIAN_POINT ( 'NONE',  ( 16.47187500061452070, -6.054752690667223547, -1.112240025338166033E-15 ) ) ;
#31427 = CARTESIAN_POINT ( 'NONE',  ( 7.996875000614515727, 4.119189519843966529, -2.378215178124998275 ) ) ;
#31428 = CARTESIAN_POINT ( 'NONE',  ( 27.18750000122903288, 6.123233995736764310E-16, -4.999999999999998224 ) ) ;
#31429 = CARTESIAN_POINT ( 'NONE',  ( 5.446875000614518569, 6.054752690667223547, 3.707466751127219781E-16 ) ) ;
#31430 = CARTESIAN_POINT ( 'NONE',  ( 16.88437500061451502, -4.541064518000419881, 2.621784821874995952 ) ) ;
#31431 = CARTESIAN_POINT ( 'NONE',  ( 4.819830401275195797, -1.330621173773433918, -5.072058569993805222 ) ) ;
#31432 = CARTESIAN_POINT ( 'NONE',  ( 23.96249999999999858, 2.886751345948129099, -4.999999999999998224 ) ) ;
#31433 = CARTESIAN_POINT ( 'NONE',  ( 3.637500001229036162, -4.330127018922194537, 2.499999999999995559 ) ) ;
#31434 = CARTESIAN_POINT ( 'NONE',  ( 27.68437500061451573, -4.541064518000419881, 2.621784821874995952 ) ) ;
#31435 = CARTESIAN_POINT ( 'NONE',  ( 2.655984681222220721E-16, 14.21562499938548463, 25.66244784525396483 ) ) ;
#31436 = CARTESIAN_POINT ( 'NONE',  ( 21.67500000000000071, 6.123233995736764310E-16, -4.999999999999998224 ) ) ;
#31437 = CARTESIAN_POINT ( 'NONE',  ( 6.862500000000002487, 2.886751345948129099, -4.999999999999998224 ) ) ;
#31438 = CARTESIAN_POINT ( 'NONE',  ( 9.121875000614517504, -4.119189519843968306, 2.378215178124996054 ) ) ;
#31439 = CARTESIAN_POINT ( 'NONE',  ( 22.90312500061451573, 4.541064518000418104, -2.621784821874998173 ) ) ;
#31440 = CARTESIAN_POINT ( 'NONE',  ( 12.00000000000000000, 0.000000000000000000, 4.999999999999998224 ) ) ;
#31441 = CARTESIAN_POINT ( 'NONE',  ( 4.303125000614516971, -4.541064518000417216, -2.621784821875001281 ) ) ;
#31442 = CARTESIAN_POINT ( 'NONE',  ( 19.87500000000000000, 6.123233995736764310E-16, -4.999999999999998224 ) ) ;
#31443 = CARTESIAN_POINT ( 'NONE',  ( 18.81562500061452070, 3.027376345333613106, -5.243569643749998122 ) ) ;
#31444 = CARTESIAN_POINT ( 'NONE',  ( 4.057522967627288146, -2.921730200955767298, 4.057522967627288146 ) ) ;
#31445 = CARTESIAN_POINT ( 'NONE',  ( 23.55000000122903359, -2.886751345948125991, -5.000000000000000000 ) ) ;
#31446 = CARTESIAN_POINT ( 'NONE',  ( 1.878215178124997609, 18.86562499938548143, 33.25316411605952993 ) ) ;
#31447 = CARTESIAN_POINT ( 'NONE',  ( 3.787500000000002753, 5.773502691896255534, 3.535250795749688894E-16 ) ) ;
#31448 = ORIENTED_EDGE ( 'NONE', *, *, #9880, .F. ) ;
#31449 = CARTESIAN_POINT ( 'NONE',  ( 20.57812500061451644, 6.421520780324663323E-16, -5.243569643749999010 ) ) ;
#31450 = CARTESIAN_POINT ( 'NONE',  ( 26.91562500061451146, 3.027376345333613106, -5.243569643749998122 ) ) ;
#31451 = CARTESIAN_POINT ( 'NONE',  ( 24.98437500061451644, -4.541064518000419881, 2.621784821874995952 ) ) ;
#31452 = CARTESIAN_POINT ( 'NONE',  ( 8.512499999999999289, -5.773502691896255534, -1.060575238724906372E-15 ) ) ;
#31453 = CARTESIAN_POINT ( 'NONE',  ( 11.39062500061451644, -3.027376345333614438, 5.243569643749998122 ) ) ;
#31454 = CARTESIAN_POINT ( 'NONE',  ( 26.84062500061451573, -3.027376345333610441, -5.243569643749999898 ) ) ;
#31455 = CARTESIAN_POINT ( 'NONE',  ( 16.47187500061452070, -6.054752690667223547, -1.112240025338166033E-15 ) ) ;
#31456 = CARTESIAN_POINT ( 'NONE',  ( 9.628125000614517148, -4.541064518000419881, 2.621784821874995952 ) ) ;
#31457 = CARTESIAN_POINT ( 'NONE',  ( 14.26875000122903181, 2.886751345948182834, 4.999999999999902300 ) ) ;
#31458 = CARTESIAN_POINT ( 'NONE',  ( -2.121784821874999949, 11.23437500061451821, 26.32496088578401938 ) ) ;
#31459 = CARTESIAN_POINT ( 'NONE',  ( 23.25000000122903288, 5.773502691896255534, 3.535250795749688894E-16 ) ) ;
#31460 = CARTESIAN_POINT ( 'NONE',  ( 19.43437500061451928, 4.119189519843966529, 2.378215178124999607 ) ) ;
#31461 = CARTESIAN_POINT ( 'NONE',  ( 15.44062500061451892, -3.027376345333614438, 5.243569643749998122 ) ) ;
#31462 = CARTESIAN_POINT ( 'NONE',  ( 9.721875000614517148, -6.054752690667223547, -1.112240025338166033E-15 ) ) ;
#31463 = CARTESIAN_POINT ( 'NONE',  ( 9.571875000614518569, 3.027376345333611329, 5.243569643749999010 ) ) ;
#31464 = ORIENTED_EDGE ( 'NONE', *, *, #24944, .F. ) ;
#31465 = CARTESIAN_POINT ( 'NONE',  ( -1.964573642069356252, 9.807014569943703464, 35.67272520908200306 ) ) ;
#31466 = CARTESIAN_POINT ( 'NONE',  ( 21.36562500061451431, -6.054752690667223547, -1.112240025338166033E-15 ) ) ;
#31467 = EDGE_CURVE ( 'NONE', #30832, #48258, #26417, .T. ) ;
#31468 = CARTESIAN_POINT ( 'NONE',  ( 17.52187500061451431, 3.027376345333613106, -5.243569643749998122 ) ) ;
#31469 = CARTESIAN_POINT ( 'NONE',  ( 20.80312500061451431, 0.000000000000000000, 5.243569643749999010 ) ) ;
#31470 = CARTESIAN_POINT ( 'NONE',  ( -3.999999999999999556, 11.41250000000000142, 27.69059892324149530 ) ) ;
#31471 = CARTESIAN_POINT ( 'NONE',  ( 26.05312500061451431, 4.541064518000418104, -2.621784821874998173 ) ) ;
#31472 = CARTESIAN_POINT ( 'NONE',  ( 6.075000001229034829, 2.886751345948129099, -4.999999999999998224 ) ) ;
#31473 = ORIENTED_EDGE ( 'NONE', *, *, #3140, .T. ) ;
#31474 = CARTESIAN_POINT ( 'NONE',  ( 29.36250000000000071, 2.886751345948129099, -4.999999999999998224 ) ) ;
#31475 = CARTESIAN_POINT ( 'NONE',  ( 4.000000000000000000, 17.03750000000000142, -27.69059892324149530 ) ) ;
#31476 = AXIS2_PLACEMENT_3D ( 'NONE', #70826, #20200, #25393 ) ;
#31477 = CARTESIAN_POINT ( 'NONE',  ( 25.23750000122903359, -4.330127018922194537, 2.499999999999995559 ) ) ;
#31478 = CARTESIAN_POINT ( 'NONE',  ( -1.878215178124999163, 15.60312499938548392, 26.74683588394047007 ) ) ;
#31479 = ADVANCED_FACE ( 'NONE', ( #61685 ), #5905, .T. ) ;
#31480 = CARTESIAN_POINT ( 'NONE',  ( 5.971875000614516260, 3.027376345333611329, 5.243569643749999010 ) ) ;
#31481 = CARTESIAN_POINT ( 'NONE',  ( 23.43750000000000000, -2.886751345948142422, -4.999999999999970690 ) ) ;
#31482 = CARTESIAN_POINT ( 'NONE',  ( 15.51562500061451644, -6.054752690667223547, -1.112240025338166033E-15 ) ) ;
#31483 = CARTESIAN_POINT ( 'NONE',  ( 8.146875000614516082, 6.054752690667223547, 3.707466751127219781E-16 ) ) ;
#31484 = CARTESIAN_POINT ( 'NONE',  ( 25.95000000122903216, 5.773502691896255534, 3.535250795749688894E-16 ) ) ;
#31485 = CARTESIAN_POINT ( 'NONE',  ( 16.84687500061452070, -3.027376345333614438, 5.243569643749998122 ) ) ;
#31486 = CARTESIAN_POINT ( 'NONE',  ( 6.196875000614515905, -3.027376345333610441, -5.243569643749999898 ) ) ;
#31487 = DIRECTION ( 'NONE',  ( -0.000000000000000000, -1.000000000000000000, -0.000000000000000000 ) ) ;
#31488 = EDGE_CURVE ( 'NONE', #3749, #26440, #45074, .T. ) ;
#31489 = CARTESIAN_POINT ( 'NONE',  ( 4.753125000614515372, -4.541064518000417216, -2.621784821875001281 ) ) ;
#31490 = CARTESIAN_POINT ( 'NONE',  ( 15.14062500061451644, -3.027376345333610441, -5.243569643749999898 ) ) ;
#31491 = ORIENTED_EDGE ( 'NONE', *, *, #68597, .F. ) ;
#31492 = CARTESIAN_POINT ( 'NONE',  ( 12.96562500061451750, 3.027376345333613106, -5.243569643749998122 ) ) ;
#31493 = VECTOR ( 'NONE', #25693, 1000.000000000000227 ) ;
#31494 = CARTESIAN_POINT ( 'NONE',  ( 5.625000001229036428, 2.886751345948129099, -4.999999999999998224 ) ) ;
#31495 = CARTESIAN_POINT ( 'NONE',  ( 10.11562500061451608, -6.054752690667223547, -1.112240025338166033E-15 ) ) ;
#31496 = CARTESIAN_POINT ( 'NONE',  ( 20.14687500061451786, -2.746126346562642428, -4.756430356249999214 ) ) ;
#31497 = CARTESIAN_POINT ( 'NONE',  ( 11.47499999999999964, 4.330127018922191873, 2.499999999999999556 ) ) ;
#31498 = CARTESIAN_POINT ( 'NONE',  ( 3.750000001229034652, -2.886751345948125991, -5.000000000000000000 ) ) ;
#31499 = CARTESIAN_POINT ( 'NONE',  ( 18.07499999999999929, 6.123233995736764310E-16, -4.999999999999998224 ) ) ;
#31500 = CARTESIAN_POINT ( 'NONE',  ( 19.54687500061451644, -3.027376345333614438, 5.243569643749998122 ) ) ;
#31501 = CARTESIAN_POINT ( 'NONE',  ( 15.86250000122903181, -4.330127018922190985, -2.500000000000001332 ) ) ;
#31502 = CARTESIAN_POINT ( 'NONE',  ( 21.37499999999999645, 4.330127018922191873, 2.499999999999999556 ) ) ;
#31503 = CARTESIAN_POINT ( 'NONE',  ( -2.121784821874999949, 17.02812500061451573, -33.67503911421598417 ) ) ;
#31504 = CARTESIAN_POINT ( 'NONE',  ( 12.11250000122903181, 0.000000000000000000, 4.999999999999998224 ) ) ;
#31505 = CARTESIAN_POINT ( 'NONE',  ( 2.814937200665621919, -4.236319168869982832, -2.662479962439228132 ) ) ;
#31506 = CARTESIAN_POINT ( 'NONE',  ( 29.39062500061451289, -3.027376345333614438, 5.243569643749998122 ) ) ;
#31507 = EDGE_CURVE ( 'NONE', #22068, #23988, #61810, .T. ) ;
#31508 = CARTESIAN_POINT ( 'NONE',  ( 4.826610586788474322, 1.315217771577623873, 4.826610586788474322 ) ) ;
#31509 = DIRECTION ( 'NONE',  ( -1.000000000000000000, -0.000000000000000000, -0.000000000000000000 ) ) ;
#31510 = CARTESIAN_POINT ( 'NONE',  ( 16.80937500061451573, 0.000000000000000000, 5.243569643749999010 ) ) ;
#31511 = CARTESIAN_POINT ( 'NONE',  ( 28.83749999999999858, -2.886751345948125991, -5.000000000000000000 ) ) ;
#31512 = CARTESIAN_POINT ( 'NONE',  ( 12.66562500061451502, 3.027376345333611329, 5.243569643749999010 ) ) ;
#31513 = CARTESIAN_POINT ( 'NONE',  ( 29.67187500061451644, 4.119189519843966529, 2.378215178124999607 ) ) ;
#31514 = CARTESIAN_POINT ( 'NONE',  ( 23.63437500061451502, -4.541064518000419881, 2.621784821874995952 ) ) ;
#31515 = CARTESIAN_POINT ( 'NONE',  ( 15.42187500061451466, -4.119189519843968306, 2.378215178124996054 ) ) ;
#31516 = CARTESIAN_POINT ( 'NONE',  ( 8.690625000614515372, -3.027376345333614438, 5.243569643749998122 ) ) ;
#31517 = CARTESIAN_POINT ( 'NONE',  ( 13.54687500061451999, 6.054752690667223547, 3.707466751127219781E-16 ) ) ;
#31518 = VERTEX_POINT ( 'NONE', #67256 ) ;
#31519 = CARTESIAN_POINT ( 'NONE',  ( 24.08437500061451786, -4.541064518000419881, 2.621784821874995952 ) ) ;
#31520 = CARTESIAN_POINT ( 'NONE',  ( 28.56562500061451715, -6.054752690667223547, -1.112240025338166033E-15 ) ) ;
#31521 = CARTESIAN_POINT ( 'NONE',  ( 17.04375000122903572, -2.886751345948130876, 4.999999999999996447 ) ) ;
#31522 = CARTESIAN_POINT ( 'NONE',  ( 7.387500000000001066, 5.773502691896255534, 3.535250795749688894E-16 ) ) ;
#31523 = VECTOR ( 'NONE', #23553, 1000.000000000000000 ) ;
#31524 = CARTESIAN_POINT ( 'NONE',  ( 17.66250000122903430, -4.330127018922190985, -2.500000000000001332 ) ) ;
#31525 = CARTESIAN_POINT ( 'NONE',  ( 8.859375000614514661, 2.746126346562645981, -4.756430356249997438 ) ) ;
#31526 = ORIENTED_EDGE ( 'NONE', *, *, #57166, .T. ) ;
#31527 = CARTESIAN_POINT ( 'NONE',  ( 16.19999999999999929, -4.330127018922190985, -2.500000000000001332 ) ) ;
#31528 = CARTESIAN_POINT ( 'NONE',  ( 18.89999999999999858, -4.330127018922190985, -2.500000000000001332 ) ) ;
#31529 = CARTESIAN_POINT ( 'NONE',  ( 14.69062500061451537, -3.027376345333610441, -5.243569643749999898 ) ) ;
#31530 = ORIENTED_EDGE ( 'NONE', *, *, #16880, .F. ) ;
#31531 = CARTESIAN_POINT ( 'NONE',  ( -4.000000000000000888, 16.75624999877096499, 32.30940107675850470 ) ) ;
#31532 = CARTESIAN_POINT ( 'NONE',  ( 2.121784821875001281, 16.40937500061452070, -26.32496088578401938 ) ) ;
#31533 = CARTESIAN_POINT ( 'NONE',  ( 3.553125000614516082, 4.541064518000418104, -2.621784821874998173 ) ) ;
#31534 = CARTESIAN_POINT ( 'NONE',  ( 65.00000000000000000, 0.000000000000000000, 0.000000000000000000 ) ) ;
#31535 = CARTESIAN_POINT ( 'NONE',  ( 13.16249999999999964, 2.886751345948129099, -4.999999999999998224 ) ) ;
#31536 = CARTESIAN_POINT ( 'NONE',  ( 27.60937500061451644, -5.492252693125287522, -1.008910452111647106E-15 ) ) ;
#31537 = ORIENTED_EDGE ( 'NONE', *, *, #15860, .T. ) ;
#31538 = CARTESIAN_POINT ( 'NONE',  ( -2.121784821874996840, 15.37812500061451892, 33.67503911421598417 ) ) ;
#31539 = CARTESIAN_POINT ( 'NONE',  ( 26.24062500061451431, -3.027376345333614438, 5.243569643749998122 ) ) ;
#31540 = CARTESIAN_POINT ( 'NONE',  ( 25.74375000122903856, -2.886751345948098013, -5.000000000000047073 ) ) ;
#31541 = CARTESIAN_POINT ( 'NONE',  ( -3.756430356250001434, 20.10312499938548214, 32.16877607737301048 ) ) ;
#31542 = CARTESIAN_POINT ( 'NONE',  ( 24.83437500061451431, 4.541064518000418104, 2.621784821874999949 ) ) ;
#31543 = CARTESIAN_POINT ( 'NONE',  ( 17.99062500061451786, 6.054752690667223547, 3.707466751127219781E-16 ) ) ;
#31544 = CARTESIAN_POINT ( 'NONE',  ( 4.243569643749999898, 14.17812500061459247, -30.00000000000000000 ) ) ;
#31545 = CARTESIAN_POINT ( 'NONE',  ( 23.55000000122903359, -2.886751345948125991, -5.000000000000000000 ) ) ;
#31546 = CARTESIAN_POINT ( 'NONE',  ( 3.965625000614515727, 3.027376345333613106, -5.243569643749998122 ) ) ;
#31547 = CARTESIAN_POINT ( 'NONE',  ( 27.49687500061451573, 5.492252693125287522, 3.363034840372157021E-16 ) ) ;
#31548 = CARTESIAN_POINT ( 'NONE',  ( 20.61562500061451431, 3.027376345333612662, -5.243569643749998122 ) ) ;
#31549 = CARTESIAN_POINT ( 'NONE',  ( 9.234375000614518214, -4.119189519843968306, 2.378215178124996054 ) ) ;
#31550 = CARTESIAN_POINT ( 'NONE',  ( -1.878215178125001827, 16.99062499938548498, 33.25316411605952283 ) ) ;
#31551 =( BOUNDED_CURVE ( )  B_SPLINE_CURVE ( 2, ( #43836, #66363, #9484, #32746, #15738, #34913, #57075, #34546, #23097 ),
 .UNSPECIFIED., .F., .F. ) 
 B_SPLINE_CURVE_WITH_KNOTS ( ( 3, 2, 2, 2, 3 ),
 ( 0.4021739130434782705, 0.4057971014492753881, 0.4130434782608695676, 0.4202898550724637472, 0.4239130434782608647 ),
 .UNSPECIFIED. ) 
 CURVE ( )  GEOMETRIC_REPRESENTATION_ITEM ( )  RATIONAL_B_SPLINE_CURVE ( ( 0.9330127018922194093, 0.9330127018922194093, 1.000000000000000000, 0.8660254037844387076, 1.000000000000000000, 0.8660254037844387076, 1.000000000000000000, 0.9330127018922194093, 0.9330127018922194093 ) ) 
 REPRESENTATION_ITEM ( '' )  );
#31552 = CARTESIAN_POINT ( 'NONE',  ( 16.69687500061451502, 6.054752690667223547, 3.707466751127219781E-16 ) ) ;
#31553 = CARTESIAN_POINT ( 'NONE',  ( 16.92187500061451999, -6.054752690667223547, -1.112240025338166033E-15 ) ) ;
#31554 = CARTESIAN_POINT ( 'NONE',  ( 25.99687500061451928, -3.027376345333610441, -5.243569643749999898 ) ) ;
#31555 = CARTESIAN_POINT ( 'NONE',  ( -4.243569643749999898, 13.97187500061451715, 27.54997392385601529 ) ) ;
#31556 = CARTESIAN_POINT ( 'NONE',  ( 6.065625000614516260, -6.054752690667223547, -1.112240025338166033E-15 ) ) ;
#31557 = CARTESIAN_POINT ( 'NONE',  ( 28.11562500061451431, -6.054752690667223547, -1.112240025338166033E-15 ) ) ;
#31558 = CARTESIAN_POINT ( 'NONE',  ( 28.34062500061451928, 6.054752690667223547, 3.707466751127219781E-16 ) ) ;
#31559 = CARTESIAN_POINT ( 'NONE',  ( 45.00000000000000000, 6.123233995736764310E-16, -4.999999999999998224 ) ) ;
#31560 = CARTESIAN_POINT ( 'NONE',  ( 8.484601909799253346E-16, 18.31250000000000355, 34.61880215351700230 ) ) ;
#31561 = CARTESIAN_POINT ( 'NONE',  ( 7.809375000614519280, 0.000000000000000000, 5.243569643749999010 ) ) ;
#31562 = CARTESIAN_POINT ( 'NONE',  ( 13.27500000122903323, 2.886751345948129099, -4.999999999999998224 ) ) ;
#31563 = CARTESIAN_POINT ( 'NONE',  ( 9.000000001229034652, -2.886751345948129988, 4.999999999999997335 ) ) ;
#31564 = CARTESIAN_POINT ( 'NONE',  ( 6.065625000614516260, -6.054752690667223547, -1.112240025338166033E-15 ) ) ;
#31565 = CARTESIAN_POINT ( 'NONE',  ( -3.999999999999999556, 17.13124999877096855, 27.69059892324149175 ) ) ;
#31566 = CARTESIAN_POINT ( 'NONE',  ( 21.28125000122903288, 6.123233995736764310E-16, -4.999999999999998224 ) ) ;
#31567 = CARTESIAN_POINT ( 'NONE',  ( 13.84687500061451537, -3.027376345333610441, -5.243569643749999898 ) ) ;
#31568 = FACE_OUTER_BOUND ( 'NONE', #68876, .T. ) ;
#31569 = ORIENTED_EDGE ( 'NONE', *, *, #42670, .F. ) ;
#31570 = CARTESIAN_POINT ( 'NONE',  ( 22.15312500061451573, 0.000000000000000000, 5.243569643749999010 ) ) ;
#31571 = CARTESIAN_POINT ( 'NONE',  ( 7.115625000614516082, 3.027376345333613106, -5.243569643749998122 ) ) ;
#31572 = CARTESIAN_POINT ( 'NONE',  ( 23.78437500061451360, 6.421520780324663323E-16, -5.243569643749999010 ) ) ;
#31573 = CARTESIAN_POINT ( 'NONE',  ( 7.865625000614516971, -6.054752690667223547, -1.112240025338166033E-15 ) ) ;
#31574 = CARTESIAN_POINT ( 'NONE',  ( 20.54999999999999716, 0.000000000000000000, 4.999999999999998224 ) ) ;
#31576 = EDGE_CURVE ( 'NONE', #12847, #58973, #19722, .T. ) ;
#31575 = CARTESIAN_POINT ( 'NONE',  ( 8.887500001229033941, 4.330127018922191873, 2.499999999999999556 ) ) ;
#31577 = CARTESIAN_POINT ( 'NONE',  ( 21.70312500061451644, 0.000000000000000000, 5.243569643749999010 ) ) ;
#31578 = CARTESIAN_POINT ( 'NONE',  ( -2.121784821874999949, 10.27812500061451750, -33.67503911421598417 ) ) ;
#31579 = CARTESIAN_POINT ( 'NONE',  ( 11.36250000122903536, -4.330127018922190985, -2.500000000000001332 ) ) ;
#31580 = CARTESIAN_POINT ( 'NONE',  ( 20.50312500061451715, -4.541064518000417216, -2.621784821875001281 ) ) ;
#31581 = CARTESIAN_POINT ( 'NONE',  ( 18.96562500061451573, 3.027376345333611329, 5.243569643749999010 ) ) ;
#31582 = CARTESIAN_POINT ( 'NONE',  ( 27.27187500061451431, -5.492252693125287522, -1.008910452111647106E-15 ) ) ;
#31583 = CARTESIAN_POINT ( 'NONE',  ( 17.10000000000000142, -4.330127018922190985, -2.500000000000001332 ) ) ;
#31584 = CARTESIAN_POINT ( 'NONE',  ( 10.95000000122903394, -2.886751345948125991, -5.000000000000000000 ) ) ;
#31585 = VECTOR ( 'NONE', #63264, 1000.000000000000000 ) ;
#31586 = CARTESIAN_POINT ( 'NONE',  ( 6.853125000614516793, 0.000000000000000000, 5.243569643749999010 ) ) ;
#31587 = CARTESIAN_POINT ( 'NONE',  ( 12.36562500061451608, -6.054752690667223547, -1.112240025338166033E-15 ) ) ;
#31588 = AXIS2_PLACEMENT_3D ( 'NONE', #21140, #48868, #55501 ) ;
#31589 = CARTESIAN_POINT ( 'NONE',  ( 24.03750000122903430, 6.123233995736764310E-16, -4.999999999999998224 ) ) ;
#31590 = CARTESIAN_POINT ( 'NONE',  ( 22.88437500061451857, 6.421520780324663323E-16, -5.243569643749999010 ) ) ;
#31591 = CARTESIAN_POINT ( 'NONE',  ( 22.06875000122903074, -5.773502691896255534, -1.060575238724906372E-15 ) ) ;
#31592 = CARTESIAN_POINT ( 'NONE',  ( 6.037500001229035185, 6.123233995736764310E-16, -4.999999999999998224 ) ) ;
#31593 =( BOUNDED_CURVE ( )  B_SPLINE_CURVE ( 2, ( #64202, #19125, #41679, #25042, #13589, #48324, #36136, #53491, #20222 ),
 .UNSPECIFIED., .F., .F. ) 
 B_SPLINE_CURVE_WITH_KNOTS ( ( 3, 2, 2, 2, 3 ),
 ( 0.1847826086956521896, 0.1884057971014492794, 0.1956521739130434867, 0.2028985507246376940, 0.2065217391304347838 ),
 .UNSPECIFIED. ) 
 CURVE ( )  GEOMETRIC_REPRESENTATION_ITEM ( )  RATIONAL_B_SPLINE_CURVE ( ( 0.9330127018922194093, 0.9330127018922196314, 1.000000000000000000, 0.8660254037844387076, 1.000000000000000000, 0.8660254037844387076, 1.000000000000000000, 0.9330127018922194093, 0.9330127018922194093 ) ) 
 REPRESENTATION_ITEM ( '' )  );
#31594 = CARTESIAN_POINT ( 'NONE',  ( 7.321875000614516793, 3.027376345333611329, 5.243569643749999010 ) ) ;
#31595 = CARTESIAN_POINT ( 'NONE',  ( 24.00937500061451502, 0.000000000000000000, 5.243569643749999010 ) ) ;
#31596 =( BOUNDED_CURVE ( )  B_SPLINE_CURVE ( 2, ( #9631, #32165, #66143, #33612, #66888, #12169, #57226 ),
 .UNSPECIFIED., .F., .F. ) 
 B_SPLINE_CURVE_WITH_KNOTS ( ( 3, 2, 2, 3 ),
 ( 0.4750000000000000333, 0.4777777777777778567, 0.4805555555555556246, 0.4833333333333333925 ),
 .UNSPECIFIED. ) 
 CURVE ( )  GEOMETRIC_REPRESENTATION_ITEM ( )  RATIONAL_B_SPLINE_CURVE ( ( 0.9999999999999973355, 0.8660254037844413721, 1.000000000000000000, 0.8660254037844387076, 1.000000000000000000, 0.8660254037844360431, 1.000000000000002665 ) ) 
 REPRESENTATION_ITEM ( '' )  );
#31597 = CARTESIAN_POINT ( 'NONE',  ( 4.324156358178267823, -2.510600649150880770, -4.568139011954959194 ) ) ;
#31598 = CARTESIAN_POINT ( 'NONE',  ( 17.87812500061451715, 6.421520780324663323E-16, -5.243569643749999010 ) ) ;
#31599 = CARTESIAN_POINT ( 'NONE',  ( 23.78437500061451360, 6.421520780324663323E-16, -5.243569643749999010 ) ) ;
#31600 = CARTESIAN_POINT ( 'NONE',  ( 3.756430356250000102, 19.95312499938548356, 30.00000000000000000 ) ) ;
#31601 = CARTESIAN_POINT ( 'NONE',  ( 12.52500000122903145, 2.886751345948126879, 4.999999999999998224 ) ) ;
#31602 = CYLINDRICAL_SURFACE ( 'NONE', #32446, 4.999999999999998224 ) ;
#31603 = CARTESIAN_POINT ( 'NONE',  ( 4.884375000614518569, 6.421520780324663323E-16, -5.243569643749999010 ) ) ;
#31604 = CARTESIAN_POINT ( 'NONE',  ( 17.95312500061451644, 4.541064518000418104, -2.621784821874998173 ) ) ;
#31605 = CARTESIAN_POINT ( 'NONE',  ( 12.79687500061451821, -3.027376345333614438, 5.243569643749998122 ) ) ;
#31606 = ORIENTED_EDGE ( 'NONE', *, *, #3230, .T. ) ;
#31607 = CARTESIAN_POINT ( 'NONE',  ( 22.16250000000000142, 2.886751345948095793, -5.000000000000055067 ) ) ;
#31608 = CARTESIAN_POINT ( 'NONE',  ( 25.67812500061451431, 4.541064518000418104, 2.621784821874999949 ) ) ;
#31609 = DIRECTION ( 'NONE',  ( -0.000000000000000000, -1.000000000000000000, -0.000000000000000000 ) ) ;
#31610 = CARTESIAN_POINT ( 'NONE',  ( -2.000000000000000000, 18.23750000122903359, 26.53589838486224650 ) ) ;
#31611 = ADVANCED_FACE ( 'NONE', ( #371 ), #39902, .T. ) ;
#31612 = CARTESIAN_POINT ( 'NONE',  ( 14.58750000000000036, 5.773502691896255534, 3.535250795749688894E-16 ) ) ;
#31613 = CARTESIAN_POINT ( 'NONE',  ( 24.30000000122903359, -2.886751345948129988, 4.999999999999997335 ) ) ;
#31614 = CARTESIAN_POINT ( 'NONE',  ( 18.77812500061451573, 6.421520780324663323E-16, -5.243569643749999010 ) ) ;
#31615 = ORIENTED_EDGE ( 'NONE', *, *, #26754, .T. ) ;
#31616 = CARTESIAN_POINT ( 'NONE',  ( 22.08749999999999858, -2.886751345948125991, -5.000000000000000000 ) ) ;
#31617 = CARTESIAN_POINT ( 'NONE',  ( 23.55937500061451573, 0.000000000000000000, 5.243569643749999010 ) ) ;
#31618 =( BOUNDED_CURVE ( )  B_SPLINE_CURVE ( 2, ( #60940, #49509, #38792, #8885, #27340, #44341, #21413 ),
 .UNSPECIFIED., .F., .T. ) 
 B_SPLINE_CURVE_WITH_KNOTS ( ( 3, 2, 2, 3 ),
 ( 0.6166666666666666963, 0.6194444444444444642, 0.6222222222222222321, 0.6250000000000000000 ),
 .UNSPECIFIED. ) 
 CURVE ( )  GEOMETRIC_REPRESENTATION_ITEM ( )  RATIONAL_B_SPLINE_CURVE ( ( 1.000000000000000000, 0.8660254037844387076, 1.000000000000000000, 0.8660254037844387076, 1.000000000000000000, 0.8660254037844387076, 1.000000000000000000 ) ) 
 REPRESENTATION_ITEM ( '' )  );
#31619 = VERTEX_POINT ( 'NONE', #40256 ) ;
#31620 = CARTESIAN_POINT ( 'NONE',  ( 11.58750000000000036, -2.886751345948074920, 5.000000000000092371 ) ) ;
#31621 = CARTESIAN_POINT ( 'NONE',  ( 11.12812500061451715, 6.421520780324663323E-16, -5.243569643749999010 ) ) ;
#31622 = CARTESIAN_POINT ( 'NONE',  ( 4.678125000614516971, -4.541064518000419881, 2.621784821874995952 ) ) ;
#31623 = CARTESIAN_POINT ( 'NONE',  ( 17.37187500061451573, 5.824947211148865298E-16, -4.756430356249998326 ) ) ;
#31624 = CARTESIAN_POINT ( 'NONE',  ( 26.65312500061451573, 0.000000000000000000, 5.243569643749999010 ) ) ;
#31625 = CARTESIAN_POINT ( 'NONE',  ( 19.68750000000000355, -2.886751345948129988, 4.999999999999997335 ) ) ;
#31626 = CARTESIAN_POINT ( 'NONE',  ( 27.37500000000000000, -4.330127018922194537, 2.499999999999995559 ) ) ;
#31627 = CARTESIAN_POINT ( 'NONE',  ( 3.384375000614517237, -4.541064518000419881, 2.621784821874995952 ) ) ;
#31628 = CARTESIAN_POINT ( 'NONE',  ( 7.771875000614516971, 3.027376345333611329, 5.243569643749999010 ) ) ;
#31629 = CARTESIAN_POINT ( 'NONE',  ( 17.70937500061451431, 0.000000000000000000, 5.243569643749999010 ) ) ;
#31630 = CARTESIAN_POINT ( 'NONE',  ( -3.999999999999999112, 13.81250000122903465, 30.00000000000000000 ) ) ;
#31631 = VERTEX_POINT ( 'NONE', #67970 ) ;
#31632 = CARTESIAN_POINT ( 'NONE',  ( 25.86562500061451431, -6.054752690667223547, -1.112240025338166033E-15 ) ) ;
#31633 = CARTESIAN_POINT ( 'NONE',  ( 28.35937500061451289, 4.541064518000418104, -2.621784821874998173 ) ) ;
#31634 = CARTESIAN_POINT ( 'NONE',  ( 7.387500001229032165, 6.123233995736764310E-16, -4.999999999999998224 ) ) ;
#31635 = VECTOR ( 'NONE', #39156, 1000.000000000000000 ) ;
#31636 = CARTESIAN_POINT ( 'NONE',  ( 15.52500000000000036, 4.330127018922191873, 2.499999999999999556 ) ) ;
#31637 = CARTESIAN_POINT ( 'NONE',  ( 12.02812500061451573, 6.421520780324663323E-16, -5.243569643749999010 ) ) ;
#31638 = CARTESIAN_POINT ( 'NONE',  ( 25.78125000122903288, 6.123233995736764310E-16, -4.999999999999998224 ) ) ;
#31639 = CARTESIAN_POINT ( 'NONE',  ( -2.000000000000001776, 18.14374999877096428, 33.46410161513775705 ) ) ;
#31640 = CARTESIAN_POINT ( 'NONE',  ( 28.15312500061451573, -4.541064518000417216, -2.621784821875001281 ) ) ;
#31641 = CARTESIAN_POINT ( 'NONE',  ( 17.25000000122903288, -2.886751345948125991, -5.000000000000000000 ) ) ;
#31642 = CARTESIAN_POINT ( 'NONE',  ( 27.05625000122903145, -4.330127018922190985, -2.500000000000001332 ) ) ;
#31643 = CARTESIAN_POINT ( 'NONE',  ( 17.18437500061451573, 4.119189519843966529, 2.378215178124999607 ) ) ;
#31644 = CARTESIAN_POINT ( 'NONE',  ( 4.715625000614516615, -6.054752690667223547, -1.112240025338166033E-15 ) ) ;
#31645 = CARTESIAN_POINT ( 'NONE',  ( 22.05937500061451573, 4.541064518000418104, -2.621784821874998173 ) ) ;
#31646 = CARTESIAN_POINT ( 'NONE',  ( 4.243569643749999898, 17.79687500061451999, 32.45002607614398471 ) ) ;
#31647 = CARTESIAN_POINT ( 'NONE',  ( 24.15937500061451715, -4.541064518000417216, -2.621784821875001281 ) ) ;
#31648 = CARTESIAN_POINT ( 'NONE',  ( 4.949999999999999289, -4.330127018922190985, -2.500000000000001332 ) ) ;
#31649 = CARTESIAN_POINT ( 'NONE',  ( 4.000000000000000000, 11.75000000122903643, 32.30940107675849049 ) ) ;
#31650 = CARTESIAN_POINT ( 'NONE',  ( 13.07812500061451821, 4.541064518000418104, 2.621784821874999949 ) ) ;
#31651 = CARTESIAN_POINT ( 'NONE',  ( 4.762500001229033941, 4.330127018922192761, -2.499999999999997780 ) ) ;
#31652 = CARTESIAN_POINT ( 'NONE',  ( 9.346875000614517148, -3.027376345333610441, -5.243569643749999898 ) ) ;
#31653 = CYLINDRICAL_SURFACE ( 'NONE', #52523, 4.999999999999998224 ) ;
#31654 = CARTESIAN_POINT ( 'NONE',  ( 9.703125000614514661, -4.541064518000417216, -2.621784821875001281 ) ) ;
#31655 = CARTESIAN_POINT ( 'NONE',  ( 14.59687500061452070, -3.027376345333614438, 5.243569643749998122 ) ) ;
#31656 = CARTESIAN_POINT ( 'NONE',  ( 20.96250000122903145, 4.330127018922192761, -2.499999999999997780 ) ) ;
#31657 = CARTESIAN_POINT ( 'NONE',  ( 10.69687500061451679, -3.027376345333610441, -5.243569643749999898 ) ) ;
#31658 = CARTESIAN_POINT ( 'NONE',  ( 11.72812500061451857, 4.541064518000418104, 2.621784821874999949 ) ) ;
#31659 = CARTESIAN_POINT ( 'NONE',  ( 28.81875000122903074, -5.773502691896255534, -1.060575238724906372E-15 ) ) ;
#31660 = CARTESIAN_POINT ( 'NONE',  ( 20.48437500061451289, -4.541064518000419881, 2.621784821874995952 ) ) ;
#31661 = CARTESIAN_POINT ( 'NONE',  ( 29.92968750030725644, 0.000000000000000000, 4.878215178124998275 ) ) ;
#31662 = CARTESIAN_POINT ( 'NONE',  ( -0.2761983717765542079, 4.994289515549795944, 33.99286899158064301 ) ) ;
#31663 = CYLINDRICAL_SURFACE ( 'NONE', #47850, 3.999999999999996447 ) ;
#31664 = ADVANCED_FACE ( 'NONE', ( #11814 ), #34331, .F. ) ;
#31665 = CARTESIAN_POINT ( 'NONE',  ( 4.243569643749999010, 15.17187500061451644, -32.45002607614398471 ) ) ;
#31666 = CARTESIAN_POINT ( 'NONE',  ( 16.38750000122903216, 6.123233995736764310E-16, -4.999999999999998224 ) ) ;
#31667 = CARTESIAN_POINT ( 'NONE',  ( 9.534375000614517148, 4.541064518000418104, 2.621784821874999949 ) ) ;
#31668 = CARTESIAN_POINT ( 'NONE',  ( 2.121784821874999061, 17.85312500061451502, -33.67503911421598417 ) ) ;
#31669 = CARTESIAN_POINT ( 'NONE',  ( 17.02500000122903145, 2.886751345948126879, 4.999999999999999112 ) ) ;
#31670 = CARTESIAN_POINT ( 'NONE',  ( 13.52812500061451750, 4.541064518000418104, 2.621784821874999949 ) ) ;
#31671 = ORIENTED_EDGE ( 'NONE', *, *, #13788, .T. ) ;
#31672 = CARTESIAN_POINT ( 'NONE',  ( 16.91250000000000142, 2.886751345948126879, 4.999999999999999112 ) ) ;
#31673 = CARTESIAN_POINT ( 'NONE',  ( 16.50000000000000000, 0.000000000000000000, 4.999999999999998224 ) ) ;
#31674 = CARTESIAN_POINT ( 'NONE',  ( 11.25937500061451679, 4.541064518000418104, -2.621784821874998173 ) ) ;
#31675 = CARTESIAN_POINT ( 'NONE',  ( 17.84999999999999787, 0.000000000000000000, 4.999999999999998224 ) ) ;
#31676 = CARTESIAN_POINT ( 'NONE',  ( 13.72500000122903074, 2.886751345948129099, -4.999999999999998224 ) ) ;
#31677 = CARTESIAN_POINT ( 'NONE',  ( 20.21250000122903145, 0.000000000000000000, 4.999999999999998224 ) ) ;
#31678 = CARTESIAN_POINT ( 'NONE',  ( 18.77812500061451573, 6.421520780324663323E-16, -5.243569643749999010 ) ) ;
#31679 = CARTESIAN_POINT ( 'NONE',  ( 20.42812500061451431, -4.541064518000419881, 2.621784821874995952 ) ) ;
#31680 = CARTESIAN_POINT ( 'NONE',  ( 28.95000000122903572, -2.886751345948125991, -5.000000000000000000 ) ) ;
#31681 = CARTESIAN_POINT ( 'NONE',  ( 4.453125000614517326, 4.541064518000418104, -2.621784821874998173 ) ) ;
#31682 = CARTESIAN_POINT ( 'NONE',  ( 24.56250000000000000, 2.886751345948126879, 4.999999999999999112 ) ) ;
#31683 = DIRECTION ( 'NONE',  ( 0.000000000000000000, 0.000000000000000000, 1.000000000000000000 ) ) ;
#31684 = CARTESIAN_POINT ( 'NONE',  ( 7.659375000614518036, 4.119189519843966529, -2.378215178124998275 ) ) ;
#31685 = CARTESIAN_POINT ( 'NONE',  ( 27.94687500061451502, 6.054752690667223547, 3.707466751127219781E-16 ) ) ;
#31686 = CARTESIAN_POINT ( 'NONE',  ( 4.837500001229035895, 4.330127018922191873, 2.499999999999999556 ) ) ;
#31687 = CARTESIAN_POINT ( 'NONE',  ( 29.44687500061451857, -3.027376345333614438, 5.243569643749998122 ) ) ;
#31688 = CARTESIAN_POINT ( 'NONE',  ( 22.80000000000000071, 0.000000000000000000, 4.999999999999998224 ) ) ;
#31689 = CARTESIAN_POINT ( 'NONE',  ( 7.321875000614516793, 3.027376345333611329, 5.243569643749999010 ) ) ;
#31690 = CARTESIAN_POINT ( 'NONE',  ( 26.80312500061451431, -4.541064518000417216, -2.621784821875001281 ) ) ;
#31691 = CARTESIAN_POINT ( 'NONE',  ( -7.967954043666661671E-16, 13.09062499938548285, 34.33755215474603517 ) ) ;
#31692 = CYLINDRICAL_SURFACE ( 'NONE', #29122, 9.000000000000000000 ) ;
#31693 = CARTESIAN_POINT ( 'NONE',  ( 27.58125000122903359, 6.123233995736764310E-16, -4.999999999999998224 ) ) ;
#31694 = CARTESIAN_POINT ( 'NONE',  ( 4.846875000614519813, -3.027376345333610441, -5.243569643749999898 ) ) ;
#31695 = CARTESIAN_POINT ( 'NONE',  ( 9.121875000614517504, 3.027376345333611329, 5.243569643749999010 ) ) ;
#31696 = CARTESIAN_POINT ( 'NONE',  ( 3.637500000000001954, -2.886751345948125991, -5.000000000000000000 ) ) ;
#31697 = CARTESIAN_POINT ( 'NONE',  ( -4.243569643749999898, 12.56562500061459531, 27.54997392385601529 ) ) ;
#31698 = CARTESIAN_POINT ( 'NONE',  ( 20.77500000000000213, 6.123233995736764310E-16, -4.999999999999998224 ) ) ;
#31699 = CARTESIAN_POINT ( 'NONE',  ( -1.999999999999997113, 17.82499999999999929, -26.53589838486224295 ) ) ;
#31700 = CARTESIAN_POINT ( 'NONE',  ( 5.250000000000000888, 0.000000000000000000, 4.999999999999998224 ) ) ;
#31701 = CARTESIAN_POINT ( 'NONE',  ( 15.04687500061451466, -4.119189519843965641, -2.378215178125001383 ) ) ;
#31702 = VERTEX_POINT ( 'NONE', #13979 ) ;
#31703 = CARTESIAN_POINT ( 'NONE',  ( 20.61562500061451431, 3.027376345333613106, -5.243569643749998122 ) ) ;
#31704 = CARTESIAN_POINT ( 'NONE',  ( 9.740625000614516082, -3.027376345333610441, -5.243569643749999898 ) ) ;
#31705 = CARTESIAN_POINT ( 'NONE',  ( 22.95937500061451786, 2.746126346562643317, 4.756430356249998326 ) ) ;
#31706 = CARTESIAN_POINT ( 'NONE',  ( 7.509375000614517681, -4.541064518000417216, -2.621784821875001281 ) ) ;
#31707 = CARTESIAN_POINT ( 'NONE',  ( 23.25000000000000000, 0.000000000000000000, 4.999999999999998224 ) ) ;
#31708 = CARTESIAN_POINT ( 'NONE',  ( 19.01250000122903216, -4.330127018922190985, -2.500000000000001332 ) ) ;
#31709 = CARTESIAN_POINT ( 'NONE',  ( 27.17812500061451786, -4.541064518000419881, 2.621784821874995952 ) ) ;
#31710 = CARTESIAN_POINT ( 'NONE',  ( 4.000000000000000000, 10.85000000122903430, 32.30940107675849760 ) ) ;
#31711 = CARTESIAN_POINT ( 'NONE',  ( 8.821875000614518569, -6.054752690667223547, -1.112240025338166033E-15 ) ) ;
#31712 = CARTESIAN_POINT ( 'NONE',  ( 13.92187500061451644, 3.027376345333613106, -5.243569643749998122 ) ) ;
#31713 = CARTESIAN_POINT ( 'NONE',  ( 24.23437500061451644, 6.421520780324663323E-16, -5.243569643749999010 ) ) ;
#31714 = CARTESIAN_POINT ( 'NONE',  ( 3.734827092922140768, -3.324314453528163682, -3.734827092927292203 ) ) ;
#31715 = CARTESIAN_POINT ( 'NONE',  ( 12.44999999999999929, 0.000000000000000000, 4.999999999999998224 ) ) ;
#31716 = CARTESIAN_POINT ( 'NONE',  ( 19.32187500061451857, 3.027376345333613106, -5.243569643749998122 ) ) ;
#31717 = CARTESIAN_POINT ( 'NONE',  ( 9.046875000614518214, 6.054752690667223547, 3.707466751127219781E-16 ) ) ;
#31718 = CARTESIAN_POINT ( 'NONE',  ( 2.655984681222220721E-16, 20.51562499938548356, 25.66244784525396483 ) ) ;
#31719 = CARTESIAN_POINT ( 'NONE',  ( 22.87500000000000000, -4.330127018922194537, 2.499999999999995559 ) ) ;
#31720 = CARTESIAN_POINT ( 'NONE',  ( -1.999999999999999112, 14.90000000000000036, 26.53589838486224650 ) ) ;
#31721 = CARTESIAN_POINT ( 'NONE',  ( -4.243569643749999898, 10.40937500061451892, -30.00000000000000000 ) ) ;
#31722 = CARTESIAN_POINT ( 'NONE',  ( 25.80937500061451928, 0.000000000000000000, 4.756430356249998326 ) ) ;
#31723 = CARTESIAN_POINT ( 'NONE',  ( 12.32812500061451821, -4.541064518000419881, 2.621784821874995952 ) ) ;
#31724 = CARTESIAN_POINT ( 'NONE',  ( 28.35937500061451289, 4.541064518000418104, -2.621784821874998173 ) ) ;
#31725 = CARTESIAN_POINT ( 'NONE',  ( -3.999999999999999112, 19.21250000122903501, -30.00000000000000000 ) ) ;
#31726 = PLANE ( 'NONE',  #17280 ) ;
#31727 = CARTESIAN_POINT ( 'NONE',  ( 11.40000000000000036, 4.330127018922192761, -2.499999999999997780 ) ) ;
#31728 = CARTESIAN_POINT ( 'NONE',  ( -3.999999999999997335, 17.90000000122903501, 32.30940107675850470 ) ) ;
#31729 = CARTESIAN_POINT ( 'NONE',  ( 10.46250000122903323, -4.330127018922190985, -2.500000000000001332 ) ) ;
#31730 = CARTESIAN_POINT ( 'NONE',  ( 21.68437500061451573, 4.541064518000418104, 2.621784821874999949 ) ) ;
#31731 = CARTESIAN_POINT ( 'NONE',  ( 17.37187500061451573, -6.054752690667223547, -1.112240025338166033E-15 ) ) ;
#31732 = CARTESIAN_POINT ( 'NONE',  ( 5.000000000000000000, 39.99999999999999289, 30.00000000000000000 ) ) ;
#31733 = ORIENTED_EDGE ( 'NONE', *, *, #38503, .F. ) ;
#31734 = CARTESIAN_POINT ( 'NONE',  ( 17.24062500061451786, -3.027376345333614438, 5.243569643749998122 ) ) ;
#31735 = CARTESIAN_POINT ( 'NONE',  ( 28.23750000122903359, 4.330127018922191873, 2.499999999999999556 ) ) ;
#31736 = CARTESIAN_POINT ( 'NONE',  ( 17.07187500061451502, 3.027376345333613106, -5.243569643749998122 ) ) ;
#31737 = CARTESIAN_POINT ( 'NONE',  ( 27.98437500061451289, 4.541064518000418104, 2.621784821874999949 ) ) ;
#31738 = CARTESIAN_POINT ( 'NONE',  ( 4.828125000614518214, 6.421520780324663323E-16, -5.243569643749999010 ) ) ;
#31739 = CARTESIAN_POINT ( 'NONE',  ( 20.39062500061451644, -3.027376345333614438, 5.243569643749998122 ) ) ;
#31740 = CARTESIAN_POINT ( 'NONE',  ( 29.14687500061451075, -3.027376345333610441, -5.243569643749999898 ) ) ;
#31741 = CARTESIAN_POINT ( 'NONE',  ( 2.121784821875001281, 12.75312500061451715, 33.67503911421598417 ) ) ;
#31742 = CARTESIAN_POINT ( 'NONE',  ( 16.91250000122903430, 4.330127018922192761, -2.499999999999997780 ) ) ;
#31743 = CARTESIAN_POINT ( 'NONE',  ( 8.784375000614518925, -4.119189519843968306, 2.378215178124996054 ) ) ;
#31744 = ADVANCED_FACE ( 'NONE', ( #46520 ), #8442, .T. ) ;
#31745 = CARTESIAN_POINT ( 'NONE',  ( 7.903125000614515727, -4.541064518000417216, -2.621784821875001281 ) ) ;
#31746 = CARTESIAN_POINT ( 'NONE',  ( 27.96562500061451928, 3.027376345333611329, 5.243569643749999010 ) ) ;
#31747 = CARTESIAN_POINT ( 'NONE',  ( 9.787500001229036073, 4.330127018922191873, 2.499999999999999556 ) ) ;
#31748 = CARTESIAN_POINT ( 'NONE',  ( 22.24687500061451217, -3.027376345333614438, 5.243569643749998122 ) ) ;
#31749 = CARTESIAN_POINT ( 'NONE',  ( 11.61562500061451608, 3.027376345333613106, -5.243569643749998122 ) ) ;
#31750 = CARTESIAN_POINT ( 'NONE',  ( 23.10000000122903074, -2.886751345948125991, -5.000000000000000000 ) ) ;
#31751 = EDGE_CURVE ( 'NONE', #1870, #24236, #9392, .T. ) ;
#31752 = CARTESIAN_POINT ( 'NONE',  ( 23.54062500061451146, -3.027376345333614438, 5.243569643749998122 ) ) ;
#31753 = CARTESIAN_POINT ( 'NONE',  ( 18.64687500061451786, -3.027376345333614438, 5.243569643749998122 ) ) ;
#31754 = CARTESIAN_POINT ( 'NONE',  ( 13.34062500061451750, -3.027376345333610441, -5.243569643749999898 ) ) ;
#31755 = CARTESIAN_POINT ( 'NONE',  ( -4.243569643749997233, 15.39687500061451786, 32.45002607614398471 ) ) ;
#31756 = CARTESIAN_POINT ( 'NONE',  ( 19.60312500061451502, -4.541064518000417216, -2.621784821875001281 ) ) ;
#31757 = CARTESIAN_POINT ( 'NONE',  ( -1.071796769724490339, 17.58259618943233349, 26.00000000000000000 ) ) ;
#31758 = ORIENTED_EDGE ( 'NONE', *, *, #1146, .T. ) ;
#31759 = EDGE_LOOP ( 'NONE', ( #2626, #62075, #48034, #26025 ) ) ;
#31760 = CARTESIAN_POINT ( 'NONE',  ( 21.78750000000000142, 5.773502691896255534, 3.535250795749688894E-16 ) ) ;
#31761 = CARTESIAN_POINT ( 'NONE',  ( 4.243569643749999898, 19.63437500061451857, -30.00000000000000000 ) ) ;
#31762 = CARTESIAN_POINT ( 'NONE',  ( 1.071796769724488119, 17.99509619066137134, 33.99999999999999289 ) ) ;
#31763 = CARTESIAN_POINT ( 'NONE',  ( 26.57812500061451644, 4.541064518000418104, 2.621784821874999949 ) ) ;
#31764 = CARTESIAN_POINT ( 'NONE',  ( 5.878125000614517148, 4.541064518000418104, 2.621784821874999949 ) ) ;
#31765 = CARTESIAN_POINT ( 'NONE',  ( 18.93750000122903288, -4.330127018922194537, 2.499999999999995559 ) ) ;
#31766 = CARTESIAN_POINT ( 'NONE',  ( 25.64062500061451644, 6.054752690667223547, 3.707466751127219781E-16 ) ) ;
#31767 = CARTESIAN_POINT ( 'NONE',  ( 23.96249999999999858, 2.886751345948129099, -4.999999999999998224 ) ) ;
#31768 = EDGE_CURVE ( 'NONE', #7627, #6226, #34842, .T. ) ;
#31769 = CARTESIAN_POINT ( 'NONE',  ( 27.92812500061451431, 4.541064518000418104, 2.621784821874999949 ) ) ;
#31770 = CARTESIAN_POINT ( 'NONE',  ( 8.503125000614515372, 4.541064518000418104, -2.621784821874998173 ) ) ;
#31771 = VERTEX_POINT ( 'NONE', #25061 ) ;
#31772 = CARTESIAN_POINT ( 'NONE',  ( 22.67812500061451431, -4.541064518000419881, 2.621784821874995952 ) ) ;
#31773 = CARTESIAN_POINT ( 'NONE',  ( 5.990625000614517859, -3.027376345333614438, 5.243569643749998122 ) ) ;
#31774 = CARTESIAN_POINT ( 'NONE',  ( 14.03437500061451715, 4.119189519843966529, 2.378215178124999607 ) ) ;
#31775 = CARTESIAN_POINT ( 'NONE',  ( 2.803125000614518747, 0.000000000000000000, 5.243569643749999010 ) ) ;
#31776 = CARTESIAN_POINT ( 'NONE',  ( -2.000000000000000000, 14.18750000122903288, -33.46410161513775705 ) ) ;
#31777 = CARTESIAN_POINT ( 'NONE',  ( 11.58750000000000036, -2.886751345948129988, 4.999999999999997335 ) ) ;
#31778 = CARTESIAN_POINT ( 'NONE',  ( 10.09687500061451715, -3.027376345333614438, 5.243569643749998122 ) ) ;
#31779 = CARTESIAN_POINT ( 'NONE',  ( 6.300000001229033586, -2.886751345948129988, 4.999999999999997335 ) ) ;
#31780 = CARTESIAN_POINT ( 'NONE',  ( 13.95937500061451786, 4.541064518000418104, -2.621784821874998173 ) ) ;
#31781 = CARTESIAN_POINT ( 'NONE',  ( 15.59999999999999964, 0.000000000000000000, 4.999999999999998224 ) ) ;
#31782 = CARTESIAN_POINT ( 'NONE',  ( 5.821875000614519458, 3.027376345333613106, -5.243569643749998122 ) ) ;
#31783 = CARTESIAN_POINT ( 'NONE',  ( -4.243569643749999898, 9.865625000614517859, -32.45002607614398471 ) ) ;
#31784 = DIRECTION ( 'NONE',  ( 0.000000000000000000, 0.000000000000000000, 1.000000000000000000 ) ) ;
#31785 = CARTESIAN_POINT ( 'NONE',  ( 11.93437500061451573, -4.541064518000419881, 2.621784821874995952 ) ) ;
#31786 = CYLINDRICAL_SURFACE ( 'NONE', #54808, 3.999999999999996447 ) ;
#31787 = CARTESIAN_POINT ( 'NONE',  ( 21.29062500061451502, -3.027376345333614438, 5.243569643749998122 ) ) ;
#31788 = CARTESIAN_POINT ( 'NONE',  ( 4.243569643749999010, 11.12187500061451928, 27.54997392385601174 ) ) ;
#31789 = CARTESIAN_POINT ( 'NONE',  ( 9.001249775931846008E-16, 18.56562500061459531, 34.90005215228797653 ) ) ;
#31790 = CARTESIAN_POINT ( 'NONE',  ( 25.24687500061451573, 6.054752690667223547, 3.707466751127219781E-16 ) ) ;
#31791 = LINE ( 'NONE', #60574, #70742 ) ;
#31792 = CARTESIAN_POINT ( 'NONE',  ( 3.815625000614518036, -6.054752690667223547, -1.112240025338166033E-15 ) ) ;
#31793 = CARTESIAN_POINT ( 'NONE',  ( 23.40937500061451715, 2.746126346562643317, 4.756430356249998326 ) ) ;
#31794 = CARTESIAN_POINT ( 'NONE',  ( 14.48437500061451821, 4.541064518000418104, 2.621784821874999949 ) ) ;
#31795 = CARTESIAN_POINT ( 'NONE',  ( 29.92500000000000071, 4.330127018922191873, 2.499999999999999556 ) ) ;
#31796 = CARTESIAN_POINT ( 'NONE',  ( 28.16250000122903074, 4.330127018922192761, -2.499999999999997780 ) ) ;
#31797 = CARTESIAN_POINT ( 'NONE',  ( 4.996875000614516615, 6.054752690667223547, 3.707466751127219781E-16 ) ) ;
#31798 = CARTESIAN_POINT ( 'NONE',  ( 17.74687500061451928, -3.027376345333614438, 5.243569643749998122 ) ) ;
#31799 = CARTESIAN_POINT ( 'NONE',  ( 1.071796769724491227, 17.93615380933863079, 26.00000000000000000 ) ) ;
#31800 = CARTESIAN_POINT ( 'NONE',  ( 24.11249999999999716, 2.886751345948126879, 4.999999999999999112 ) ) ;
#31801 = CARTESIAN_POINT ( 'NONE',  ( 2.962500001229034119, 4.330127018922192761, -2.499999999999997780 ) ) ;
#31802 = CARTESIAN_POINT ( 'NONE',  ( 26.07187500061451857, 3.027376345333613106, -5.243569643749998122 ) ) ;
#31803 = CARTESIAN_POINT ( 'NONE',  ( -1.878215178124999163, 14.70312499938548356, 26.74683588394047007 ) ) ;
#31804 = CARTESIAN_POINT ( 'NONE',  ( 14.32500000122903216, 2.886751345948193936, 4.999999999999883649 ) ) ;
#31805 = CARTESIAN_POINT ( 'NONE',  ( 8.137500000000002842, -2.886751345948125991, -5.000000000000000000 ) ) ;
#31806 = CARTESIAN_POINT ( 'NONE',  ( 9.421875000614514661, 4.119189519843966529, 2.378215178124999607 ) ) ;
#31807 = CARTESIAN_POINT ( 'NONE',  ( 21.89062500061451289, -3.027376345333610441, -5.243569643749999898 ) ) ;
#31808 = CARTESIAN_POINT ( 'NONE',  ( 11.40000000000000036, 4.330127018922192761, -2.499999999999997780 ) ) ;
#31809 = CARTESIAN_POINT ( 'NONE',  ( 4.003125000614518925, 4.541064518000418104, -2.621784821874998173 ) ) ;
#31810 = CARTESIAN_POINT ( 'NONE',  ( 20.40000000000000213, 4.330127018922192761, -2.499999999999997780 ) ) ;
#31811 = CARTESIAN_POINT ( 'NONE',  ( 17.91562500061451502, 3.027376345333613106, -5.243569643749998122 ) ) ;
#31812 = CARTESIAN_POINT ( 'NONE',  ( -2.000000000000000000, 18.68750000122903288, 26.53589838486224650 ) ) ;
#31813 = CARTESIAN_POINT ( 'NONE',  ( 22.76250000122903216, 4.330127018922192761, -2.499999999999997780 ) ) ;
#31814 = CARTESIAN_POINT ( 'NONE',  ( -1.878215178125001827, 19.24062499938548143, 33.25316411605952283 ) ) ;
#31815 = CARTESIAN_POINT ( 'NONE',  ( 29.70937500061451431, 4.541064518000418104, -2.621784821874998173 ) ) ;
#31816 = VERTEX_POINT ( 'NONE', #70134 ) ;
#31817 = CARTESIAN_POINT ( 'NONE',  ( 19.64062500061451644, -3.027376345333610441, -5.243569643749999898 ) ) ;
#31818 = CARTESIAN_POINT ( 'NONE',  ( 24.92812500061451431, -4.541064518000419881, 2.621784821874995952 ) ) ;
#31819 = CARTESIAN_POINT ( 'NONE',  ( 25.47187500061451715, -6.054752690667223547, -1.112240025338166033E-15 ) ) ;
#31820 = CARTESIAN_POINT ( 'NONE',  ( 9.487500000000000711, -2.886751345948125991, -5.000000000000000000 ) ) ;
#31821 = CARTESIAN_POINT ( 'NONE',  ( 12.40312500061451573, -4.541064518000417216, -2.621784821875001281 ) ) ;
#31822 = CARTESIAN_POINT ( 'NONE',  ( 25.90312500061451573, -4.541064518000417216, -2.621784821875001281 ) ) ;
#31823 = CARTESIAN_POINT ( 'NONE',  ( 17.59687500061451715, 6.054752690667223547, 3.707466751127219781E-16 ) ) ;
#31824 = CARTESIAN_POINT ( 'NONE',  ( 7.978125000614517681, 6.421520780324663323E-16, -5.243569643749999010 ) ) ;
#31825 = CYLINDRICAL_SURFACE ( 'NONE', #46307, 1.500000000000000444 ) ;
#31826 = CARTESIAN_POINT ( 'NONE',  ( -4.243569643749999898, 10.85937500061451821, 30.00000000000000000 ) ) ;
#31827 = CARTESIAN_POINT ( 'NONE',  ( 23.02500000122903145, -5.773502691896255534, -1.060575238724906372E-15 ) ) ;
#31828 = CARTESIAN_POINT ( 'NONE',  ( 16.13437500061451502, 5.824947211148865298E-16, -4.756430356249998326 ) ) ;
#31829 = CARTESIAN_POINT ( 'NONE',  ( 14.91562500061451679, 3.027376345333611329, 5.243569643749999010 ) ) ;
#31830 = CARTESIAN_POINT ( 'NONE',  ( 8.184375000614515727, 4.541064518000418104, 2.621784821874999949 ) ) ;
#31831 = CARTESIAN_POINT ( 'NONE',  ( 6.196875000614515905, -3.027376345333610441, -5.243569643749999898 ) ) ;
#31832 = ORIENTED_EDGE ( 'NONE', *, *, #22734, .F. ) ;
#31833 = CARTESIAN_POINT ( 'NONE',  ( -4.112406224592624504, 9.116497278081070021, 34.37320649897247193 ) ) ;
#31834 = CARTESIAN_POINT ( 'NONE',  ( 22.00312500061451360, 4.541064518000418104, -2.621784821874998173 ) ) ;
#31835 =( BOUNDED_SURFACE ( )  B_SPLINE_SURFACE ( 1, 2, ( 
 ( #16186, #55720, #33181, #50184, #67183, #39458, #72712, #22095, #4397, #10290, #28366, #72343, #61613, #16544, #67540, #39096, #11381, #60885, #49819, #5478, #4752, #26926, #11015, #17269, #44653, #33536, #43913, #5114, #33900, #56086, #61979, #28017, #27648, #50545, #32456, #49451, #66813, #67897, #9918, #16903, #38358, #73073, #21724, #27285, #22454, #44283, #56444, #5834, #50902, #32820, #39830, #38737, #301, #71985, #22811, #61257, #45362, #54991, #21359, #66438, #63786, #19073, #62345, #17626, #51631, #11741, #30180, #2117, #51265, #18710, #1032, #29454, #23901, #40919, #52711, #12464, #24629, #6924, #51991, #57876, #23538, #69707, #1392, #46815, #47174, #46449, #29096, #1753, #6564, #34258, #7286, #29815, #68987, #52350, #69353, #18344, #56791, #24266, #28724, #40186, #63431, #6196, #46088, #12818, #41275, #68624, #35352, #63061, #13176, #17986, #57523, #40545, #35715, #667, #58237, #7642, #23175, #45729, #34994, #68264, #62707, #12101, #34622, #57153, #64886, #54180, #13912, #53814, #36812, #36451, #20172, #48273, #36084, #8738, #70797, #25363, #42726, #65247, #9109, #14274, #14636, #58604, #58965, #54542, #2834, #59327, #19811, #13536, #24992, #25736, #30902, #37177, #31647, #53444, #31271, #8373, #41999, #59702, #47907, #3576, #20535, #43091, #64149, #26099, #3207, #8011, #48637, #2468, #9478, #64519, #41630, #71162, #65619, #15007, #70436, #42364, #30546, #53073, #26467, #37544, #60066, #32007, #3944, #49006, #71537, #47536, #70065, #19438, #60799, #33456, #38271, #5756, #16458, #61531, #33098, #39016, #5394, #27568, #15369, #10929, #60428, #71903, #10570, #37911, #10205, #55637, #50464, #55277, #5031, #21642, #27931, #32740, #16101, #4672, #67100, #56366, #56000, #72992, #44925, #22373, #27202, #67461, #66730, #16824, #28290, #49737, #44199, #39378, #66355, #50100, #38651, #15732, #72630, #22014, #9839, #61175, #44570, #72264, #61897, #11302, #33823, #50821, #20912, #32368, #43464, #65988, #54906, #4314, #26839, #49373, #21276, #43830, #62620, #29373, #63344, #12016, #23457, #40106, #586, #1304, #6476, #12730, #52264, #1666, #22729, #40828, #17900, #39749, #68539, #34176, #41189, #23091, #224, #7197, #35266, #51905, #45648, #34539, #67816, #45282, #58148, #57788, #34907, #17189, #24175, #6113, #29726, #29011, #57069, #46727, #69262, #30087, #62266, #28644, #51548, #11661, #63698, #13089, #56712, #18624, #949, #40460, #57435, #23813, #35627, #46003, #7553, #62976, #51182, #12372, #68182, #46364, #17545, #68898, #6838, #18255, #2030, #47086, #36360, #37458, #52625, #14548, #7919, #70703, #19346, #47444, #42634, #69976, #54093, #47811, #2745, #30456, #9387, #52985, #69619, #65158, #20078, #58508, #25264, #41903, #2381, #53720, #65530, #70341, #19717, #31553, #59977, #64428, #24541, #25642, #18981, #42269, #14916, #24899, #3112, #48547, #64792, #71074, #14183, #13820, #41542, #9022, #59239, #8648, #37084, #58874, #36718, #8284, #64060, #59608, #31177, #30814, #13441, #48179, #3490, #35990, #20449, #26008, #53347, #42999, #43737, #4583, #50379, #10117, #66633, #44479, #26749, #67010, #37819, #22286, #26375, #15639, #16011, #49282, #33374, #48914, #71445, #67373, #16371, #4221, #32647, #38926, #72535, #31918, #4944, #44838, #61445, #49646, #55188, #61805, #38180, #27113, #72173, #21553, #38559, #10839, #44107, #61082, #20820, #32281, #72904, #21186, #10480, #33009, #55910, #55548, #5303, #9747, #71815, #27478, #66262, #43375, #50011, #39291, #21923, #27848, #60704, #16736, #54454, #3853, #65899, #15279, #60338, #54815, #28917, #11927, #41101, #17458, #56980, #34452, #51455, #68445, #40736, #858, #23365, #5670, #11574, #29638, #491, #62886, #17807, #46272, #40368, #12644, #62177, #51094, #6750, #6025, #28206, #12281, #18537, #45913, #34814, #45193, #6384, #35180, #57344, #63252, #29283, #51813, #1216, #33735, #50735, #68091, #69176, #11208, #68811, #39658, #23722, #23000, #28559, #18167, #45560, #57704, #7109, #52176, #34089, #56281, #56630, #137, #1578, #24087, #17098, #46634, #40016, #62530, #22643, #67725, #13732, #30727, #42546, #70987, #30370, #63611, #36632, #58059, #53259, #25923, #13356, #64708, #59520, #2657, #8933, #58788, #52899, #29994, #19993, #70254, #19627, #53629, #69890, #36274, #47358, #20363, #70619, #8198, #63973, #35539, #42183, #59154, #1944, #31463, #36997, #7468, #25552, #2297, #25175, #54006, #41810, #47716, #3021, #58421, #48095, #69534, #3402, #52535, #19255, #14092, #7833, #65073, #24450, #46999, #48463, #14464, #24812, #8562, #64340, #31090, #13002, #18893, #41455, #35897, #60994, #26663, #38468, #15551, #55463, #50294, #54730, #66175, #4855, #15191, #55100, #38094, #37729, #21464, #49560, #37370, #10026, #72081, #49197, #44018, #66540, #10393, #60617, #15920, #59893, #60249, #55825, #4133, #32562, #21100, #14828, #26288, #27029, #32197, #32925, #27389, #71730, #4500, #9664, #43289, #49921, #43651, #72445, #21829, #44394, #65437, #66919, #16288, #9298, #38843, #3764, #10755, #65809, #42914, #61358, #33286, #5213, #27754, #72817, #31831, #54369, #48825, #71356, #20730, #16647, #1131, #28119, #51730, #51004, #11482, #46186, #23640, #52090, #22200, #50648, #34005, #44754, #63165, #35095, #11116, #68725, #56542, #62444, #56893, #768, #12560, #45468, #57620, #39930, #11842, #17723, #5935, #29554, #34361, #6668, #7023, #6298, #62089, #34724, #39564, #67288, #40283, #62804, #28827, #12197, #29196, #51366, #39203, #57254, #61717, #52, #23276, #33645, #28469, #45826, #18085, #402, #68362, #22910, #40646, #56189, #5582, #67641, #68000, #22557, #45105, #17007, #17373, #64987, #8473, #19171, #2214, #31377, #7745, #47272, #24729, #41726, #58703, #31007, #64253, #13641, #69090, #1859, #19912, #63883, #53173, #8114, #36549, #30641 ),
 ( #59433, #64623, #36185, #18451, #53540, #7382, #2936, #30281, #13274, #25465, #48009, #1495, #24001, #29913, #35812, #46549, #42465, #14378, #63531, #70537, #58334, #2570, #25090, #47633, #36913, #69806, #8841, #70166, #19543, #42101, #52814, #41016, #14010, #59068, #12918, #35451, #41373, #57975, #18809, #52453, #24366, #46913, #69452, #73007, #39395, #61547, #48375, #22391, #20274, #31746, #44586, #70902, #43200, #67118, #11319, #15106, #16475, #54640, #61914, #71263, #50117, #65720, #27948, #17206, #50481, #44940, #5774, #67478, #37642, #16841, #26570, #33840, #62284, #60165, #4045, #56381, #26201, #39033, #54283, #20643, #28305, #48740, #42826, #10949, #11679, #22029, #33470, #14740, #72646, #50840, #56018, #240, #5410, #22748, #45299, #3311, #65350, #9575, #39767, #53918, #67833, #9210, #25838, #32107, #37282, #59804, #3677, #35644, #29390, #57452, #62638, #64077, #34558, #28662, #46746, #1683, #40123, #24558, #34195, #68915, #12748, #47104, #6856, #69636, #51924, #1321, #29744, #68557, #41559, #23830, #18642, #18998, #46381, #965, #69280, #51565, #56729, #52281, #24192, #18272, #41206, #63714, #40846, #51201, #13106, #603, #12033, #63364, #23109, #23475, #35284, #58166, #17916, #57806, #34925, #7570, #46021, #7215, #40479, #30106, #6131, #52640, #2047, #45666, #68199, #62994, #17562, #57086, #6494, #29029, #12389, #36738, #26026, #58893, #25662, #8667, #8303, #65177, #20096, #7936, #53740, #42653, #70361, #14568, #37101, #54109, #59258, #59627, #30474, #30833, #26393, #47831, #31198, #64812, #58526, #69994, #70721, #2763, #9040, #3507, #25285, #3133, #53366, #13838, #31570, #19738, #42288, #48565, #19363, #3870, #53003, #14202, #71091, #48198, #14936, #2398, #24919, #48935, #20465, #43019, #65547, #37475, #59995, #13459, #9405, #71464, #31935, #54472, #20840, #43394, #36007, #47461, #41921, #64446, #36377, #22303, #33028, #4962, #60356, #66281, #11228, #55208, #44497, #72554, #27864, #21942, #67391, #43756, #32667, #61463, #60724, #9765, #67030, #154, #55567, #27495, #26768, #16030, #16753, #16389, #44855, #38945, #38578, #10500, #15297, #32299, #49665, #50751, #65916, #50396, #21204, #10858, #4601, #10135, #55927, #27132, #39311, #61102, #50029, #15659, #22660, #38198, #54834, #5323, #33391, #72921, #37836, #61823, #72193, #33751, #5686, #56296, #28221, #4241, #49300, #21572, #71834, #44126, #66653, #34835, #7484, #68109, #46288, #41118, #57361, #63629, #40386, #34470, #11591, #1594, #51831, #1235, #35198, #51474, #17825, #28937, #1962, #52193, #68463, #45577, #17116, #23740, #18185, #56647, #13018, #18553, #62195, #7126, #56998, #62905, #35556, #23383, #6768, #57721, #68829, #58076, #29301, #30013, #12299, #6405, #34108, #24105, #40755, #63270, #29656, #876, #12662, #45932, #45210, #46653, #69193, #17475, #39675, #52556, #67744, #6042, #28576, #51113, #510, #23021, #40035, #62549, #11945, #2675, #59171, #37014, #19274, #59538, #30387, #14847, #18912, #8215, #8579, #41828, #25939, #41472, #63992, #59910, #8948, #69907, #25191, #31482, #65089, #24469, #70634, #37386, #54024, #42201, #47735, #54385, #30744, #70274, #19645, #64725, #31108, #3419, #14110, #36649, #13373, #24829, #42930, #13749, #3040, #53647, #48479, #25571, #71003, #2314, #64359, #20009, #36291, #35915, #48111, #31849, #42562, #14480, #58440, #20379, #65454, #9316, #47017, #69552, #7851, #52916, #47377, #58805, #53276, #61733, #3780, #38859, #32213, #21847, #43670, #71747, #66936, #21117, #5230, #72099, #27046, #54747, #33662, #4149, #71373, #16305, #44410, #61374, #26305, #10771, #49213, #4871, #16663, #49577, #44036, #55842, #11134, #66193, #48842, #49938, #20748, #66558, #39221, #26681, #43305, #72462, #33304, #27771, #50311, #60634, #72833, #21484, #22216, #65826, #15571, #15938, #44770, #38113, #38487, #61011, #10046, #55479, #10409, #15208, #32941, #27407, #32580, #67305, #37748, #60266, #9680, #55118, #4517, #28485, #69106, #17390, #51383, #34378, #28136, #39582, #40299, #45485, #12213, #46201, #68017, #6315, #22927, #56558, #57272, #62460, #68742, #35110, #57634, #5599, #23657, #785, #22574, #23294, #17023, #24015, #5953, #56206, #63181, #18100, #34742, #51022, #39947, #50664, #68, #41031, #40661, #17740, #45122, #7040, #62106, #12576, #11858, #56910, #29570, #52106, #12933, #67657, #11499, #28844, #34021, #46564, #18468, #1511, #62821, #63547, #418, #6683, #29211, #45843, #68379, #51747, #1148, #53189, #31022, #69822, #42845, #25105, #19928, #25855, #47649, #2231, #48027, #52829, #20290, #53556, #2953, #70181, #25481, #42482, #42115, #29928, #70553, #1875, #13290, #19559, #52468, #24744, #64639, #65005, #19188, #14025, #36200, #14393, #47288, #30657, #41741, #8489, #36930, #59451, #36565, #24381, #8858, #46929, #35827, #59085, #69467, #64269, #31394, #53934, #13658, #3329, #58718, #48392, #8130, #2586, #70920, #65366, #35468, #57990, #7400, #18825, #41388, #63900, #58350, #7761, #30297, #22128, #26586, #38024, #27317, #60182, #26957, #9954, #9591, #66470, #21391, #9227, #55025, #43947, #71655, #15847, #38393, #55389, #60547, #60917, #31764, #32123, #27679, #49126, #32490, #66102, #59822, #71281, #72015, #4060, #10320, #4783, #21028, #4428, #54657, #15122, #32852, #43581, #49849, #66846, #16216, #37299, #72375, #49484, #54301, #21755, #48757, #55750, #37659, #14755, #44316, #38769, #61288, #15481, #10681, #3693, #26218, #72742, #33211, #5144, #20658, #50217, #43217, #44683, #65737, #56474, #18020, #68655, #23931, #67214, #22486, #5866, #16575, #35025, #6955, #1064, #51297, #57553, #39127, #28757, #45760, #29486, #17303, #52023, #11774, #34290, #62738, #28398, #1425, #56822, #51662, #61642, #6229, #33932, #6599, #11415, #11044, #12130, #34657, #698, #62013, #40576, #33570 ) ),
 .UNSPECIFIED., .F., .F., .F. ) 
 B_SPLINE_SURFACE_WITH_KNOTS ( ( 2, 2 ),
 ( 3, 2, 2, 2, 2, 2, 2, 2, 2, 2, 2, 2, 2, 2, 2, 2, 2, 2, 2, 2, 2, 2, 2, 2, 2, 2, 2, 2, 2, 2, 2, 2, 2, 2, 2, 2, 2, 2, 2, 2, 2, 2, 2, 2, 2, 2, 2, 2, 2, 2, 2, 2, 2, 2, 2, 2, 2, 2, 2, 2, 2, 2, 2, 2, 2, 2, 2, 2, 2, 2, 2, 2, 2, 2, 2, 2, 2, 2, 2, 2, 2, 2, 2, 2, 2, 2, 2, 2, 2, 2, 2, 2, 2, 2, 2, 2, 2, 2, 2, 2, 2, 2, 2, 2, 2, 2, 2, 2, 2, 2, 2, 2, 2, 2, 2, 2, 2, 2, 2, 2, 2, 2, 2, 2, 2, 2, 2, 2, 2, 2, 2, 2, 2, 2, 2, 2, 2, 2, 2, 2, 2, 2, 2, 2, 2, 2, 2, 2, 2, 2, 2, 2, 2, 2, 2, 2, 2, 2, 2, 2, 2, 2, 2, 2, 2, 2, 2, 2, 2, 2, 2, 2, 2, 2, 2, 2, 2, 2, 2, 2, 2, 2, 2, 2, 2, 2, 2, 2, 2, 2, 2, 2, 2, 2, 2, 2, 2, 2, 2, 2, 2, 2, 2, 2, 2, 2, 2, 2, 2, 2, 2, 2, 2, 2, 2, 2, 2, 2, 2, 2, 2, 2, 2, 2, 2, 2, 2, 2, 2, 2, 2, 2, 2, 2, 2, 2, 2, 2, 2, 2, 2, 2, 2, 2, 2, 2, 2, 2, 2, 2, 2, 2, 2, 2, 2, 2, 2, 2, 2, 2, 2, 2, 2, 2, 2, 2, 2, 2, 2, 2, 2, 2, 2, 2, 2, 2, 2, 2, 2, 2, 2, 2, 2, 2, 2, 2, 2, 2, 2, 2, 2, 2, 2, 2, 2, 2, 2, 2, 2, 2, 2, 2, 2, 2, 2, 2, 2, 2, 2, 2, 2, 2, 2, 2, 2, 2, 2, 2, 2, 2, 2, 2, 2, 2, 2, 2, 2, 2, 2, 2, 2, 2, 2, 2, 2, 2, 2, 2, 2, 2, 2, 2, 2, 2, 2, 2, 2, 2, 2, 2, 2, 2, 2, 2, 2, 2, 2, 2, 2, 2, 3 ),
 ( 0.000000000000000000, 1.000000000000000000 ),
 ( 0.000000000000000000, 0.002777777777777777884, 0.005555555555555555768, 0.008333333333333333218, 0.01111111111111111154, 0.01388888888888888812, 0.01666666666666666644, 0.01944444444444444475, 0.02222222222222222307, 0.02500000000000000139, 0.02777777777777777624, 0.03055555555555555455, 0.03333333333333333287, 0.03611111111111110772, 0.03888888888888888951, 0.04166666666666666435, 0.04444444444444444614, 0.04722222222222222099, 0.05000000000000000278, 0.05277777777777777762, 0.05555555555555555247, 0.05833333333333333426, 0.06111111111111110911, 0.06388888888888888395, 0.06666666666666666574, 0.06944444444444444753, 0.07222222222222221544, 0.07499999999999999722, 0.07777777777777777901, 0.08055555555555556080, 0.08333333333333332871, 0.08611111111111111049, 0.08888888888888889228, 0.09166666666666666019, 0.09444444444444444198, 0.09722222222222222376, 0.1000000000000000056, 0.1027777777777777735, 0.1055555555555555552, 0.1083333333333333370, 0.1111111111111111049, 0.1138888888888888867, 0.1166666666666666685, 0.1194444444444444503, 0.1222222222222222182, 0.1250000000000000000, 0.1277777777777777679, 0.1305555555555555636, 0.1333333333333333315, 0.1361111111111110994, 0.1388888888888888951, 0.1416666666666666630, 0.1444444444444444309, 0.1472222222222222265, 0.1499999999999999944, 0.1527777777777777901, 0.1555555555555555580, 0.1583333333333333259, 0.1611111111111111216, 0.1638888888888888895, 0.1666666666666666574, 0.1694444444444444531, 0.1722222222222222210, 0.1749999999999999889, 0.1777777777777777846, 0.1805555555555555525, 0.1833333333333333204, 0.1861111111111111160, 0.1888888888888888840, 0.1916666666666666796, 0.1944444444444444475, 0.1972222222222222154, 0.2000000000000000111, 0.2027777777777777790, 0.2055555555555555469, 0.2083333333333333426, 0.2111111111111111105, 0.2138888888888888784, 0.2166666666666666741, 0.2194444444444444420, 0.2222222222222222099, 0.2250000000000000056, 0.2277777777777777735, 0.2305555555555555691, 0.2333333333333333370, 0.2361111111111111049, 0.2388888888888889006, 0.2416666666666666685, 0.2444444444444444364, 0.2472222222222222321, 0.2500000000000000000, 0.2527777777777777679, 0.2555555555555555358, 0.2583333333333333592, 0.2611111111111111271, 0.2638888888888888951, 0.2666666666666666630, 0.2694444444444444309, 0.2722222222222221988, 0.2750000000000000222, 0.2777777777777777901, 0.2805555555555555580, 0.2833333333333333259, 0.2861111111111110938, 0.2888888888888888618, 0.2916666666666666852, 0.2944444444444444531, 0.2972222222222222210, 0.2999999999999999889, 0.3027777777777777568, 0.3055555555555555802, 0.3083333333333333481, 0.3111111111111111160, 0.3138888888888888840, 0.3166666666666666519, 0.3194444444444444198, 0.3222222222222222432, 0.3250000000000000111, 0.3277777777777777790, 0.3305555555555555469, 0.3333333333333333148, 0.3361111111111111382, 0.3388888888888889062, 0.3416666666666666741, 0.3444444444444444420, 0.3472222222222222099, 0.3499999999999999778, 0.3527777777777778012, 0.3555555555555555691, 0.3583333333333333370, 0.3611111111111111049, 0.3638888888888888729, 0.3666666666666666408, 0.3694444444444444642, 0.3722222222222222321, 0.3750000000000000000, 0.3777777777777777679, 0.3805555555555555358, 0.3833333333333333592, 0.3861111111111111271, 0.3888888888888888951, 0.3916666666666666630, 0.3944444444444444309, 0.3972222222222221988, 0.4000000000000000222, 0.4027777777777777901, 0.4055555555555555580, 0.4083333333333333259, 0.4111111111111110938, 0.4138888888888888618, 0.4166666666666666852, 0.4194444444444444531, 0.4222222222222222210, 0.4249999999999999889, 0.4277777777777777568, 0.4305555555555555802, 0.4333333333333333481, 0.4361111111111111160, 0.4388888888888888840, 0.4416666666666666519, 0.4444444444444444198, 0.4472222222222222432, 0.4500000000000000111, 0.4527777777777777790, 0.4555555555555555469, 0.4583333333333333148, 0.4611111111111111382, 0.4638888888888889062, 0.4666666666666666741, 0.4694444444444444420, 0.4722222222222222099, 0.4749999999999999778, 0.4777777777777778012, 0.4805555555555555691, 0.4833333333333333370, 0.4861111111111111049, 0.4888888888888888729, 0.4916666666666666408, 0.4944444444444444642, 0.4972222222222222321, 0.5000000000000000000, 0.5027777777777777679, 0.5055555555555555358, 0.5083333333333333037, 0.5111111111111110716, 0.5138888888888888395, 0.5166666666666667185, 0.5194444444444444864, 0.5222222222222222543, 0.5250000000000000222, 0.5277777777777777901, 0.5305555555555555580, 0.5333333333333333259, 0.5361111111111110938, 0.5388888888888888618, 0.5416666666666666297, 0.5444444444444443976, 0.5472222222222222765, 0.5500000000000000444, 0.5527777777777778123, 0.5555555555555555802, 0.5583333333333333481, 0.5611111111111111160, 0.5638888888888888840, 0.5666666666666666519, 0.5694444444444444198, 0.5722222222222221877, 0.5749999999999999556, 0.5777777777777777235, 0.5805555555555556024, 0.5833333333333333703, 0.5861111111111111382, 0.5888888888888889062, 0.5916666666666666741, 0.5944444444444444420, 0.5972222222222222099, 0.5999999999999999778, 0.6027777777777777457, 0.6055555555555555136, 0.6083333333333332815, 0.6111111111111111605, 0.6138888888888889284, 0.6166666666666666963, 0.6194444444444444642, 0.6222222222222222321, 0.6250000000000000000, 0.6277777777777777679, 0.6305555555555555358, 0.6333333333333333037, 0.6361111111111110716, 0.6388888888888888395, 0.6416666666666667185, 0.6444444444444444864, 0.6472222222222222543, 0.6500000000000000222, 0.6527777777777777901, 0.6555555555555555580, 0.6583333333333333259, 0.6611111111111110938, 0.6638888888888888618, 0.6666666666666666297, 0.6694444444444443976, 0.6722222222222222765, 0.6750000000000000444, 0.6777777777777778123, 0.6805555555555555802, 0.6833333333333333481, 0.6861111111111111160, 0.6888888888888888840, 0.6916666666666666519, 0.6944444444444444198, 0.6972222222222221877, 0.6999999999999999556, 0.7027777777777777235, 0.7055555555555556024, 0.7083333333333333703, 0.7111111111111111382, 0.7138888888888889062, 0.7166666666666666741, 0.7194444444444444420, 0.7222222222222222099, 0.7249999999999999778, 0.7277777777777777457, 0.7305555555555555136, 0.7333333333333332815, 0.7361111111111111605, 0.7388888888888889284, 0.7416666666666666963, 0.7444444444444444642, 0.7472222222222222321, 0.7500000000000000000, 0.7527777777777777679, 0.7555555555555555358, 0.7583333333333333037, 0.7611111111111110716, 0.7638888888888888395, 0.7666666666666667185, 0.7694444444444444864, 0.7722222222222222543, 0.7750000000000000222, 0.7777777777777777901, 0.7805555555555555580, 0.7833333333333333259, 0.7861111111111110938, 0.7888888888888888618, 0.7916666666666666297, 0.7944444444444443976, 0.7972222222222222765, 0.8000000000000000444, 0.8027777777777778123, 0.8055555555555555802, 0.8083333333333333481, 0.8111111111111111160, 0.8138888888888888840, 0.8166666666666666519, 0.8194444444444444198, 0.8222222222222221877, 0.8249999999999999556, 0.8277777777777777235, 0.8305555555555556024, 0.8333333333333333703, 0.8361111111111111382, 0.8388888888888889062, 0.8416666666666666741, 0.8444444444444444420, 0.8472222222222222099, 0.8499999999999999778, 0.8527777777777777457, 0.8555555555555555136, 0.8583333333333332815, 0.8611111111111111605, 0.8638888888888889284, 0.8666666666666666963, 0.8694444444444444642, 0.8722222222222222321, 0.8750000000000000000, 0.8777777777777777679, 0.8805555555555555358, 0.8833333333333333037, 0.8861111111111110716, 0.8888888888888888395, 0.8916666666666667185, 0.8944444444444444864, 0.8972222222222222543, 0.9000000000000000222, 0.9027777777777777901, 0.9055555555555555580, 0.9083333333333333259, 0.9111111111111110938, 0.9138888888888888618, 0.9166666666666666297, 0.9194444444444443976, 0.9222222222222222765, 0.9250000000000000444, 0.9277777777777778123, 0.9305555555555555802, 0.9333333333333333481, 0.9361111111111111160, 0.9388888888888888840, 0.9416666666666666519, 0.9444444444444444198, 0.9472222222222221877, 0.9499999999999999556, 0.9527777777777777235, 0.9555555555555556024, 0.9583333333333333703, 0.9611111111111111382, 0.9638888888888889062, 0.9666666666666666741, 0.9694444444444444420, 0.9722222222222222099, 0.9749999999999999778, 0.9777777777777777457, 0.9805555555555555136, 0.9833333333333332815, 0.9861111111111111605, 0.9888888888888889284, 0.9916666666666666963, 0.9944444444444444642, 0.9972222222222222321, 1.000000000000000000 ),
 .UNSPECIFIED. ) 
 GEOMETRIC_REPRESENTATION_ITEM ( )  RATIONAL_B_SPLINE_SURFACE ( (
 ( 1.000000000000000000, 0.8660254037844387076, 1.000000000000000000, 0.8660254037844387076, 1.000000000000000000, 0.8660254037844387076, 1.000000000000000000, 0.8660254037844387076, 1.000000000000000000, 0.8660254037844387076, 1.000000000000000000, 0.8660254037844387076, 1.000000000000000000, 0.8660254037844387076, 1.000000000000000000, 0.8660254037844387076, 1.000000000000000000, 0.8660254037844387076, 1.000000000000000000, 0.8660254037844387076, 1.000000000000000000, 0.8660254037844387076, 1.000000000000000000, 0.8660254037844387076, 1.000000000000000000, 0.8660254037844387076, 1.000000000000000000, 0.8660254037844387076, 1.000000000000000000, 0.8660254037844387076, 1.000000000000000000, 0.8660254037844387076, 1.000000000000000000, 0.8660254037844387076, 1.000000000000000000, 0.8660254037844387076, 1.000000000000000000, 0.8660254037844387076, 1.000000000000000000, 0.8660254037844387076, 1.000000000000000000, 0.8660254037844387076, 1.000000000000000000, 0.8660254037844387076, 1.000000000000000000, 0.8660254037844387076, 1.000000000000000000, 0.8660254037844387076, 1.000000000000000000, 0.8660254037844387076, 1.000000000000000000, 0.8660254037844387076, 1.000000000000000000, 0.8660254037844387076, 1.000000000000000000, 0.8660254037844387076, 1.000000000000000000, 0.8660254037844387076, 1.000000000000000000, 0.8660254037844387076, 1.000000000000000000, 0.8660254037844387076, 1.000000000000000000, 0.8660254037844387076, 1.000000000000000000, 0.8660254037844387076, 1.000000000000000000, 0.8660254037844387076, 1.000000000000000000, 0.8660254037844387076, 1.000000000000000000, 0.8660254037844387076, 1.000000000000000000, 0.8660254037844387076, 1.000000000000000000, 0.8660254037844387076, 1.000000000000000000, 0.8660254037844387076, 1.000000000000000000, 0.8660254037844387076, 1.000000000000000000, 0.8660254037844387076, 1.000000000000000000, 0.8660254037844387076, 1.000000000000000000, 0.8660254037844387076, 1.000000000000000000, 0.8660254037844387076, 1.000000000000000000, 0.8660254037844387076, 1.000000000000000000, 0.8660254037844387076, 1.000000000000000000, 0.8660254037844387076, 1.000000000000000000, 0.8660254037844387076, 1.000000000000000000, 0.8660254037844387076, 1.000000000000000000, 0.8660254037844387076, 1.000000000000000000, 0.8660254037844387076, 1.000000000000000000, 0.8660254037844387076, 1.000000000000000000, 0.8660254037844387076, 1.000000000000000000, 0.8660254037844387076, 1.000000000000000000, 0.8660254037844387076, 1.000000000000000000, 0.8660254037844387076, 1.000000000000000000, 0.8660254037844387076, 1.000000000000000000, 0.8660254037844387076, 1.000000000000000000, 0.8660254037844387076, 1.000000000000000000, 0.8660254037844387076, 1.000000000000000000, 0.8660254037844387076, 1.000000000000000000, 0.8660254037844387076, 1.000000000000000000, 0.8660254037844387076, 1.000000000000000000, 0.8660254037844387076, 1.000000000000000000, 0.8660254037844387076, 1.000000000000000000, 0.8660254037844387076, 1.000000000000000000, 0.8660254037844387076, 1.000000000000000000, 0.8660254037844387076, 1.000000000000000000, 0.8660254037844387076, 1.000000000000000000, 0.8660254037844387076, 1.000000000000000000, 0.8660254037844387076, 1.000000000000000000, 0.8660254037844387076, 1.000000000000000000, 0.8660254037844387076, 1.000000000000000000, 0.8660254037844387076, 1.000000000000000000, 0.8660254037844387076, 1.000000000000000000, 0.8660254037844387076, 1.000000000000000000, 0.8660254037844387076, 1.000000000000000000, 0.8660254037844387076, 1.000000000000000000, 0.8660254037844387076, 1.000000000000000000, 0.8660254037844387076, 1.000000000000000000, 0.8660254037844387076, 1.000000000000000000, 0.8660254037844387076, 1.000000000000000000, 0.8660254037844387076, 1.000000000000000000, 0.8660254037844387076, 1.000000000000000000, 0.8660254037844387076, 1.000000000000000000, 0.8660254037844387076, 1.000000000000000000, 0.8660254037844387076, 1.000000000000000000, 0.8660254037844387076, 1.000000000000000000, 0.8660254037844387076, 1.000000000000000000, 0.8660254037844387076, 1.000000000000000000, 0.8660254037844387076, 1.000000000000000000, 0.8660254037844387076, 1.000000000000000000, 0.8660254037844387076, 1.000000000000000000, 0.8660254037844387076, 1.000000000000000000, 0.8660254037844387076, 1.000000000000000000, 0.8660254037844387076, 1.000000000000000000, 0.8660254037844387076, 1.000000000000000000, 0.8660254037844387076, 1.000000000000000000, 0.8660254037844387076, 1.000000000000000000, 0.8660254037844387076, 1.000000000000000000, 0.8660254037844387076, 1.000000000000000000, 0.8660254037844387076, 1.000000000000000000, 0.8660254037844387076, 1.000000000000000000, 0.8660254037844387076, 1.000000000000000000, 0.8660254037844387076, 1.000000000000000000, 0.8660254037844387076, 1.000000000000000000, 0.8660254037844387076, 1.000000000000000000, 0.8660254037844387076, 1.000000000000000000, 0.8660254037844387076, 1.000000000000000000, 0.8660254037844387076, 1.000000000000000000, 0.8660254037844387076, 1.000000000000000000, 0.8660254037844387076, 1.000000000000000000, 0.8660254037844387076, 1.000000000000000000, 0.8660254037844387076, 1.000000000000000000, 0.8660254037844387076, 1.000000000000000000, 0.8660254037844387076, 1.000000000000000000, 0.8660254037844387076, 1.000000000000000000, 0.8660254037844387076, 1.000000000000000000, 0.8660254037844387076, 1.000000000000000000, 0.8660254037844387076, 1.000000000000000000, 0.8660254037844387076, 1.000000000000000000, 0.8660254037844387076, 1.000000000000000000, 0.8660254037844387076, 1.000000000000000000, 0.8660254037844387076, 1.000000000000000000, 0.8660254037844387076, 1.000000000000000000, 0.8660254037844387076, 1.000000000000000000, 0.8660254037844387076, 1.000000000000000000, 0.8660254037844387076, 1.000000000000000000, 0.8660254037844387076, 1.000000000000000000, 0.8660254037844387076, 1.000000000000000000, 0.8660254037844387076, 1.000000000000000000, 0.8660254037844387076, 1.000000000000000000, 0.8660254037844387076, 1.000000000000000000, 0.8660254037844387076, 1.000000000000000000, 0.8660254037844387076, 1.000000000000000000, 0.8660254037844387076, 1.000000000000000000, 0.8660254037844387076, 1.000000000000000000, 0.8660254037844387076, 1.000000000000000000, 0.8660254037844387076, 1.000000000000000000, 0.8660254037844387076, 1.000000000000000000, 0.8660254037844387076, 1.000000000000000000, 0.8660254037844387076, 1.000000000000000000, 0.8660254037844387076, 1.000000000000000000, 0.8660254037844387076, 1.000000000000000000, 0.8660254037844387076, 1.000000000000000000, 0.8660254037844387076, 1.000000000000000000, 0.8660254037844387076, 1.000000000000000000, 0.8660254037844387076, 1.000000000000000000, 0.8660254037844387076, 1.000000000000000000, 0.8660254037844387076, 1.000000000000000000, 0.8660254037844387076, 1.000000000000000000, 0.8660254037844387076, 1.000000000000000000, 0.8660254037844387076, 1.000000000000000000, 0.8660254037844387076, 1.000000000000000000, 0.8660254037844387076, 1.000000000000000000, 0.8660254037844387076, 1.000000000000000000, 0.8660254037844387076, 1.000000000000000000, 0.8660254037844387076, 1.000000000000000000, 0.8660254037844387076, 1.000000000000000000, 0.8660254037844387076, 1.000000000000000000, 0.8660254037844387076, 1.000000000000000000, 0.8660254037844387076, 1.000000000000000000, 0.8660254037844387076, 1.000000000000000000, 0.8660254037844387076, 1.000000000000000000, 0.8660254037844387076, 1.000000000000000000, 0.8660254037844387076, 1.000000000000000000, 0.8660254037844387076, 1.000000000000000000, 0.8660254037844387076, 1.000000000000000000, 0.8660254037844387076, 1.000000000000000000, 0.8660254037844387076, 1.000000000000000000, 0.8660254037844387076, 1.000000000000000000, 0.8660254037844387076, 1.000000000000000000, 0.8660254037844387076, 1.000000000000000000, 0.8660254037844387076, 1.000000000000000000, 0.8660254037844387076, 1.000000000000000000, 0.8660254037844387076, 1.000000000000000000, 0.8660254037844387076, 1.000000000000000000, 0.8660254037844387076, 1.000000000000000000, 0.8660254037844387076, 1.000000000000000000, 0.8660254037844387076, 1.000000000000000000, 0.8660254037844387076, 1.000000000000000000, 0.8660254037844387076, 1.000000000000000000, 0.8660254037844387076, 1.000000000000000000, 0.8660254037844387076, 1.000000000000000000, 0.8660254037844387076, 1.000000000000000000, 0.8660254037844387076, 1.000000000000000000, 0.8660254037844387076, 1.000000000000000000, 0.8660254037844387076, 1.000000000000000000, 0.8660254037844387076, 1.000000000000000000, 0.8660254037844387076, 1.000000000000000000, 0.8660254037844387076, 1.000000000000000000, 0.8660254037844387076, 1.000000000000000000, 0.8660254037844387076, 1.000000000000000000, 0.8660254037844387076, 1.000000000000000000, 0.8660254037844387076, 1.000000000000000000, 0.8660254037844387076, 1.000000000000000000, 0.8660254037844387076, 1.000000000000000000, 0.8660254037844387076, 1.000000000000000000, 0.8660254037844387076, 1.000000000000000000, 0.8660254037844387076, 1.000000000000000000, 0.8660254037844387076, 1.000000000000000000, 0.8660254037844387076, 1.000000000000000000, 0.8660254037844387076, 1.000000000000000000, 0.8660254037844387076, 1.000000000000000000, 0.8660254037844387076, 1.000000000000000000, 0.8660254037844387076, 1.000000000000000000, 0.8660254037844387076, 1.000000000000000000, 0.8660254037844387076, 1.000000000000000000, 0.8660254037844387076, 1.000000000000000000, 0.8660254037844387076, 1.000000000000000000, 0.8660254037844387076, 1.000000000000000000, 0.8660254037844387076, 1.000000000000000000, 0.8660254037844387076, 1.000000000000000000, 0.8660254037844387076, 1.000000000000000000, 0.8660254037844387076, 1.000000000000000000, 0.8660254037844387076, 1.000000000000000000, 0.8660254037844387076, 1.000000000000000000, 0.8660254037844387076, 1.000000000000000000, 0.8660254037844387076, 1.000000000000000000, 0.8660254037844387076, 1.000000000000000000, 0.8660254037844387076, 1.000000000000000000, 0.8660254037844387076, 1.000000000000000000, 0.8660254037844387076, 1.000000000000000000, 0.8660254037844387076, 1.000000000000000000, 0.8660254037844387076, 1.000000000000000000, 0.8660254037844387076, 1.000000000000000000, 0.8660254037844387076, 1.000000000000000000, 0.8660254037844387076, 1.000000000000000000, 0.8660254037844387076, 1.000000000000000000, 0.8660254037844387076, 1.000000000000000000, 0.8660254037844387076, 1.000000000000000000, 0.8660254037844387076, 1.000000000000000000, 0.8660254037844387076, 1.000000000000000000, 0.8660254037844387076, 1.000000000000000000, 0.8660254037844387076, 1.000000000000000000, 0.8660254037844387076, 1.000000000000000000, 0.8660254037844387076, 1.000000000000000000, 0.8660254037844387076, 1.000000000000000000, 0.8660254037844387076, 1.000000000000000000, 0.8660254037844387076, 1.000000000000000000, 0.8660254037844387076, 1.000000000000000000, 0.8660254037844387076, 1.000000000000000000, 0.8660254037844387076, 1.000000000000000000, 0.8660254037844387076, 1.000000000000000000, 0.8660254037844387076, 1.000000000000000000, 0.8660254037844387076, 1.000000000000000000, 0.8660254037844387076, 1.000000000000000000, 0.8660254037844387076, 1.000000000000000000, 0.8660254037844387076, 1.000000000000000000, 0.8660254037844387076, 1.000000000000000000, 0.8660254037844387076, 1.000000000000000000, 0.8660254037844387076, 1.000000000000000000, 0.8660254037844387076, 1.000000000000000000, 0.8660254037844387076, 1.000000000000000000, 0.8660254037844387076, 1.000000000000000000, 0.8660254037844387076, 1.000000000000000000, 0.8660254037844387076, 1.000000000000000000, 0.8660254037844387076, 1.000000000000000000, 0.8660254037844387076, 1.000000000000000000, 0.8660254037844387076, 1.000000000000000000, 0.8660254037844387076, 1.000000000000000000, 0.8660254037844387076, 1.000000000000000000, 0.8660254037844387076, 1.000000000000000000, 0.8660254037844387076, 1.000000000000000000, 0.8660254037844387076, 1.000000000000000000, 0.8660254037844387076, 1.000000000000000000, 0.8660254037844387076, 1.000000000000000000, 0.8660254037844387076, 1.000000000000000000, 0.8660254037844387076, 1.000000000000000000, 0.8660254037844387076, 1.000000000000000000, 0.8660254037844387076, 1.000000000000000000, 0.8660254037844387076, 1.000000000000000000, 0.8660254037844387076, 1.000000000000000000, 0.8660254037844387076, 1.000000000000000000, 0.8660254037844387076, 1.000000000000000000, 0.8660254037844387076, 1.000000000000000000, 0.8660254037844387076, 1.000000000000000000, 0.8660254037844387076, 1.000000000000000000, 0.8660254037844387076, 1.000000000000000000, 0.8660254037844387076, 1.000000000000000000, 0.8660254037844387076, 1.000000000000000000, 0.8660254037844387076, 1.000000000000000000, 0.8660254037844387076, 1.000000000000000000, 0.8660254037844387076, 1.000000000000000000, 0.8660254037844387076, 1.000000000000000000, 0.8660254037844387076, 1.000000000000000000, 0.8660254037844387076, 1.000000000000000000, 0.8660254037844387076, 1.000000000000000000, 0.8660254037844387076, 1.000000000000000000, 0.8660254037844387076, 1.000000000000000000, 0.8660254037844387076, 1.000000000000000000, 0.8660254037844387076, 1.000000000000000000, 0.8660254037844387076, 1.000000000000000000, 0.8660254037844387076, 1.000000000000000000, 0.8660254037844387076, 1.000000000000000000, 0.8660254037844387076, 1.000000000000000000, 0.8660254037844387076, 1.000000000000000000, 0.8660254037844387076, 1.000000000000000000, 0.8660254037844387076, 1.000000000000000000, 0.8660254037844387076, 1.000000000000000000, 0.8660254037844387076, 1.000000000000000000, 0.8660254037844387076, 1.000000000000000000, 0.8660254037844387076, 1.000000000000000000, 0.8660254037844387076, 1.000000000000000000, 0.8660254037844387076, 1.000000000000000000, 0.8660254037844387076, 1.000000000000000000, 0.8660254037844387076, 1.000000000000000000, 0.8660254037844387076, 1.000000000000000000, 0.8660254037844387076, 1.000000000000000000, 0.8660254037844387076, 1.000000000000000000, 0.8660254037844387076, 1.000000000000000000, 0.8660254037844387076, 1.000000000000000000, 0.8660254037844387076, 1.000000000000000000, 0.8660254037844387076, 1.000000000000000000, 0.8660254037844387076, 1.000000000000000000, 0.8660254037844387076, 1.000000000000000000, 0.8660254037844387076, 1.000000000000000000, 0.8660254037844387076, 1.000000000000000000, 0.8660254037844387076, 1.000000000000000000, 0.8660254037844387076, 1.000000000000000000, 0.8660254037844387076, 1.000000000000000000, 0.8660254037844387076, 1.000000000000000000, 0.8660254037844387076, 1.000000000000000000, 0.8660254037844387076, 1.000000000000000000, 0.8660254037844387076, 1.000000000000000000, 0.8660254037844387076, 1.000000000000000000, 0.8660254037844387076, 1.000000000000000000, 0.8660254037844387076, 1.000000000000000000, 0.8660254037844387076, 1.000000000000000000, 0.8660254037844387076, 1.000000000000000000, 0.8660254037844387076, 1.000000000000000000, 0.8660254037844387076, 1.000000000000000000, 0.8660254037844387076, 1.000000000000000000, 0.8660254037844387076, 1.000000000000000000, 0.8660254037844387076, 1.000000000000000000, 0.8660254037844387076, 1.000000000000000000, 0.8660254037844387076, 1.000000000000000000, 0.8660254037844387076, 1.000000000000000000, 0.8660254037844387076, 1.000000000000000000, 0.8660254037844387076, 1.000000000000000000, 0.8660254037844387076, 1.000000000000000000, 0.8660254037844387076, 1.000000000000000000, 0.8660254037844387076, 1.000000000000000000, 0.8660254037844387076, 1.000000000000000000, 0.8660254037844387076, 1.000000000000000000, 0.8660254037844387076, 1.000000000000000000, 0.8660254037844387076, 1.000000000000000000, 0.8660254037844387076, 1.000000000000000000, 0.8660254037844387076, 1.000000000000000000, 0.8660254037844387076, 1.000000000000000000, 0.8660254037844387076, 1.000000000000000000, 0.8660254037844387076, 1.000000000000000000, 0.8660254037844387076, 1.000000000000000000, 0.8660254037844387076, 1.000000000000000000, 0.8660254037844387076, 1.000000000000000000, 0.8660254037844387076, 1.000000000000000000, 0.8660254037844387076, 1.000000000000000000, 0.8660254037844387076, 1.000000000000000000, 0.8660254037844387076, 1.000000000000000000, 0.8660254037844387076, 1.000000000000000000),
 ( 1.000000000000000000, 0.8660254037844387076, 1.000000000000000000, 0.8660254037844387076, 1.000000000000000000, 0.8660254037844387076, 1.000000000000000000, 0.8660254037844387076, 1.000000000000000000, 0.8660254037844387076, 1.000000000000000000, 0.8660254037844387076, 1.000000000000000000, 0.8660254037844387076, 1.000000000000000000, 0.8660254037844387076, 1.000000000000000000, 0.8660254037844387076, 1.000000000000000000, 0.8660254037844387076, 1.000000000000000000, 0.8660254037844387076, 1.000000000000000000, 0.8660254037844387076, 1.000000000000000000, 0.8660254037844387076, 1.000000000000000000, 0.8660254037844387076, 1.000000000000000000, 0.8660254037844387076, 1.000000000000000000, 0.8660254037844387076, 1.000000000000000000, 0.8660254037844387076, 1.000000000000000000, 0.8660254037844387076, 1.000000000000000000, 0.8660254037844387076, 1.000000000000000000, 0.8660254037844387076, 1.000000000000000000, 0.8660254037844387076, 1.000000000000000000, 0.8660254037844387076, 1.000000000000000000, 0.8660254037844387076, 1.000000000000000000, 0.8660254037844387076, 1.000000000000000000, 0.8660254037844387076, 1.000000000000000000, 0.8660254037844387076, 1.000000000000000000, 0.8660254037844387076, 1.000000000000000000, 0.8660254037844387076, 1.000000000000000000, 0.8660254037844387076, 1.000000000000000000, 0.8660254037844387076, 1.000000000000000000, 0.8660254037844387076, 1.000000000000000000, 0.8660254037844387076, 1.000000000000000000, 0.8660254037844387076, 1.000000000000000000, 0.8660254037844387076, 1.000000000000000000, 0.8660254037844387076, 1.000000000000000000, 0.8660254037844387076, 1.000000000000000000, 0.8660254037844387076, 1.000000000000000000, 0.8660254037844387076, 1.000000000000000000, 0.8660254037844387076, 1.000000000000000000, 0.8660254037844387076, 1.000000000000000000, 0.8660254037844387076, 1.000000000000000000, 0.8660254037844387076, 1.000000000000000000, 0.8660254037844387076, 1.000000000000000000, 0.8660254037844387076, 1.000000000000000000, 0.8660254037844387076, 1.000000000000000000, 0.8660254037844387076, 1.000000000000000000, 0.8660254037844387076, 1.000000000000000000, 0.8660254037844387076, 1.000000000000000000, 0.8660254037844387076, 1.000000000000000000, 0.8660254037844387076, 1.000000000000000000, 0.8660254037844387076, 1.000000000000000000, 0.8660254037844387076, 1.000000000000000000, 0.8660254037844387076, 1.000000000000000000, 0.8660254037844387076, 1.000000000000000000, 0.8660254037844387076, 1.000000000000000000, 0.8660254037844387076, 1.000000000000000000, 0.8660254037844387076, 1.000000000000000000, 0.8660254037844387076, 1.000000000000000000, 0.8660254037844387076, 1.000000000000000000, 0.8660254037844387076, 1.000000000000000000, 0.8660254037844387076, 1.000000000000000000, 0.8660254037844387076, 1.000000000000000000, 0.8660254037844387076, 1.000000000000000000, 0.8660254037844387076, 1.000000000000000000, 0.8660254037844387076, 1.000000000000000000, 0.8660254037844387076, 1.000000000000000000, 0.8660254037844387076, 1.000000000000000000, 0.8660254037844387076, 1.000000000000000000, 0.8660254037844387076, 1.000000000000000000, 0.8660254037844387076, 1.000000000000000000, 0.8660254037844387076, 1.000000000000000000, 0.8660254037844387076, 1.000000000000000000, 0.8660254037844387076, 1.000000000000000000, 0.8660254037844387076, 1.000000000000000000, 0.8660254037844387076, 1.000000000000000000, 0.8660254037844387076, 1.000000000000000000, 0.8660254037844387076, 1.000000000000000000, 0.8660254037844387076, 1.000000000000000000, 0.8660254037844387076, 1.000000000000000000, 0.8660254037844387076, 1.000000000000000000, 0.8660254037844387076, 1.000000000000000000, 0.8660254037844387076, 1.000000000000000000, 0.8660254037844387076, 1.000000000000000000, 0.8660254037844387076, 1.000000000000000000, 0.8660254037844387076, 1.000000000000000000, 0.8660254037844387076, 1.000000000000000000, 0.8660254037844387076, 1.000000000000000000, 0.8660254037844387076, 1.000000000000000000, 0.8660254037844387076, 1.000000000000000000, 0.8660254037844387076, 1.000000000000000000, 0.8660254037844387076, 1.000000000000000000, 0.8660254037844387076, 1.000000000000000000, 0.8660254037844387076, 1.000000000000000000, 0.8660254037844387076, 1.000000000000000000, 0.8660254037844387076, 1.000000000000000000, 0.8660254037844387076, 1.000000000000000000, 0.8660254037844387076, 1.000000000000000000, 0.8660254037844387076, 1.000000000000000000, 0.8660254037844387076, 1.000000000000000000, 0.8660254037844387076, 1.000000000000000000, 0.8660254037844387076, 1.000000000000000000, 0.8660254037844387076, 1.000000000000000000, 0.8660254037844387076, 1.000000000000000000, 0.8660254037844387076, 1.000000000000000000, 0.8660254037844387076, 1.000000000000000000, 0.8660254037844387076, 1.000000000000000000, 0.8660254037844387076, 1.000000000000000000, 0.8660254037844387076, 1.000000000000000000, 0.8660254037844387076, 1.000000000000000000, 0.8660254037844387076, 1.000000000000000000, 0.8660254037844387076, 1.000000000000000000, 0.8660254037844387076, 1.000000000000000000, 0.8660254037844387076, 1.000000000000000000, 0.8660254037844387076, 1.000000000000000000, 0.8660254037844387076, 1.000000000000000000, 0.8660254037844387076, 1.000000000000000000, 0.8660254037844387076, 1.000000000000000000, 0.8660254037844387076, 1.000000000000000000, 0.8660254037844387076, 1.000000000000000000, 0.8660254037844387076, 1.000000000000000000, 0.8660254037844387076, 1.000000000000000000, 0.8660254037844387076, 1.000000000000000000, 0.8660254037844387076, 1.000000000000000000, 0.8660254037844387076, 1.000000000000000000, 0.8660254037844387076, 1.000000000000000000, 0.8660254037844387076, 1.000000000000000000, 0.8660254037844387076, 1.000000000000000000, 0.8660254037844387076, 1.000000000000000000, 0.8660254037844387076, 1.000000000000000000, 0.8660254037844387076, 1.000000000000000000, 0.8660254037844387076, 1.000000000000000000, 0.8660254037844387076, 1.000000000000000000, 0.8660254037844387076, 1.000000000000000000, 0.8660254037844387076, 1.000000000000000000, 0.8660254037844387076, 1.000000000000000000, 0.8660254037844387076, 1.000000000000000000, 0.8660254037844387076, 1.000000000000000000, 0.8660254037844387076, 1.000000000000000000, 0.8660254037844387076, 1.000000000000000000, 0.8660254037844387076, 1.000000000000000000, 0.8660254037844387076, 1.000000000000000000, 0.8660254037844387076, 1.000000000000000000, 0.8660254037844387076, 1.000000000000000000, 0.8660254037844387076, 1.000000000000000000, 0.8660254037844387076, 1.000000000000000000, 0.8660254037844387076, 1.000000000000000000, 0.8660254037844387076, 1.000000000000000000, 0.8660254037844387076, 1.000000000000000000, 0.8660254037844387076, 1.000000000000000000, 0.8660254037844387076, 1.000000000000000000, 0.8660254037844387076, 1.000000000000000000, 0.8660254037844387076, 1.000000000000000000, 0.8660254037844387076, 1.000000000000000000, 0.8660254037844387076, 1.000000000000000000, 0.8660254037844387076, 1.000000000000000000, 0.8660254037844387076, 1.000000000000000000, 0.8660254037844387076, 1.000000000000000000, 0.8660254037844387076, 1.000000000000000000, 0.8660254037844387076, 1.000000000000000000, 0.8660254037844387076, 1.000000000000000000, 0.8660254037844387076, 1.000000000000000000, 0.8660254037844387076, 1.000000000000000000, 0.8660254037844387076, 1.000000000000000000, 0.8660254037844387076, 1.000000000000000000, 0.8660254037844387076, 1.000000000000000000, 0.8660254037844387076, 1.000000000000000000, 0.8660254037844387076, 1.000000000000000000, 0.8660254037844387076, 1.000000000000000000, 0.8660254037844387076, 1.000000000000000000, 0.8660254037844387076, 1.000000000000000000, 0.8660254037844387076, 1.000000000000000000, 0.8660254037844387076, 1.000000000000000000, 0.8660254037844387076, 1.000000000000000000, 0.8660254037844387076, 1.000000000000000000, 0.8660254037844387076, 1.000000000000000000, 0.8660254037844387076, 1.000000000000000000, 0.8660254037844387076, 1.000000000000000000, 0.8660254037844387076, 1.000000000000000000, 0.8660254037844387076, 1.000000000000000000, 0.8660254037844387076, 1.000000000000000000, 0.8660254037844387076, 1.000000000000000000, 0.8660254037844387076, 1.000000000000000000, 0.8660254037844387076, 1.000000000000000000, 0.8660254037844387076, 1.000000000000000000, 0.8660254037844387076, 1.000000000000000000, 0.8660254037844387076, 1.000000000000000000, 0.8660254037844387076, 1.000000000000000000, 0.8660254037844387076, 1.000000000000000000, 0.8660254037844387076, 1.000000000000000000, 0.8660254037844387076, 1.000000000000000000, 0.8660254037844387076, 1.000000000000000000, 0.8660254037844387076, 1.000000000000000000, 0.8660254037844387076, 1.000000000000000000, 0.8660254037844387076, 1.000000000000000000, 0.8660254037844387076, 1.000000000000000000, 0.8660254037844387076, 1.000000000000000000, 0.8660254037844387076, 1.000000000000000000, 0.8660254037844387076, 1.000000000000000000, 0.8660254037844387076, 1.000000000000000000, 0.8660254037844387076, 1.000000000000000000, 0.8660254037844387076, 1.000000000000000000, 0.8660254037844387076, 1.000000000000000000, 0.8660254037844387076, 1.000000000000000000, 0.8660254037844387076, 1.000000000000000000, 0.8660254037844387076, 1.000000000000000000, 0.8660254037844387076, 1.000000000000000000, 0.8660254037844387076, 1.000000000000000000, 0.8660254037844387076, 1.000000000000000000, 0.8660254037844387076, 1.000000000000000000, 0.8660254037844387076, 1.000000000000000000, 0.8660254037844387076, 1.000000000000000000, 0.8660254037844387076, 1.000000000000000000, 0.8660254037844387076, 1.000000000000000000, 0.8660254037844387076, 1.000000000000000000, 0.8660254037844387076, 1.000000000000000000, 0.8660254037844387076, 1.000000000000000000, 0.8660254037844387076, 1.000000000000000000, 0.8660254037844387076, 1.000000000000000000, 0.8660254037844387076, 1.000000000000000000, 0.8660254037844387076, 1.000000000000000000, 0.8660254037844387076, 1.000000000000000000, 0.8660254037844387076, 1.000000000000000000, 0.8660254037844387076, 1.000000000000000000, 0.8660254037844387076, 1.000000000000000000, 0.8660254037844387076, 1.000000000000000000, 0.8660254037844387076, 1.000000000000000000, 0.8660254037844387076, 1.000000000000000000, 0.8660254037844387076, 1.000000000000000000, 0.8660254037844387076, 1.000000000000000000, 0.8660254037844387076, 1.000000000000000000, 0.8660254037844387076, 1.000000000000000000, 0.8660254037844387076, 1.000000000000000000, 0.8660254037844387076, 1.000000000000000000, 0.8660254037844387076, 1.000000000000000000, 0.8660254037844387076, 1.000000000000000000, 0.8660254037844387076, 1.000000000000000000, 0.8660254037844387076, 1.000000000000000000, 0.8660254037844387076, 1.000000000000000000, 0.8660254037844387076, 1.000000000000000000, 0.8660254037844387076, 1.000000000000000000, 0.8660254037844387076, 1.000000000000000000, 0.8660254037844387076, 1.000000000000000000, 0.8660254037844387076, 1.000000000000000000, 0.8660254037844387076, 1.000000000000000000, 0.8660254037844387076, 1.000000000000000000, 0.8660254037844387076, 1.000000000000000000, 0.8660254037844387076, 1.000000000000000000, 0.8660254037844387076, 1.000000000000000000, 0.8660254037844387076, 1.000000000000000000, 0.8660254037844387076, 1.000000000000000000, 0.8660254037844387076, 1.000000000000000000, 0.8660254037844387076, 1.000000000000000000, 0.8660254037844387076, 1.000000000000000000, 0.8660254037844387076, 1.000000000000000000, 0.8660254037844387076, 1.000000000000000000, 0.8660254037844387076, 1.000000000000000000, 0.8660254037844387076, 1.000000000000000000, 0.8660254037844387076, 1.000000000000000000, 0.8660254037844387076, 1.000000000000000000, 0.8660254037844387076, 1.000000000000000000, 0.8660254037844387076, 1.000000000000000000, 0.8660254037844387076, 1.000000000000000000, 0.8660254037844387076, 1.000000000000000000, 0.8660254037844387076, 1.000000000000000000, 0.8660254037844387076, 1.000000000000000000, 0.8660254037844387076, 1.000000000000000000, 0.8660254037844387076, 1.000000000000000000, 0.8660254037844387076, 1.000000000000000000, 0.8660254037844387076, 1.000000000000000000, 0.8660254037844387076, 1.000000000000000000, 0.8660254037844387076, 1.000000000000000000, 0.8660254037844387076, 1.000000000000000000, 0.8660254037844387076, 1.000000000000000000, 0.8660254037844387076, 1.000000000000000000, 0.8660254037844387076, 1.000000000000000000, 0.8660254037844387076, 1.000000000000000000, 0.8660254037844387076, 1.000000000000000000, 0.8660254037844387076, 1.000000000000000000, 0.8660254037844387076, 1.000000000000000000, 0.8660254037844387076, 1.000000000000000000, 0.8660254037844387076, 1.000000000000000000, 0.8660254037844387076, 1.000000000000000000, 0.8660254037844387076, 1.000000000000000000, 0.8660254037844387076, 1.000000000000000000, 0.8660254037844387076, 1.000000000000000000, 0.8660254037844387076, 1.000000000000000000, 0.8660254037844387076, 1.000000000000000000, 0.8660254037844387076, 1.000000000000000000, 0.8660254037844387076, 1.000000000000000000, 0.8660254037844387076, 1.000000000000000000, 0.8660254037844387076, 1.000000000000000000, 0.8660254037844387076, 1.000000000000000000, 0.8660254037844387076, 1.000000000000000000, 0.8660254037844387076, 1.000000000000000000, 0.8660254037844387076, 1.000000000000000000, 0.8660254037844387076, 1.000000000000000000, 0.8660254037844387076, 1.000000000000000000, 0.8660254037844387076, 1.000000000000000000, 0.8660254037844387076, 1.000000000000000000, 0.8660254037844387076, 1.000000000000000000, 0.8660254037844387076, 1.000000000000000000, 0.8660254037844387076, 1.000000000000000000, 0.8660254037844387076, 1.000000000000000000, 0.8660254037844387076, 1.000000000000000000, 0.8660254037844387076, 1.000000000000000000, 0.8660254037844387076, 1.000000000000000000, 0.8660254037844387076, 1.000000000000000000, 0.8660254037844387076, 1.000000000000000000, 0.8660254037844387076, 1.000000000000000000, 0.8660254037844387076, 1.000000000000000000, 0.8660254037844387076, 1.000000000000000000, 0.8660254037844387076, 1.000000000000000000, 0.8660254037844387076, 1.000000000000000000, 0.8660254037844387076, 1.000000000000000000, 0.8660254037844387076, 1.000000000000000000, 0.8660254037844387076, 1.000000000000000000, 0.8660254037844387076, 1.000000000000000000, 0.8660254037844387076, 1.000000000000000000, 0.8660254037844387076, 1.000000000000000000, 0.8660254037844387076, 1.000000000000000000, 0.8660254037844387076, 1.000000000000000000, 0.8660254037844387076, 1.000000000000000000, 0.8660254037844387076, 1.000000000000000000, 0.8660254037844387076, 1.000000000000000000, 0.8660254037844387076, 1.000000000000000000, 0.8660254037844387076, 1.000000000000000000, 0.8660254037844387076, 1.000000000000000000, 0.8660254037844387076, 1.000000000000000000, 0.8660254037844387076, 1.000000000000000000, 0.8660254037844387076, 1.000000000000000000, 0.8660254037844387076, 1.000000000000000000, 0.8660254037844387076, 1.000000000000000000, 0.8660254037844387076, 1.000000000000000000, 0.8660254037844387076, 1.000000000000000000, 0.8660254037844387076, 1.000000000000000000, 0.8660254037844387076, 1.000000000000000000, 0.8660254037844387076, 1.000000000000000000, 0.8660254037844387076, 1.000000000000000000, 0.8660254037844387076, 1.000000000000000000, 0.8660254037844387076, 1.000000000000000000, 0.8660254037844387076, 1.000000000000000000, 0.8660254037844387076, 1.000000000000000000, 0.8660254037844387076, 1.000000000000000000, 0.8660254037844387076, 1.000000000000000000, 0.8660254037844387076, 1.000000000000000000, 0.8660254037844387076, 1.000000000000000000, 0.8660254037844387076, 1.000000000000000000, 0.8660254037844387076, 1.000000000000000000, 0.8660254037844387076, 1.000000000000000000, 0.8660254037844387076, 1.000000000000000000, 0.8660254037844387076, 1.000000000000000000, 0.8660254037844387076, 1.000000000000000000, 0.8660254037844387076, 1.000000000000000000, 0.8660254037844387076, 1.000000000000000000, 0.8660254037844387076, 1.000000000000000000, 0.8660254037844387076, 1.000000000000000000, 0.8660254037844387076, 1.000000000000000000, 0.8660254037844387076, 1.000000000000000000, 0.8660254037844387076, 1.000000000000000000, 0.8660254037844387076, 1.000000000000000000) ) ) 
 REPRESENTATION_ITEM ( '' )  SURFACE ( )  );
#31836 = ADVANCED_FACE ( 'NONE', ( #12890 ), #35423, .F. ) ;
#31837 = CARTESIAN_POINT ( 'NONE',  ( 17.37187500061451573, -6.054752690667223547, -1.112240025338166033E-15 ) ) ;
#31838 = CARTESIAN_POINT ( 'NONE',  ( 21.29062500061451502, -3.027376345333614438, 5.243569643749998122 ) ) ;
#31839 = CARTESIAN_POINT ( 'NONE',  ( 2.000000000000001332, 12.50000000000000000, 33.46410161513774995 ) ) ;
#31840 = CARTESIAN_POINT ( 'NONE',  ( 27.47812500061451502, 4.541064518000418104, 2.621784821874999949 ) ) ;
#31841 = CARTESIAN_POINT ( 'NONE',  ( 6.862500001229034474, -4.330127018922190985, -2.500000000000001332 ) ) ;
#31842 = ORIENTED_EDGE ( 'NONE', *, *, #5278, .T. ) ;
#31843 = CYLINDRICAL_SURFACE ( 'NONE', #58094, 4.999999999999998224 ) ;
#31844 = CARTESIAN_POINT ( 'NONE',  ( -3.999999999999997335, 16.88749999999999929, -27.69059892324149175 ) ) ;
#31845 = CARTESIAN_POINT ( 'NONE',  ( 24.41250000122903430, -4.330127018922190985, -2.500000000000001332 ) ) ;
#31846 = CARTESIAN_POINT ( 'NONE',  ( 1.878215178125000495, 14.62812499938548427, 26.74683588394047007 ) ) ;
#31847 = CARTESIAN_POINT ( 'NONE',  ( 7.584375000614516082, 6.421520780324663323E-16, -5.243569643749999010 ) ) ;
#31848 = CYLINDRICAL_SURFACE ( 'NONE', #1910, 4.999999999999998224 ) ;
#31849 = CARTESIAN_POINT ( 'NONE',  ( 14.31562500061451537, 3.027376345333613106, -5.243569643749998122 ) ) ;
#31850 = CARTESIAN_POINT ( 'NONE',  ( 7.846875000614518036, -3.027376345333614438, 5.243569643749998122 ) ) ;
#31851 = CARTESIAN_POINT ( 'NONE',  ( 27.00000000122903288, -2.886751345948129988, 4.999999999999997335 ) ) ;
#31852 = CARTESIAN_POINT ( 'NONE',  ( 17.59687500061451715, 6.054752690667223547, 3.707466751127219781E-16 ) ) ;
#31853 = CARTESIAN_POINT ( 'NONE',  ( 5.709375000614517859, -4.541064518000417216, -2.621784821875001281 ) ) ;
#31854 = FACE_OUTER_BOUND ( 'NONE', #26933, .T. ) ;
#31855 = CARTESIAN_POINT ( 'NONE',  ( 6.178125000614518747, 6.421520780324663323E-16, -5.243569643749999010 ) ) ;
#31856 = CARTESIAN_POINT ( 'NONE',  ( 16.49062500061451786, -3.027376345333610441, -5.243569643749999898 ) ) ;
#31857 = ORIENTED_EDGE ( 'NONE', *, *, #67743, .F. ) ;
#31858 = CARTESIAN_POINT ( 'NONE',  ( 11.80312500061451608, 0.000000000000000000, 5.243569643749999010 ) ) ;
#31859 = CARTESIAN_POINT ( 'NONE',  ( 5.962500001229033231, -4.330127018922190985, -2.500000000000001332 ) ) ;
#31860 = CARTESIAN_POINT ( 'NONE',  ( 7.828125000614517326, -4.541064518000419881, 2.621784821874995952 ) ) ;
#31861 = CARTESIAN_POINT ( 'NONE',  ( 21.90937500061451715, -4.119189519843965641, -2.378215178125001383 ) ) ;
#31862 = CARTESIAN_POINT ( 'NONE',  ( 9.600000000000001421, 4.330127018922192761, -2.499999999999997780 ) ) ;
#31863 = CARTESIAN_POINT ( 'NONE',  ( 3.900000001229034563, 5.773502691896255534, 3.535250795749688894E-16 ) ) ;
#31864 = CARTESIAN_POINT ( 'NONE',  ( 18.82500000000000284, -4.330127018922194537, 2.499999999999995559 ) ) ;
#31865 = CARTESIAN_POINT ( 'NONE',  ( 18.38437500061451857, 6.421520780324663323E-16, -5.243569643749999010 ) ) ;
#31866 = CARTESIAN_POINT ( 'NONE',  ( 15.15000000122903323, 5.773502691896255534, 3.535250795749688894E-16 ) ) ;
#31867 = CARTESIAN_POINT ( 'NONE',  ( 21.07499999999999929, -4.330127018922194537, 2.499999999999995559 ) ) ;
#31868 = CARTESIAN_POINT ( 'NONE',  ( -2.121784821874996840, 16.72812500061451857, -26.32496088578401583 ) ) ;
#31869 = DIRECTION ( 'NONE',  ( 1.000000000000000000, 0.000000000000000000, 0.000000000000000000 ) ) ;
#31870 = CARTESIAN_POINT ( 'NONE',  ( 1.071796769724485232, 16.13615380933863008, 25.99999999999999645 ) ) ;
#31871 = CARTESIAN_POINT ( 'NONE',  ( 3.617702362022032325, -3.451409801779584452, 3.617702362022032325 ) ) ;
#31872 = CARTESIAN_POINT ( 'NONE',  ( 28.19062500061451715, -3.027376345333610441, -5.243569643749999898 ) ) ;
#31873 = DIRECTION ( 'NONE',  ( -0.000000000000000000, -1.000000000000000000, -0.000000000000000000 ) ) ;
#31874 = DIRECTION ( 'NONE',  ( -1.000000000000000000, -0.000000000000000000, -0.000000000000000000 ) ) ;
#31875 = CARTESIAN_POINT ( 'NONE',  ( 17.10937500061451999, 4.541064518000418104, -2.621784821874998173 ) ) ;
#31876 = CARTESIAN_POINT ( 'NONE',  ( 29.73750000000000071, -2.886751345948125991, -5.000000000000000000 ) ) ;
#31877 = EDGE_CURVE ( 'NONE', #1400, #52020, #52422, .T. ) ;
#31878 = CARTESIAN_POINT ( 'NONE',  ( 10.64062500061451644, -3.027376345333610441, -5.243569643749999898 ) ) ;
#31879 = CARTESIAN_POINT ( 'NONE',  ( 29.52187500061451431, 5.824947211148865298E-16, -4.756430356249998326 ) ) ;
#31880 = CARTESIAN_POINT ( 'NONE',  ( 20.48437500061451289, -4.541064518000419881, 2.621784821874995952 ) ) ;
#31881 = CARTESIAN_POINT ( 'NONE',  ( 15.15937500061451892, 2.746126346562645981, -4.756430356249997438 ) ) ;
#31882 = CARTESIAN_POINT ( 'NONE',  ( 8.053125000614516082, 4.541064518000418104, -2.621784821874998173 ) ) ;
#31883 = CARTESIAN_POINT ( 'NONE',  ( 12.34687500061452070, -3.027376345333614438, 5.243569643749998122 ) ) ;
#31884 = EDGE_LOOP ( 'NONE', ( #23785, #71661, #15987, #7470 ) ) ;
#31885 = CARTESIAN_POINT ( 'NONE',  ( 23.29687500061451644, -3.027376345333610441, -5.243569643749999898 ) ) ;
#31886 = CARTESIAN_POINT ( 'NONE',  ( 28.15312500061451573, -4.541064518000417216, -2.621784821875001281 ) ) ;
#31887 = CARTESIAN_POINT ( 'NONE',  ( 0.000000000000000000, 27.50000000000000000, 30.00000000000000000 ) ) ;
#31888 = CARTESIAN_POINT ( 'NONE',  ( 6.712500000000000355, -5.773502691896255534, -1.060575238724906372E-15 ) ) ;
#31889 = CARTESIAN_POINT ( 'NONE',  ( 17.25000000122903288, -2.886751345948125991, -5.000000000000000000 ) ) ;
#31890 = DIRECTION ( 'NONE',  ( -1.000000000000000000, -0.000000000000000000, -0.000000000000000000 ) ) ;
#31891 = CARTESIAN_POINT ( 'NONE',  ( 7.921875000614517326, 5.824947211148865298E-16, -4.756430356249998326 ) ) ;
#31892 = VERTEX_POINT ( 'NONE', #2185 ) ;
#31893 = CARTESIAN_POINT ( 'NONE',  ( 15.41250000000000142, 2.886751345948129099, -4.999999999999998224 ) ) ;
#31894 = CARTESIAN_POINT ( 'NONE',  ( 19.34999999999999787, -4.330127018922190985, -2.500000000000001332 ) ) ;
#31895 = CARTESIAN_POINT ( 'NONE',  ( 10.86562500061451431, 3.027376345333611329, 5.243569643749999010 ) ) ;
#31896 = ORIENTED_EDGE ( 'NONE', *, *, #20969, .F. ) ;
#31897 = CARTESIAN_POINT ( 'NONE',  ( -3.999999999999997335, 11.03749999999999964, -27.69059892324149530 ) ) ;
#31898 = CARTESIAN_POINT ( 'NONE',  ( -4.243569643749999898, 17.60937500061451999, -30.00000000000000000 ) ) ;
#31899 = CARTESIAN_POINT ( 'NONE',  ( 3.028125000614518392, 6.421520780324663323E-16, -5.243569643749999010 ) ) ;
#31900 = CARTESIAN_POINT ( 'NONE',  ( 9.112500000000000711, 2.886751345948129099, -4.999999999999998224 ) ) ;
#31901 = CARTESIAN_POINT ( 'NONE',  ( 16.10625000122903216, 0.000000000000000000, 4.999999999999998224 ) ) ;
#31902 = EDGE_LOOP ( 'NONE', ( #3214, #35834, #7435, #16992 ) ) ;
#31903 = CARTESIAN_POINT ( 'NONE',  ( 4.243569643749999898, 11.92812500061451608, 30.00000000000000000 ) ) ;
#31904 = CARTESIAN_POINT ( 'NONE',  ( 27.74062500061451431, -3.027376345333610441, -5.243569643749999898 ) ) ;
#31905 = DIRECTION ( 'NONE',  ( 1.000000000000000000, 0.000000000000000000, 0.000000000000000000 ) ) ;
#31906 = CARTESIAN_POINT ( 'NONE',  ( 2.655984681222220721E-16, 20.40312499938548285, 25.66244784525396483 ) ) ;
#31907 = CARTESIAN_POINT ( 'NONE',  ( 21.83437500061451786, -4.541064518000419881, 2.621784821874995952 ) ) ;
#31908 = EDGE_CURVE ( 'NONE', #11892, #32497, #53143, .T. ) ;
#31909 = CARTESIAN_POINT ( 'NONE',  ( 18.02812500061451573, 4.541064518000418104, 2.621784821874999949 ) ) ;
#31910 = CARTESIAN_POINT ( 'NONE',  ( -4.243569643749998122, 14.44062500061459531, -27.54997392385601174 ) ) ;
#31911 = CARTESIAN_POINT ( 'NONE',  ( 22.38750000122903216, 4.330127018922191873, 2.499999999999999556 ) ) ;
#31912 = CARTESIAN_POINT ( 'NONE',  ( 3.590625000614518836, 6.054752690667223547, 3.707466751127219781E-16 ) ) ;
#31913 = CARTESIAN_POINT ( 'NONE',  ( 25.88437500061451502, -4.119189519843968306, 2.378215178124996054 ) ) ;
#31914 = CARTESIAN_POINT ( 'NONE',  ( 22.49062500061451431, 6.054752690667223547, 3.707466751127219781E-16 ) ) ;
#31915 = CARTESIAN_POINT ( 'NONE',  ( 7.621875000614519280, 2.746126346562645981, -4.756430356249997438 ) ) ;
#31916 = CARTESIAN_POINT ( 'NONE',  ( 3.756430356250000546, 15.82812499938548179, 27.83122392262697886 ) ) ;
#31917 = CARTESIAN_POINT ( 'NONE',  ( 15.60937500061451644, -4.541064518000417216, -2.621784821875001281 ) ) ;
#31918 = CARTESIAN_POINT ( 'NONE',  ( 14.74687500061451573, -3.027376345333610441, -5.243569643749999898 ) ) ;
#31919 = CARTESIAN_POINT ( 'NONE',  ( 24.30937500061451573, 4.541064518000418104, -2.621784821874998173 ) ) ;
#31920 = CARTESIAN_POINT ( 'NONE',  ( 4.243569643749999898, 13.33437500061451786, 30.00000000000000000 ) ) ;
#31921 = CARTESIAN_POINT ( 'NONE',  ( 5.803125000614517859, 4.541064518000418104, -2.621784821874998173 ) ) ;
#31922 = CARTESIAN_POINT ( 'NONE',  ( 16.38750000122903216, 6.123233995736764310E-16, -4.999999999999998224 ) ) ;
#31923 = CARTESIAN_POINT ( 'NONE',  ( 28.71562500061451573, 3.027376345333613106, -5.243569643749998122 ) ) ;
#31924 = CARTESIAN_POINT ( 'NONE',  ( 3.999999999999998668, 19.47500000122903430, -32.30940107675850470 ) ) ;
#31925 = CARTESIAN_POINT ( 'NONE',  ( -2.000000000000000000, 18.12500000000000355, 26.53589838486224650 ) ) ;
#31926 = CARTESIAN_POINT ( 'NONE',  ( 6.796875000614516438, 6.054752690667223547, 3.707466751127219781E-16 ) ) ;
#31927 = CARTESIAN_POINT ( 'NONE',  ( 14.21250000122903323, 4.330127018922192761, -2.499999999999997780 ) ) ;
#31928 = CARTESIAN_POINT ( 'NONE',  ( 10.12500000122903465, 2.886751345948129099, -4.999999999999998224 ) ) ;
#31929 = CARTESIAN_POINT ( 'NONE',  ( 5.765625000614519102, 3.027376345333613106, -5.243569643749998122 ) ) ;
#31930 = CARTESIAN_POINT ( 'NONE',  ( -8.484601909799255319E-16, 16.38124999877096499, 34.61880215351700940 ) ) ;
#31931 = CARTESIAN_POINT ( 'NONE',  ( 18.16875000122903216, 2.886751345948129099, -4.999999999999998224 ) ) ;
#31932 = CARTESIAN_POINT ( 'NONE',  ( 14.18437500061451750, -4.541064518000419881, 2.621784821874995952 ) ) ;
#31933 = CARTESIAN_POINT ( 'NONE',  ( 21.07499999999999929, -4.330127018922194537, 2.499999999999995559 ) ) ;
#31934 = ORIENTED_EDGE ( 'NONE', *, *, #37808, .T. ) ;
#31935 = CARTESIAN_POINT ( 'NONE',  ( 21.32812500061451644, -4.541064518000419881, 2.621784821874995952 ) ) ;
#31936 = CARTESIAN_POINT ( 'NONE',  ( 6.703125000614516438, 4.541064518000418104, -2.621784821874998173 ) ) ;
#31937 = CARTESIAN_POINT ( 'NONE',  ( 25.24687500061451573, 6.054752690667223547, 3.707466751127219781E-16 ) ) ;
#31938 = CARTESIAN_POINT ( 'NONE',  ( 7.228125000614517681, 4.541064518000418104, 2.621784821874999949 ) ) ;
#31939 = CARTESIAN_POINT ( 'NONE',  ( -4.000000000000000888, 16.30624999877096570, 32.30940107675850470 ) ) ;
#31940 = CARTESIAN_POINT ( 'NONE',  ( 7.200000001229035718, -2.886751345948129988, 4.999999999999997335 ) ) ;
#31941 = EDGE_CURVE ( 'NONE', #36195, #45966, #69788, .T. ) ;
#31942 = CARTESIAN_POINT ( 'NONE',  ( 22.26562500061451644, -6.054752690667223547, -1.112240025338166033E-15 ) ) ;
#31943 = CARTESIAN_POINT ( 'NONE',  ( -2.000000000000000000, 19.58750000122903501, -33.46410161513775705 ) ) ;
#31944 = CARTESIAN_POINT ( 'NONE',  ( 11.02500000122903501, 2.886751345948129099, -4.999999999999998224 ) ) ;
#31945 = CARTESIAN_POINT ( 'NONE',  ( 19.07812500061451644, -4.541064518000419881, 2.621784821874995952 ) ) ;
#31946 = CARTESIAN_POINT ( 'NONE',  ( 18.59062500061451573, -3.027376345333614438, 5.243569643749998122 ) ) ;
#31947 = CARTESIAN_POINT ( 'NONE',  ( 28.62187500061451573, -5.492252693125287522, -1.008910452111647106E-15 ) ) ;
#31948 = CARTESIAN_POINT ( 'NONE',  ( 18.71249999999999858, 2.886751345948126879, 4.999999999999999112 ) ) ;
#31949 = CARTESIAN_POINT ( 'NONE',  ( 12.45000000122903394, 5.773502691896255534, 3.535250795749688894E-16 ) ) ;
#31950 = CARTESIAN_POINT ( 'NONE',  ( 8.128125000614515372, 4.541064518000418104, 2.621784821874999949 ) ) ;
#31951 = CARTESIAN_POINT ( 'NONE',  ( 11.46562500061451573, -6.054752690667223547, -1.112240025338166033E-15 ) ) ;
#31952 = CARTESIAN_POINT ( 'NONE',  ( 22.23750000122903003, 6.123233995736764310E-16, -4.999999999999998224 ) ) ;
#31953 = CARTESIAN_POINT ( 'NONE',  ( 21.72187500061451715, 3.027376345333611329, 5.243569643749999010 ) ) ;
#31954 = CARTESIAN_POINT ( 'NONE',  ( 10.25625000122903252, 0.000000000000000000, 4.999999999999998224 ) ) ;
#31955 = CARTESIAN_POINT ( 'NONE',  ( 4.762500001229033941, 4.330127018922192761, -2.499999999999997780 ) ) ;
#31956 = CARTESIAN_POINT ( 'NONE',  ( 4.396875000614516971, -3.027376345333610441, -5.243569643749999898 ) ) ;
#31957 = CARTESIAN_POINT ( 'NONE',  ( 23.55937500061451573, 0.000000000000000000, 5.243569643749999010 ) ) ;
#31958 = CARTESIAN_POINT ( 'NONE',  ( 4.305309508024516063, -2.542763747326308277, -4.514440081878920985 ) ) ;
#31959 = CARTESIAN_POINT ( 'NONE',  ( 18.29062500061451502, -3.027376345333610441, -5.243569643749999898 ) ) ;
#31960 = CARTESIAN_POINT ( 'NONE',  ( 24.90937500061451715, 0.000000000000000000, 5.243569643749999010 ) ) ;
#31961 = CARTESIAN_POINT ( 'NONE',  ( -3.756430356249999214, 18.79062499938548214, 27.83122392262697176 ) ) ;
#31962 = CARTESIAN_POINT ( 'NONE',  ( -1.071796769724504328, 11.20490381179670081, -26.00000000000001066 ) ) ;
#31963 = CYLINDRICAL_SURFACE ( 'NONE', #53687, 1.500000000000000444 ) ;
#31964 = CARTESIAN_POINT ( 'NONE',  ( 6.421875000614519102, 3.027376345333611329, 5.243569643749999010 ) ) ;
#31965 = CARTESIAN_POINT ( 'NONE',  ( 15.21562500061451750, 3.027376345333613106, -5.243569643749998122 ) ) ;
#31966 = CARTESIAN_POINT ( 'NONE',  ( 12.60937500061451821, 4.541064518000418104, -2.621784821874998173 ) ) ;
#31967 = ORIENTED_EDGE ( 'NONE', *, *, #44349, .T. ) ;
#31968 = CARTESIAN_POINT ( 'NONE',  ( 45.00000000000000000, 0.000000000000000000, 0.000000000000000000 ) ) ;
#31969 = CARTESIAN_POINT ( 'NONE',  ( 24.47812500061451502, -4.541064518000419881, 2.621784821874995952 ) ) ;
#31970 = CARTESIAN_POINT ( 'NONE',  ( -3.137519842735245283E-14, 12.91250000000000142, -26.00000000000000711 ) ) ;
#31971 = CARTESIAN_POINT ( 'NONE',  ( 2.417052323292336544E-14, 20.48749999999999716, 34.00000000000000000 ) ) ;
#31972 = CARTESIAN_POINT ( 'NONE',  ( 15.03749999999999964, 5.773502691896255534, 3.535250795749688894E-16 ) ) ;
#31973 = CARTESIAN_POINT ( 'NONE',  ( 25.08750000122903145, 4.330127018922191873, 2.499999999999999556 ) ) ;
#31974 = CARTESIAN_POINT ( 'NONE',  ( 19.45312500061451644, 0.000000000000000000, 5.243569643749999010 ) ) ;
#31975 = ORIENTED_EDGE ( 'NONE', *, *, #50679, .F. ) ;
#31976 = CARTESIAN_POINT ( 'NONE',  ( 23.58749999999999858, 5.773502691896255534, 3.535250795749688894E-16 ) ) ;
#31977 =( BOUNDED_CURVE ( )  B_SPLINE_CURVE ( 2, ( #62537, #68818, #11215, #23008, #33741, #144, #29290, #5311, #68452 ),
 .UNSPECIFIED., .F., .F. ) 
 B_SPLINE_CURVE_WITH_KNOTS ( ( 3, 2, 2, 2, 3 ),
 ( 0.7500000000000000000, 0.7536231884057971175, 0.7608695652173913526, 0.7681159420289854767, 0.7717391304347825942 ),
 .UNSPECIFIED. ) 
 CURVE ( )  GEOMETRIC_REPRESENTATION_ITEM ( )  RATIONAL_B_SPLINE_CURVE ( ( 0.9330127018922194093, 0.9330127018922194093, 1.000000000000000000, 0.8660254037844387076, 1.000000000000000000, 0.8660254037844387076, 1.000000000000000000, 0.9330127018922194093, 0.9330127018922194093 ) ) 
 REPRESENTATION_ITEM ( '' )  );
#31978 = EDGE_CURVE ( 'NONE', #53311, #7820, #3026, .T. ) ;
#31979 = CARTESIAN_POINT ( 'NONE',  ( 24.42187500061451999, 3.027376345333611329, 5.243569643749999010 ) ) ;
#31980 = VERTEX_POINT ( 'NONE', #68698 ) ;
#31981 = CARTESIAN_POINT ( 'NONE',  ( 2.983212779636571277, -4.012535546436136968, -3.375586037630073033 ) ) ;
#31982 = CARTESIAN_POINT ( 'NONE',  ( 10.94062500061451537, -3.027376345333614438, 5.243569643749998122 ) ) ;
#31983 = CARTESIAN_POINT ( 'NONE',  ( 3.178125000614515638, 4.541064518000418104, 2.621784821874999949 ) ) ;
#31984 = CARTESIAN_POINT ( 'NONE',  ( 13.84687500061451715, 4.119189519843966529, -2.378215178124998275 ) ) ;
#31985 = CARTESIAN_POINT ( 'NONE',  ( 27.66562500061451146, -6.054752690667223547, -1.112240025338166033E-15 ) ) ;
#31986 = CARTESIAN_POINT ( 'NONE',  ( 16.68750000000000000, -2.886751345948125991, -5.000000000000000000 ) ) ;
#31987 = CARTESIAN_POINT ( 'NONE',  ( 25.57499999999999929, -4.330127018922194537, 2.499999999999995559 ) ) ;
#31988 = CARTESIAN_POINT ( 'NONE',  ( 3.999999999999998668, 10.81250000000000178, -32.30940107675850470 ) ) ;
#31989 = CARTESIAN_POINT ( 'NONE',  ( 7.846875000614518036, -3.027376345333614438, 5.243569643749998122 ) ) ;
#31990 = CARTESIAN_POINT ( 'NONE',  ( 16.88437500061451502, -4.541064518000419881, 2.621784821874995952 ) ) ;
#31991 = CARTESIAN_POINT ( 'NONE',  ( 65.00000000000000000, 0.000000000000000000, 0.000000000000000000 ) ) ;
#31992 = EDGE_LOOP ( 'NONE', ( #17725, #55241, #61873, #24191 ) ) ;
#31993 = CARTESIAN_POINT ( 'NONE',  ( 26.35312500061451857, -4.541064518000417216, -2.621784821875001281 ) ) ;
#31994 = CARTESIAN_POINT ( 'NONE',  ( 26.93437500061451573, 6.421520780324663323E-16, -5.243569643749999010 ) ) ;
#31995 = CARTESIAN_POINT ( 'NONE',  ( -3.999999999999999112, 14.88124999877096677, 27.69059892324149530 ) ) ;
#31996 = CARTESIAN_POINT ( 'NONE',  ( 13.79999999999999893, 0.000000000000000000, 4.999999999999998224 ) ) ;
#31997 = CARTESIAN_POINT ( 'NONE',  ( 10.67812500061451608, 6.421520780324663323E-16, -5.243569643749999010 ) ) ;
#31998 = CARTESIAN_POINT ( 'NONE',  ( 16.42500000000000071, 4.330127018922191873, 2.499999999999999556 ) ) ;
#31999 = CARTESIAN_POINT ( 'NONE',  ( 25.83750000122903501, 6.123233995736764310E-16, -4.999999999999998224 ) ) ;
#32000 = CARTESIAN_POINT ( 'NONE',  ( 28.11562500061451431, -6.054752690667223547, -1.112240025338166033E-15 ) ) ;
#32001 = CARTESIAN_POINT ( 'NONE',  ( 15.18750000122903465, 4.330127018922191873, 2.499999999999999556 ) ) ;
#32002 = CARTESIAN_POINT ( 'NONE',  ( 45.00000000000000000, 6.123233995736764310E-16, -4.999999999999998224 ) ) ;
#32003 = CARTESIAN_POINT ( 'NONE',  ( 14.93437500061451750, 4.119189519843966529, 2.378215178124999607 ) ) ;
#32004 = CARTESIAN_POINT ( 'NONE',  ( 4.640625000614518214, -3.027376345333614438, 5.243569643749998122 ) ) ;
#32005 = CARTESIAN_POINT ( 'NONE',  ( 21.49687500061451573, -3.027376345333610441, -5.243569643749999898 ) ) ;
#32006 = CARTESIAN_POINT ( 'NONE',  ( -2.121784821874996840, 18.13437500061451502, 33.67503911421598417 ) ) ;
#32007 = CARTESIAN_POINT ( 'NONE',  ( 23.07187500061451857, 3.027376345333611329, 5.243569643749999010 ) ) ;
#32008 = CARTESIAN_POINT ( 'NONE',  ( 4.724999999999999645, 4.330127018922191873, 2.499999999999999556 ) ) ;
#32009 = CARTESIAN_POINT ( 'NONE',  ( -2.828200636599751609E-16, 11.00000000122903288, 25.38119784648299770 ) ) ;
#32010 = CARTESIAN_POINT ( 'NONE',  ( 12.21562500061451573, 3.027376345333611329, 5.243569643749999010 ) ) ;
#32011 = CARTESIAN_POINT ( 'NONE',  ( 4.800000001229032698, 5.773502691896255534, 3.535250795749688894E-16 ) ) ;
#32012 = CARTESIAN_POINT ( 'NONE',  ( 9.534375000614517148, 4.541064518000418104, 2.621784821874999949 ) ) ;
#32013 = CARTESIAN_POINT ( 'NONE',  ( 13.08750000000000213, -2.886751345948126435, -5.000000000000000000 ) ) ;
#32014 = CARTESIAN_POINT ( 'NONE',  ( 9.928125000614517859, 4.541064518000418104, 2.621784821874999949 ) ) ;
#32015 = CARTESIAN_POINT ( 'NONE',  ( 15.04687500061451644, -3.027376345333614438, 5.243569643749998122 ) ) ;
#32016 = CARTESIAN_POINT ( 'NONE',  ( 21.97500000122903074, 2.886751345948126879, 4.999999999999999112 ) ) ;
#32017 = CARTESIAN_POINT ( 'NONE',  ( 11.40937500061451892, 0.000000000000000000, 5.243569643749999010 ) ) ;
#32018 = CARTESIAN_POINT ( 'NONE',  ( 11.46562500061451573, -6.054752690667223547, -1.112240025338166033E-15 ) ) ;
#32019 = CARTESIAN_POINT ( 'NONE',  ( 28.96875000122903288, 2.886751345948129099, -4.999999999999998224 ) ) ;
#32020 = CARTESIAN_POINT ( 'NONE',  ( 20.33437500061451786, 4.541064518000418104, 2.621784821874999949 ) ) ;
#32021 = DIRECTION ( 'NONE',  ( 0.000000000000000000, 0.000000000000000000, 1.000000000000000000 ) ) ;
#32022 = EDGE_CURVE ( 'NONE', #68374, #60259, #41697, .T. ) ;
#32023 = CARTESIAN_POINT ( 'NONE',  ( -2.000000000000000000, 19.92500000000000071, -33.46410161513775705 ) ) ;
#32024 = CARTESIAN_POINT ( 'NONE',  ( 4.243569643749999010, 15.62187500061451928, -32.45002607614398471 ) ) ;
#32025 = CARTESIAN_POINT ( 'NONE',  ( 16.35000000122903430, -2.886751345948125991, -5.000000000000000000 ) ) ;
#32026 = CARTESIAN_POINT ( 'NONE',  ( 10.32187500061451679, 3.027376345333613106, -5.243569643749998122 ) ) ;
#32027 = CARTESIAN_POINT ( 'NONE',  ( 4.243569643749999898, 16.87812500061451715, -30.00000000000000000 ) ) ;
#32028 = CARTESIAN_POINT ( 'NONE',  ( 17.77500000122903145, 2.886751345948129099, -4.999999999999998224 ) ) ;
#32029 = CARTESIAN_POINT ( 'NONE',  ( 9.328125000614518214, 6.421520780324663323E-16, -5.243569643749999010 ) ) ;
#32030 = ORIENTED_EDGE ( 'NONE', *, *, #54265, .F. ) ;
#32031 = CARTESIAN_POINT ( 'NONE',  ( 15.37500000000000000, 6.123233995736764310E-16, -4.999999999999998224 ) ) ;
#32032 = CARTESIAN_POINT ( 'NONE',  ( 29.17500000000000071, -4.330127018922194537, 2.499999999999995559 ) ) ;
#32033 = CARTESIAN_POINT ( 'NONE',  ( 10.54687500061451644, -3.027376345333614438, 5.243569643749998122 ) ) ;
#32034 = CARTESIAN_POINT ( 'NONE',  ( 28.08750000122903145, 6.123233995736764310E-16, -4.999999999999998224 ) ) ;
#32035 = EDGE_CURVE ( 'NONE', #48144, #32339, #64591, .T. ) ;
#32036 = CARTESIAN_POINT ( 'NONE',  ( 9.450000001229033941, -2.886751345948129988, 4.999999999999997335 ) ) ;
#32037 = CARTESIAN_POINT ( 'NONE',  ( 18.52500000122903145, -5.773502691896255534, -1.060575238724906372E-15 ) ) ;
#32038 =( BOUNDED_CURVE ( )  B_SPLINE_CURVE ( 1, ( #72035, #66867 ),
 .UNSPECIFIED., .F., .F. ) 
 B_SPLINE_CURVE_WITH_KNOTS ( ( 2, 2 ),
 ( 0.000000000000000000, 1.000000000000000000 ),
 .UNSPECIFIED. ) 
 CURVE ( )  GEOMETRIC_REPRESENTATION_ITEM ( )  RATIONAL_B_SPLINE_CURVE ( ( 0.9401540804572410259, 0.9401540804572410259 ) ) 
 REPRESENTATION_ITEM ( '' )  );
#32039 = EDGE_CURVE ( 'NONE', #37430, #47010, #39157, .T. ) ;
#32040 = CARTESIAN_POINT ( 'NONE',  ( 14.39062500061451821, 6.054752690667223547, 3.707466751127219781E-16 ) ) ;
#32041 = CARTESIAN_POINT ( 'NONE',  ( 18.70312500061451644, -4.541064518000417216, -2.621784821875001281 ) ) ;
#32042 = CARTESIAN_POINT ( 'NONE',  ( 28.72500000122903074, 2.886751345948126879, 4.999999999999999112 ) ) ;
#32043 =( BOUNDED_CURVE ( )  B_SPLINE_CURVE ( 2, ( #33790, #11629, #5723, #62943, #57400, #192, #34145 ),
 .UNSPECIFIED., .F., .F. ) 
 B_SPLINE_CURVE_WITH_KNOTS ( ( 3, 2, 2, 3 ),
 ( 0.8300000000000000711, 0.8333333333333334814, 0.8366666666666666696, 0.8399999999999999689 ),
 .UNSPECIFIED. ) 
 CURVE ( )  GEOMETRIC_REPRESENTATION_ITEM ( )  RATIONAL_B_SPLINE_CURVE ( ( 0.9999999999999955591, 0.8660254037844431485, 1.000000000000000000, 0.8660254037844387076, 1.000000000000000000, 0.8660254037844387076, 1.000000000000000000 ) ) 
 REPRESENTATION_ITEM ( '' )  );
#32044 = CARTESIAN_POINT ( 'NONE',  ( 3.140625000614516882, 6.054752690667223547, 3.707466751127219781E-16 ) ) ;
#32045 = CARTESIAN_POINT ( 'NONE',  ( 24.11249999999999716, 2.886751345948126879, 4.999999999999999112 ) ) ;
#32046 = CARTESIAN_POINT ( 'NONE',  ( 3.756430356250000102, 14.44062499938548250, 30.00000000000000000 ) ) ;
#32047 = CARTESIAN_POINT ( 'NONE',  ( 26.21249999999999858, 2.886751345948129099, -4.999999999999998224 ) ) ;
#32048 = CARTESIAN_POINT ( 'NONE',  ( 26.18437500061451573, 4.541064518000418104, 2.621784821874999949 ) ) ;
#32049 = CARTESIAN_POINT ( 'NONE',  ( 1.999999999999998668, 17.60000000000000142, 26.53589838486224650 ) ) ;
#32050 = CARTESIAN_POINT ( 'NONE',  ( 13.50000000122903288, -2.886751345948129988, 4.999999999999997335 ) ) ;
#32051 = CARTESIAN_POINT ( 'NONE',  ( 4.312500000000000000, 2.886751345948126879, 4.999999999999999112 ) ) ;
#32052 = DIRECTION ( 'NONE',  ( 1.000000000000000000, 0.000000000000000000, 0.000000000000000000 ) ) ;
#32053 =( BOUNDED_CURVE ( )  B_SPLINE_CURVE ( 2, ( #37709, #32906, #26269, #54351, #60598, #66155, #4836 ),
 .UNSPECIFIED., .F., .F. ) 
 B_SPLINE_CURVE_WITH_KNOTS ( ( 3, 2, 2, 3 ),
 ( 0.5166666666666666075, 0.5194444444444443754, 0.5222222222222222543, 0.5250000000000000222 ),
 .UNSPECIFIED. ) 
 CURVE ( )  GEOMETRIC_REPRESENTATION_ITEM ( )  RATIONAL_B_SPLINE_CURVE ( ( 1.000000000000005329, 0.8660254037844333785, 1.000000000000000000, 0.8660254037844387076, 1.000000000000000000, 0.8660254037844387076, 1.000000000000000000 ) ) 
 REPRESENTATION_ITEM ( '' )  );
#32054 = CARTESIAN_POINT ( 'NONE',  ( 6.946875000614517681, -3.027376345333614438, 5.243569643749998122 ) ) ;
#32055 = CARTESIAN_POINT ( 'NONE',  ( 24.92812500061451431, -4.541064518000419881, 2.621784821874995952 ) ) ;
#32056 = CARTESIAN_POINT ( 'NONE',  ( 2.000000000000000444, 17.07499999999999929, 26.53589838486224650 ) ) ;
#32057 = CARTESIAN_POINT ( 'NONE',  ( 45.00000000000000000, 1.494782592887656580, -8.875000000000001776 ) ) ;
#32058 = CARTESIAN_POINT ( 'NONE',  ( 5.709375000614517859, -4.541064518000417216, -2.621784821875001281 ) ) ;
#32059 = CARTESIAN_POINT ( 'NONE',  ( 7.659375000614518036, 4.541064518000418104, -2.621784821874998173 ) ) ;
#32060 = CARTESIAN_POINT ( 'NONE',  ( 3.787500000000002753, 5.773502691896255534, 3.535250795749688894E-16 ) ) ;
#32061 = EDGE_CURVE ( 'NONE', #54392, #11624, #44332, .T. ) ;
#32062 = CARTESIAN_POINT ( 'NONE',  ( 2.121784821875001281, 13.20312500061459637, 33.67503911421598417 ) ) ;
#32063 = CARTESIAN_POINT ( 'NONE',  ( 22.34999999999999787, 0.000000000000000000, 4.999999999999998224 ) ) ;
#32064 = AXIS2_PLACEMENT_3D ( 'NONE', #65908, #61093, #16021 ) ;
#32065 = CARTESIAN_POINT ( 'NONE',  ( 28.76249999999999929, -5.773502691896255534, -1.060575238724906372E-15 ) ) ;
#32066 = CARTESIAN_POINT ( 'NONE',  ( 3.000000000000002665, 0.000000000000000000, 4.999999999999998224 ) ) ;
#32067 = ORIENTED_EDGE ( 'NONE', *, *, #35738, .T. ) ;
#32068 = CARTESIAN_POINT ( 'NONE',  ( 18.66562500061451146, -6.054752690667223547, -1.112240025338166033E-15 ) ) ;
#32069 = CARTESIAN_POINT ( 'NONE',  ( 10.67812500061451608, 6.421520780324663323E-16, -5.243569643749999010 ) ) ;
#32070 = CARTESIAN_POINT ( 'NONE',  ( 21.49687500061451573, 4.119189519843966529, -2.378215178124998275 ) ) ;
#32071 = CARTESIAN_POINT ( 'NONE',  ( 6.346875000614517148, 6.054752690667223547, 3.707466751127219781E-16 ) ) ;
#32072 = CARTESIAN_POINT ( 'NONE',  ( 22.68750000000000000, 5.773502691896255534, 3.535250795749688894E-16 ) ) ;
#32073 = CARTESIAN_POINT ( 'NONE',  ( 19.76250000122903216, 0.000000000000000000, 4.999999999999998224 ) ) ;
#32074 = DIRECTION ( 'NONE',  ( -1.000000000000000000, -0.000000000000000000, -0.000000000000000000 ) ) ;
#32075 = CARTESIAN_POINT ( 'NONE',  ( 9.459375000614517859, 4.541064518000418104, -2.621784821874998173 ) ) ;
#32076 = CARTESIAN_POINT ( 'NONE',  ( 14.89687500061451786, 6.054752690667223547, 3.707466751127219781E-16 ) ) ;
#32077 = CARTESIAN_POINT ( 'NONE',  ( 24.34687500061451715, 6.054752690667223547, 3.707466751127219781E-16 ) ) ;
#32078 = DIRECTION ( 'NONE',  ( 0.000000000000000000, 0.000000000000000000, -1.000000000000000000 ) ) ;
#32079 = CARTESIAN_POINT ( 'NONE',  ( 13.23750000000000071, 5.773502691896255534, 3.535250795749688894E-16 ) ) ;
#32080 = CARTESIAN_POINT ( 'NONE',  ( 17.10937500061451999, 4.541064518000418104, -2.621784821874998173 ) ) ;
#32081 = CARTESIAN_POINT ( 'NONE',  ( 9.759375000614516793, -4.541064518000417216, -2.621784821875001281 ) ) ;
#32082 = CARTESIAN_POINT ( 'NONE',  ( 3.756430356249998770, 20.36562499938548143, 32.16877607737302469 ) ) ;
#32083 = CARTESIAN_POINT ( 'NONE',  ( 20.81250000000000000, 2.886751345948129099, -4.999999999999998224 ) ) ;
#32084 = CARTESIAN_POINT ( 'NONE',  ( -2.000000000000001776, 15.50000000000000000, 33.46410161513775705 ) ) ;
#32085 = CARTESIAN_POINT ( 'NONE',  ( -4.243569643749997233, 10.89687500061451786, -27.54997392385601174 ) ) ;
#32086 = CARTESIAN_POINT ( 'NONE',  ( 25.95937500061451431, -4.119189519843965641, -2.378215178125001383 ) ) ;
#32087 = CARTESIAN_POINT ( 'NONE',  ( 11.27812500061451573, 4.541064518000418104, 2.621784821874999949 ) ) ;
#32088 = CARTESIAN_POINT ( 'NONE',  ( 29.14687500061451075, -3.027376345333610441, -5.243569643749999898 ) ) ;
#32089 = CARTESIAN_POINT ( 'NONE',  ( 13.40625000122903288, 0.000000000000000000, 4.999999999999998224 ) ) ;
#32090 = CARTESIAN_POINT ( 'NONE',  ( 7.320879633048903241E-15, 17.75000000122903288, -34.00000000000000000 ) ) ;
#32091 = CARTESIAN_POINT ( 'NONE',  ( 12.44999999999999929, 0.000000000000000000, 4.999999999999998224 ) ) ;
#32092 = CARTESIAN_POINT ( 'NONE',  ( 3.999999999999999112, 17.63750000122903572, 30.00000000000000000 ) ) ;
#32093 = CARTESIAN_POINT ( 'NONE',  ( 12.52500000122903145, 2.886751345948126879, 4.999999999999999112 ) ) ;
#32094 = CARTESIAN_POINT ( 'NONE',  ( 21.27187500061451786, 3.027376345333611329, 5.243569643749999010 ) ) ;
#32095 = CARTESIAN_POINT ( 'NONE',  ( 15.90937500061451892, 0.000000000000000000, 5.243569643749999010 ) ) ;
#32096 = EDGE_LOOP ( 'NONE', ( #72700, #40045, #22628, #24139 ) ) ;
#32097 = CARTESIAN_POINT ( 'NONE',  ( 16.71562500061451573, 3.027376345333611329, 5.243569643749999010 ) ) ;
#32098 = CARTESIAN_POINT ( 'NONE',  ( 28.53750000122903074, 6.123233995736764310E-16, -4.999999999999998224 ) ) ;
#32099 = CARTESIAN_POINT ( 'NONE',  ( 16.99687500061451573, -3.027376345333610441, -5.243569643749999898 ) ) ;
#32100 = CARTESIAN_POINT ( 'NONE',  ( 3.553125000614516082, 4.541064518000418104, -2.621784821874998173 ) ) ;
#32101 = CARTESIAN_POINT ( 'NONE',  ( 18.29062500061451502, -3.027376345333610441, -5.243569643749999898 ) ) ;
#32102 = CARTESIAN_POINT ( 'NONE',  ( -1.487416814333745711E-14, 16.96250000000000213, -26.00000000000000000 ) ) ;
#32103 = CARTESIAN_POINT ( 'NONE',  ( 29.25937500061451502, 4.541064518000418104, -2.621784821874998173 ) ) ;
#32104 = CARTESIAN_POINT ( 'NONE',  ( -4.243569643749999898, 12.11562500061451608, 27.54997392385601529 ) ) ;
#32105 = CARTESIAN_POINT ( 'NONE',  ( 17.02500000122903145, 2.886751345948126879, 4.999999999999999112 ) ) ;
#32106 = CARTESIAN_POINT ( 'NONE',  ( 9.684375000614517504, -4.119189519843968306, 2.378215178124996054 ) ) ;
#32107 = CARTESIAN_POINT ( 'NONE',  ( 25.94062500061451715, -3.027376345333610441, -5.243569643749999898 ) ) ;
#32108 = CARTESIAN_POINT ( 'NONE',  ( 4.000000000000000000, 18.74374999877096570, 30.00000000000000000 ) ) ;
#32109 = CARTESIAN_POINT ( 'NONE',  ( 19.50937500061451857, 0.000000000000000000, 5.243569643749999010 ) ) ;
#32110 = CARTESIAN_POINT ( 'NONE',  ( 22.08750000122903501, -4.330127018922194537, 2.499999999999995559 ) ) ;
#32111 = CARTESIAN_POINT ( 'NONE',  ( 23.46562500061451573, 3.027376345333611329, 5.243569643749999010 ) ) ;
#32112 = CARTESIAN_POINT ( 'NONE',  ( 16.95937500061451786, -4.541064518000417216, -2.621784821875001281 ) ) ;
#32113 = CARTESIAN_POINT ( 'NONE',  ( 11.42812500061451608, -4.541064518000419881, 2.621784821874995952 ) ) ;
#32114 = CARTESIAN_POINT ( 'NONE',  ( 4.243569643749999898, 15.54687500061451644, 32.45002607614398471 ) ) ;
#32115 = CARTESIAN_POINT ( 'NONE',  ( 17.05312500061451786, 4.541064518000418104, -2.621784821874998173 ) ) ;
#32116 = CARTESIAN_POINT ( 'NONE',  ( 28.67812500061451431, 6.421520780324663323E-16, -5.243569643749999010 ) ) ;
#32117 = ORIENTED_EDGE ( 'NONE', *, *, #28533, .T. ) ;
#32118 = ORIENTED_EDGE ( 'NONE', *, *, #65260, .T. ) ;
#32119 = CARTESIAN_POINT ( 'NONE',  ( 22.80000000000000071, 0.000000000000000000, 4.999999999999998224 ) ) ;
#32120 = CARTESIAN_POINT ( 'NONE',  ( 2.121784821875001281, 18.20937500061451786, -26.32496088578401938 ) ) ;
#32121 = CARTESIAN_POINT ( 'NONE',  ( 0.000000000000000000, -4.999999999999998224, 0.000000000000000000 ) ) ;
#32122 = CARTESIAN_POINT ( 'NONE',  ( 25.49062500061451786, -3.027376345333610441, -5.243569643749999898 ) ) ;
#32123 = CARTESIAN_POINT ( 'NONE',  ( 5.840625000614516615, 6.054752690667223547, 3.707466751127219781E-16 ) ) ;
#32124 = CARTESIAN_POINT ( 'NONE',  ( 16.46250000122903501, 4.330127018922192761, -2.499999999999997780 ) ) ;
#32125 = CARTESIAN_POINT ( 'NONE',  ( 21.44062500061452070, -3.027376345333610441, -5.243569643749999898 ) ) ;
#32126 = CARTESIAN_POINT ( 'NONE',  ( 23.06250000000000355, 2.886751345948129099, -4.999999999999998224 ) ) ;
#32127 = CARTESIAN_POINT ( 'NONE',  ( 26.72812500061451502, -4.541064518000419881, 2.621784821874995952 ) ) ;
#32128 = CARTESIAN_POINT ( 'NONE',  ( 7.265625000614516438, 3.027376345333611329, 5.243569643749999010 ) ) ;
#32129 = VERTEX_POINT ( 'NONE', #44971 ) ;
#32130 = B_SPLINE_CURVE_WITH_KNOTS ( 'NONE', 3,
 ( #42690, #70760, #3540, #14972, #43431, #43057, #26431, #59292, #4278, #20135 ),
 .UNSPECIFIED., .F., .F.,
 ( 4, 3, 3, 4 ),
 ( 0.000000000000000000, 0.0001572273160846694696, 0.0003144546168236625494, 0.0005074023328272463454 ),
 .UNSPECIFIED. ) ;
#32131 = CARTESIAN_POINT ( 'NONE',  ( 23.12812500061451360, -4.541064518000419881, 2.621784821874995952 ) ) ;
#32132 = CARTESIAN_POINT ( 'NONE',  ( 6.253125000614517148, 4.541064518000418104, -2.621784821874998173 ) ) ;
#32133 = CARTESIAN_POINT ( 'NONE',  ( 12.19687500061451679, 5.492252693125287522, 3.363034840372157021E-16 ) ) ;
#32134 = CARTESIAN_POINT ( 'NONE',  ( 3.590625000614518836, 6.054752690667223547, 3.707466751127219781E-16 ) ) ;
#32135 = CARTESIAN_POINT ( 'NONE',  ( -3.999999999999999112, 12.91250000122903430, -30.00000000000000000 ) ) ;
#32136 = EDGE_CURVE ( 'NONE', #62008, #24437, #8956, .T. ) ;
#32137 = DIRECTION ( 'NONE',  ( -0.000000000000000000, -1.000000000000000000, -0.000000000000000000 ) ) ;
#32138 = CARTESIAN_POINT ( 'NONE',  ( 10.57500000000000107, 4.330127018922191873, 2.499999999999999556 ) ) ;
#32139 = CARTESIAN_POINT ( 'NONE',  ( 12.42187500061451821, -6.054752690667223547, -1.112240025338166033E-15 ) ) ;
#32140 = CARTESIAN_POINT ( 'NONE',  ( 5.550000001229032698, -2.886751345948125991, -5.000000000000000000 ) ) ;
#32141 = CARTESIAN_POINT ( 'NONE',  ( 14.63437500061451679, -4.541064518000419881, 2.621784821874995952 ) ) ;
#32142 = CARTESIAN_POINT ( 'NONE',  ( 5.221875000614519813, -6.054752690667223547, -1.112240025338166033E-15 ) ) ;
#32143 = CARTESIAN_POINT ( 'NONE',  ( 1.999999999999998668, 18.50000000000000000, 26.53589838486224650 ) ) ;
#32144 = CARTESIAN_POINT ( 'NONE',  ( 19.72499999999999787, -4.330127018922194537, 2.499999999999995559 ) ) ;
#32145 = CARTESIAN_POINT ( 'NONE',  ( 13.73437500061451821, -4.541064518000419881, 2.621784821874995952 ) ) ;
#32146 = DIRECTION ( 'NONE',  ( -0.000000000000000000, -1.000000000000000000, -0.000000000000000000 ) ) ;
#32147 = CARTESIAN_POINT ( 'NONE',  ( 22.97812500061451857, 4.541064518000418104, 2.621784821874999949 ) ) ;
#32148 = ADVANCED_FACE ( 'NONE', ( #34227 ), #22424, .F. ) ;
#32149 = CARTESIAN_POINT ( 'NONE',  ( 2.000000000000001332, 11.60000000000000142, 33.46410161513774995 ) ) ;
#32150 = CARTESIAN_POINT ( 'NONE',  ( 30.00000000000000000, 0.000000000000000000, 0.000000000000000000 ) ) ;
#32151 = CARTESIAN_POINT ( 'NONE',  ( 23.44687500061451502, 6.054752690667223547, 3.707466751127219781E-16 ) ) ;
#32152 = DIRECTION ( 'NONE',  ( 1.000000000000000000, 0.000000000000000000, 0.000000000000000000 ) ) ;
#32153 = EDGE_CURVE ( 'NONE', #2641, #70677, #57843, .T. ) ;
#32154 = CARTESIAN_POINT ( 'NONE',  ( 4.190625000614518925, -3.027376345333614438, 5.243569643749998122 ) ) ;
#32155 = CARTESIAN_POINT ( 'NONE',  ( 20.03437500061451715, -2.746126346562642428, -4.756430356249999214 ) ) ;
#32156 = CARTESIAN_POINT ( 'NONE',  ( 23.99062500061451786, -3.027376345333614438, 5.243569643749998122 ) ) ;
#32157 = CARTESIAN_POINT ( 'NONE',  ( 17.80312500061451786, -4.541064518000417216, -2.621784821875001281 ) ) ;
#32158 = CARTESIAN_POINT ( 'NONE',  ( 14.63437500061451679, -4.541064518000419881, 2.621784821874995952 ) ) ;
#32159 = CYLINDRICAL_SURFACE ( 'NONE', #72581, 4.000000000000000000 ) ;
#32160 = CARTESIAN_POINT ( 'NONE',  ( 28.12500000122902932, 2.886751345948129099, -4.999999999999998224 ) ) ;
#32161 = CARTESIAN_POINT ( 'NONE',  ( 6.909375000614518036, 0.000000000000000000, 5.243569643749999010 ) ) ;
#32162 = CARTESIAN_POINT ( 'NONE',  ( 16.92187500061451999, -6.054752690667223547, -1.112240025338166033E-15 ) ) ;
#32163 = DIRECTION ( 'NONE',  ( -0.000000000000000000, -1.000000000000000000, -0.000000000000000000 ) ) ;
#32164 = CARTESIAN_POINT ( 'NONE',  ( 24.82499999999999929, 6.123233995736764310E-16, -4.999999999999998224 ) ) ;
#32165 = CARTESIAN_POINT ( 'NONE',  ( 16.80000000122903359, -2.886751345948159742, -4.999999999999942268 ) ) ;
#32166 = CARTESIAN_POINT ( 'NONE',  ( 25.05937500061451573, -4.541064518000417216, -2.621784821875001281 ) ) ;
#32167 = CARTESIAN_POINT ( 'NONE',  ( 16.28437500061452070, 4.541064518000418104, 2.621784821874999949 ) ) ;
#32168 = CARTESIAN_POINT ( 'NONE',  ( -3.756430356250001434, 14.36562499938548143, 32.16877607737301048 ) ) ;
#32169 = CARTESIAN_POINT ( 'NONE',  ( 10.08749999999999858, 5.773502691896255534, 3.535250795749688401E-16 ) ) ;
#32170 = CARTESIAN_POINT ( 'NONE',  ( 8.925000000000002487, -4.330127018922194537, 2.499999999999995559 ) ) ;
#32171 = CARTESIAN_POINT ( 'NONE',  ( 9.234375000614514661, -2.746126346562642428, -4.756430356249999214 ) ) ;
#32172 = CARTESIAN_POINT ( 'NONE',  ( 20.57812500061451644, 6.421520780324663323E-16, -5.243569643749999010 ) ) ;
#32173 = CARTESIAN_POINT ( 'NONE',  ( 8.250000000000000000, 4.330127018922192761, -2.499999999999997780 ) ) ;
#32174 = CARTESIAN_POINT ( 'NONE',  ( 3.253125000614518036, 0.000000000000000000, 5.243569643749999010 ) ) ;
#32175 = CARTESIAN_POINT ( 'NONE',  ( 19.83750000000000213, -2.886751345948125991, -5.000000000000000000 ) ) ;
#32176 = CARTESIAN_POINT ( 'NONE',  ( 18.14062500061451644, -3.027376345333614438, 5.243569643749998122 ) ) ;
#32177 = CARTESIAN_POINT ( 'NONE',  ( 45.00000000000000000, -6.363961030678871644, 6.363961030678982667 ) ) ;
#32178 = AXIS2_PLACEMENT_3D ( 'NONE', #68148, #549, #38983 ) ;
#32179 = CARTESIAN_POINT ( 'NONE',  ( 24.22500000122903430, 2.886751345948126879, 4.999999999999999112 ) ) ;
#32180 = CARTESIAN_POINT ( 'NONE',  ( 14.96250000000000036, 2.886751345948129099, -4.999999999999997335 ) ) ;
#32181 = CARTESIAN_POINT ( 'NONE',  ( 28.65937500061451715, -4.541064518000417216, -2.621784821875001281 ) ) ;
#32182 = ORIENTED_EDGE ( 'NONE', *, *, #67378, .F. ) ;
#32183 = CARTESIAN_POINT ( 'NONE',  ( 17.46562500061451217, 3.027376345333613106, -5.243569643749998122 ) ) ;
#32184 = CARTESIAN_POINT ( 'NONE',  ( 24.44062500061451715, -3.027376345333614438, 5.243569643749998122 ) ) ;
#32185 = CARTESIAN_POINT ( 'NONE',  ( 24.68437500061451573, 6.421520780324663323E-16, -5.243569643749999010 ) ) ;
#32186 = CARTESIAN_POINT ( 'NONE',  ( 9.037499999999999645, -2.886751345948125991, -5.000000000000000000 ) ) ;
#32187 = CARTESIAN_POINT ( 'NONE',  ( 11.01562500061451821, -6.054752690667223547, -1.112240025338166033E-15 ) ) ;
#32188 = CARTESIAN_POINT ( 'NONE',  ( 27.51562500061451644, 3.027376345333611329, 5.243569643749999010 ) ) ;
#32189 = CARTESIAN_POINT ( 'NONE',  ( 18.15937500061451715, 0.000000000000000000, 5.243569643749999010 ) ) ;
#32190 = CARTESIAN_POINT ( 'NONE',  ( 19.39687500061451786, 6.054752690667223547, 3.707466751127219781E-16 ) ) ;
#32191 = CARTESIAN_POINT ( 'NONE',  ( 3.041898612738912711, -3.968258880967949320, 3.108631698898131734 ) ) ;
#32192 = CARTESIAN_POINT ( 'NONE',  ( -4.243569643749997233, 10.89687500061451786, 32.45002607614398471 ) ) ;
#32193 = CARTESIAN_POINT ( 'NONE',  ( 22.87500000122903288, 2.886751345948126879, 4.999999999999999112 ) ) ;
#32194 = CARTESIAN_POINT ( 'NONE',  ( 17.59687500061451715, 5.492252693125287522, 3.363034840372157021E-16 ) ) ;
#32195 = CARTESIAN_POINT ( 'NONE',  ( 13.82812500061451466, 6.421520780324663323E-16, -5.243569643749999010 ) ) ;
#32196 = CARTESIAN_POINT ( 'NONE',  ( 7.996875000614519280, -3.027376345333610441, -5.243569643749999898 ) ) ;
#32197 = CARTESIAN_POINT ( 'NONE',  ( 7.171875000614517326, 3.027376345333613106, -5.243569643749998122 ) ) ;
#32198 = ORIENTED_EDGE ( 'NONE', *, *, #33236, .T. ) ;
#32199 = CARTESIAN_POINT ( 'NONE',  ( 28.17187500061451644, -6.054752690667223547, -1.112240025338166033E-15 ) ) ;
#32200 = CARTESIAN_POINT ( 'NONE',  ( 19.86562500061451786, 3.027376345333611329, 5.243569643749999010 ) ) ;
#32201 = CARTESIAN_POINT ( 'NONE',  ( 23.97187500061451360, 3.027376345333611329, 5.243569643749999010 ) ) ;
#32202 = CARTESIAN_POINT ( 'NONE',  ( 20.01562500061451644, -6.054752690667223547, -1.112240025338166033E-15 ) ) ;
#32203 = CARTESIAN_POINT ( 'NONE',  ( 2.000000000000001332, 11.60000000000000142, 33.46410161513774995 ) ) ;
#32204 = CARTESIAN_POINT ( 'NONE',  ( 25.97812500061451502, 6.421520780324663323E-16, -5.243569643749999010 ) ) ;
#32205 = CARTESIAN_POINT ( 'NONE',  ( 8.175000001229031810, -5.773502691896255534, -1.060575238724906372E-15 ) ) ;
#32206 = ORIENTED_EDGE ( 'NONE', *, *, #60575, .T. ) ;
#32207 = DIRECTION ( 'NONE',  ( 0.000000000000000000, 0.000000000000000000, 1.000000000000000000 ) ) ;
#32208 = CARTESIAN_POINT ( 'NONE',  ( -3.999999999999999112, 15.94999999999999929, -30.00000000000000000 ) ) ;
#32209 = CARTESIAN_POINT ( 'NONE',  ( 23.28750000122903430, 4.330127018922191873, 2.499999999999999556 ) ) ;
#32210 = CARTESIAN_POINT ( 'NONE',  ( -3.756430356249999214, 15.64062499938548179, 27.83122392262697531 ) ) ;
#32211 = CARTESIAN_POINT ( 'NONE',  ( 3.984375000614517326, 6.421520780324663323E-16, -5.243569643749999010 ) ) ;
#32212 = CARTESIAN_POINT ( 'NONE',  ( 12.71250000000000036, 2.886751345948062486, -5.000000000000113687 ) ) ;
#32213 = CARTESIAN_POINT ( 'NONE',  ( 13.67812500061451786, -4.541064518000419881, 2.621784821874995952 ) ) ;
#32214 = CARTESIAN_POINT ( 'NONE',  ( 9.121875000614517504, 3.027376345333611329, 5.243569643749999010 ) ) ;
#32215 = CARTESIAN_POINT ( 'NONE',  ( 26.81250000122903288, 4.330127018922192761, -2.499999999999997780 ) ) ;
#32216 = CARTESIAN_POINT ( 'NONE',  ( 14.52187500061451786, 3.027376345333611329, 5.243569643749999010 ) ) ;
#32217 = CARTESIAN_POINT ( 'NONE',  ( 5.034375000614519813, 4.541064518000418104, 2.621784821874999949 ) ) ;
#32218 = FACE_OUTER_BOUND ( 'NONE', #59944, .T. ) ;
#32219 = CARTESIAN_POINT ( 'NONE',  ( 4.828125000614518214, 6.421520780324663323E-16, -5.243569643749999010 ) ) ;
#32220 = CARTESIAN_POINT ( 'NONE',  ( 15.10312500061451502, -4.541064518000417216, -2.621784821875001281 ) ) ;
#32221 = ORIENTED_EDGE ( 'NONE', *, *, #39155, .T. ) ;
#32222 = CARTESIAN_POINT ( 'NONE',  ( 11.35312500061451679, 0.000000000000000000, 5.243569643749999010 ) ) ;
#32223 = CARTESIAN_POINT ( 'NONE',  ( 8.128125000614515372, 4.541064518000418104, 2.621784821874999949 ) ) ;
#32224 = CARTESIAN_POINT ( 'NONE',  ( 20.67187500061451289, 2.746126346562645981, -4.756430356249997438 ) ) ;
#32225 = CARTESIAN_POINT ( 'NONE',  ( 9.150000000000002132, 4.330127018922192761, -2.499999999999997780 ) ) ;
#32226 = CARTESIAN_POINT ( 'NONE',  ( 4.312500001229034652, 4.330127018922192761, -2.499999999999997780 ) ) ;
#32227 = CARTESIAN_POINT ( 'NONE',  ( 18.30000000000000071, 0.000000000000000000, 4.999999999999998224 ) ) ;
#32228 = CARTESIAN_POINT ( 'NONE',  ( 17.29687500061451999, -3.027376345333614438, 5.243569643749998122 ) ) ;
#32229 = CARTESIAN_POINT ( 'NONE',  ( 14.70000000122903394, 5.773502691896255534, 3.535250795749688894E-16 ) ) ;
#32230 = CARTESIAN_POINT ( 'NONE',  ( 23.32499999999999929, -4.330127018922194537, 2.499999999999995559 ) ) ;
#32231 = CARTESIAN_POINT ( 'NONE',  ( 9.001249775931846008E-16, 16.76562500061451999, -25.09994784771203058 ) ) ;
#32232 = CARTESIAN_POINT ( 'NONE',  ( 20.73750000000000071, -2.886751345948098013, -5.000000000000047073 ) ) ;
#32233 = CARTESIAN_POINT ( 'NONE',  ( 45.00000000000000000, 0.000000000000000000, 0.000000000000000000 ) ) ;
#32234 = CARTESIAN_POINT ( 'NONE',  ( 29.24062500061451431, 6.054752690667223547, 3.707466751127219781E-16 ) ) ;
#32235 = FACE_OUTER_BOUND ( 'NONE', #19310, .T. ) ;
#32236 = CARTESIAN_POINT ( 'NONE',  ( 29.67187500061451644, 3.027376345333613106, -5.243569643749998122 ) ) ;
#32237 = CARTESIAN_POINT ( 'NONE',  ( 16.92187500061451999, -6.054752690667223547, -1.112240025338166033E-15 ) ) ;
#32238 = CARTESIAN_POINT ( 'NONE',  ( 26.58750000000000213, -2.886751345948125991, -5.000000000000000000 ) ) ;
#32239 = EDGE_CURVE ( 'NONE', #13801, #58433, #40883, .T. ) ;
#32240 = CARTESIAN_POINT ( 'NONE',  ( 11.01562500061451821, -6.054752690667223547, -1.112240025338166033E-15 ) ) ;
#32241 = CARTESIAN_POINT ( 'NONE',  ( 26.78437500061451715, -2.746126346562642428, -4.756430356249999214 ) ) ;
#32242 = CARTESIAN_POINT ( 'NONE',  ( 20.97187500061451715, -6.054752690667223547, -1.112240025338166033E-15 ) ) ;
#32243 = CARTESIAN_POINT ( 'NONE',  ( 14.25937500061451857, 2.746126346562645981, -4.756430356249997438 ) ) ;
#32244 = CARTESIAN_POINT ( 'NONE',  ( 6.478125000614516793, -4.541064518000419881, 2.621784821874995952 ) ) ;
#32245 = CARTESIAN_POINT ( 'NONE',  ( 14.07187500061451679, 3.027376345333611329, 5.243569643749999010 ) ) ;
#32246 = VERTEX_POINT ( 'NONE', #6532 ) ;
#32247 = CARTESIAN_POINT ( 'NONE',  ( 24.38437500061451502, 4.541064518000418104, 2.621784821874999949 ) ) ;
#32248 = CARTESIAN_POINT ( 'NONE',  ( 3.964577175323932057, 3.046748717458610312, -29.45119415667360840 ) ) ;
#32249 = CARTESIAN_POINT ( 'NONE',  ( 24.67500000000000071, -4.330127018922194537, 2.499999999999995559 ) ) ;
#32250 = CARTESIAN_POINT ( 'NONE',  ( 5.400000000000002132, -4.330127018922190985, -2.500000000000001332 ) ) ;
#32251 = CARTESIAN_POINT ( 'NONE',  ( 17.92500000122903359, 2.886751345948126879, 4.999999999999999112 ) ) ;
#32252 = CARTESIAN_POINT ( 'NONE',  ( 45.00000000000000000, -9.000000000000000000, 0.000000000000000000 ) ) ;
#32253 = CARTESIAN_POINT ( 'NONE',  ( 7.846875000614515372, -4.119189519843965641, -2.378215178125001383 ) ) ;
#32254 = ORIENTED_EDGE ( 'NONE', *, *, #18853, .T. ) ;
#32255 = CARTESIAN_POINT ( 'NONE',  ( 14.73749999999999893, -2.886751345948129988, 4.999999999999997335 ) ) ;
#32256 = CARTESIAN_POINT ( 'NONE',  ( 15.97499999999999964, 4.330127018922191873, 2.499999999999999556 ) ) ;
#32257 = CARTESIAN_POINT ( 'NONE',  ( 12.32812500061451821, -4.541064518000419881, 2.621784821874995952 ) ) ;
#32258 =( BOUNDED_CURVE ( )  B_SPLINE_CURVE ( 2, ( #47254, #69787, #19154, #72890, #28190, #62160, #22271, #11557, #61788 ),
 .UNSPECIFIED., .F., .F. ) 
 B_SPLINE_CURVE_WITH_KNOTS ( ( 3, 2, 2, 2, 3 ),
 ( 0.6847826086956522174, 0.6884057971014492239, 0.6956521739130434590, 0.7028985507246376940, 0.7065217391304348116 ),
 .UNSPECIFIED. ) 
 CURVE ( )  GEOMETRIC_REPRESENTATION_ITEM ( )  RATIONAL_B_SPLINE_CURVE ( ( 0.9330127018922192983, 0.9330127018922202975, 1.000000000000000000, 0.8660254037844387076, 1.000000000000000000, 0.8660254037844387076, 1.000000000000000000, 0.9330127018922194093, 0.9330127018922194093 ) ) 
 REPRESENTATION_ITEM ( '' )  );
#32259 = ORIENTED_EDGE ( 'NONE', *, *, #59745, .T. ) ;
#32260 = CARTESIAN_POINT ( 'NONE',  ( -2.000000000000000000, 16.88750000122903572, -33.46410161513775705 ) ) ;
#32261 = CARTESIAN_POINT ( 'NONE',  ( 4.243569643749999898, 16.44687500061451857, -27.54997392385601529 ) ) ;
#32262 = CARTESIAN_POINT ( 'NONE',  ( 29.66250000122903074, 0.000000000000000000, 4.999999999999998224 ) ) ;
#32263 = CARTESIAN_POINT ( 'NONE',  ( -1.878215178124999163, 13.69062499938548427, 26.74683588394047007 ) ) ;
#32264 = CARTESIAN_POINT ( 'NONE',  ( 10.35000000000000142, -4.330127018922190985, -2.500000000000001332 ) ) ;
#32265 = CARTESIAN_POINT ( 'NONE',  ( -2.498395430326213790E-14, 18.46250000000000213, 26.00000000000000000 ) ) ;
#32266 = ORIENTED_EDGE ( 'NONE', *, *, #71724, .F. ) ;
#32267 = CARTESIAN_POINT ( 'NONE',  ( -2.121784821874996840, 13.12812500061451715, 33.67503911421598417 ) ) ;
#32268 = CARTESIAN_POINT ( 'NONE',  ( 23.35312500061451857, 4.541064518000418104, -2.621784821874998173 ) ) ;
#32269 = CARTESIAN_POINT ( 'NONE',  ( 7.285825576177820915E-16, 10.00000000000000000, 36.00000000000000000 ) ) ;
#32270 = CARTESIAN_POINT ( 'NONE',  ( 45.00000000000000000, 0.000000000000000000, 0.000000000000000000 ) ) ;
#32271 = CARTESIAN_POINT ( 'NONE',  ( 21.04687500061451644, -3.027376345333610441, -5.243569643749999898 ) ) ;
#32272 = CARTESIAN_POINT ( 'NONE',  ( 20.05312500061451431, -4.541064518000417216, -2.621784821875001281 ) ) ;
#32273 = CARTESIAN_POINT ( 'NONE',  ( -2.121784821874996840, 14.47812500061459318, -26.32496088578401583 ) ) ;
#32274 = CARTESIAN_POINT ( 'NONE',  ( 23.32500000122903572, 2.886751345948126879, 4.999999999999999112 ) ) ;
#32275 = CARTESIAN_POINT ( 'NONE',  ( 4.078125000614517326, 4.541064518000418104, 2.621784821874999949 ) ) ;
#32276 = CARTESIAN_POINT ( 'NONE',  ( 23.52187500061451786, 2.746126346562643317, 4.756430356249998326 ) ) ;
#32277 = CARTESIAN_POINT ( 'NONE',  ( 21.81562500061451004, -6.054752690667223547, -1.112240025338166033E-15 ) ) ;
#32278 = FACE_OUTER_BOUND ( 'NONE', #20044, .T. ) ;
#32279 = CARTESIAN_POINT ( 'NONE',  ( -1.878215178125001827, 19.69062499938548072, 33.25316411605952283 ) ) ;
#32280 = CARTESIAN_POINT ( 'NONE',  ( 16.13437500061451502, 6.421520780324663323E-16, -5.243569643749999010 ) ) ;
#32281 = CARTESIAN_POINT ( 'NONE',  ( 14.14687500061451786, -3.027376345333614438, 5.243569643749998122 ) ) ;
#32282 = CARTESIAN_POINT ( 'NONE',  ( 23.52187500061451786, 3.027376345333611329, 5.243569643749999010 ) ) ;
#32283 = CARTESIAN_POINT ( 'NONE',  ( -4.243569643749998122, 12.69687500061451857, 32.45002607614398471 ) ) ;
#32284 = CARTESIAN_POINT ( 'NONE',  ( 4.003125000614518925, 4.541064518000418104, -2.621784821874998173 ) ) ;
#32285 = CARTESIAN_POINT ( 'NONE',  ( 25.90312500061451573, -4.541064518000417216, -2.621784821875001281 ) ) ;
#32286 = CARTESIAN_POINT ( 'NONE',  ( 27.02812500061451573, 4.541064518000418104, 2.621784821874999949 ) ) ;
#32287 = CARTESIAN_POINT ( 'NONE',  ( 17.41875000122903216, 2.886751345948182834, 4.999999999999902300 ) ) ;
#32288 = CARTESIAN_POINT ( 'NONE',  ( -3.999999999999999112, 19.09999999999999787, 30.00000000000000000 ) ) ;
#32289 = CARTESIAN_POINT ( 'NONE',  ( 7.359375000614516438, 0.000000000000000000, 5.243569643749999010 ) ) ;
#32290 = APPLICATION_PROTOCOL_DEFINITION ( 'draft international standard', 'automotive_design', 1998, #38961 ) ;
#32291 = CARTESIAN_POINT ( 'NONE',  ( 15.37500000122903465, -5.773502691896255534, -1.060575238724906372E-15 ) ) ;
#32292 = CARTESIAN_POINT ( 'NONE',  ( 9.637500001229033941, 6.123233995736764310E-16, -4.999999999999998224 ) ) ;
#32293 = CARTESIAN_POINT ( 'NONE',  ( 29.40000000122903145, -2.886751345948125991, -5.000000000000000000 ) ) ;
#32294 = CARTESIAN_POINT ( 'NONE',  ( -4.000000000000000000, 15.81874999877096499, 30.00000000000000000 ) ) ;
#32295 = CARTESIAN_POINT ( 'NONE',  ( 18.01875000122903359, -5.773502691896255534, -1.060575238724906372E-15 ) ) ;
#32296 = CARTESIAN_POINT ( 'NONE',  ( 15.15937500061451715, -4.541064518000417216, -2.621784821875001281 ) ) ;
#32297 = CARTESIAN_POINT ( 'NONE',  ( 45.00000000000000000, 0.000000000000000000, 0.000000000000000000 ) ) ;
#32298 = EDGE_LOOP ( 'NONE', ( #60979, #45524, #38900, #16708 ) ) ;
#32299 = CARTESIAN_POINT ( 'NONE',  ( 19.86562500061451786, 3.027376345333611329, 5.243569643749999010 ) ) ;
#32300 = CARTESIAN_POINT ( 'NONE',  ( 6.178125000614518747, 6.421520780324663323E-16, -5.243569643749999010 ) ) ;
#32301 = CARTESIAN_POINT ( 'NONE',  ( 24.08437500061451786, -4.541064518000419881, 2.621784821874995952 ) ) ;
#32302 = CARTESIAN_POINT ( 'NONE',  ( 8.353125000614518569, -4.541064518000417216, -2.621784821875001281 ) ) ;
#32303 = CARTESIAN_POINT ( 'NONE',  ( -3.999999999999999112, 16.23124999877096641, 27.69059892324149530 ) ) ;
#32304 = CARTESIAN_POINT ( 'NONE',  ( 7.125000001229033764, 2.886751345948126879, 4.999999999999999112 ) ) ;
#32305 = EDGE_CURVE ( 'NONE', #18562, #15973, #62315, .T. ) ;
#32306 = CARTESIAN_POINT ( 'NONE',  ( 22.67812500061451431, -4.541064518000419881, 2.621784821874995952 ) ) ;
#32307 = CARTESIAN_POINT ( 'NONE',  ( 1.999999999999998668, 18.16250000122903074, -33.46410161513775705 ) ) ;
#32308 = CARTESIAN_POINT ( 'NONE',  ( 11.17500000122903536, 2.886751345948126879, 4.999999999999999112 ) ) ;
#32309 = CARTESIAN_POINT ( 'NONE',  ( 19.04062500061451146, -3.027376345333614438, 5.243569643749998122 ) ) ;
#32310 = CARTESIAN_POINT ( 'NONE',  ( 15.02812500061451750, -4.541064518000419881, 2.621784821874995952 ) ) ;
#32311 = CARTESIAN_POINT ( 'NONE',  ( 27.64687500061452141, -2.746126346562646425, 4.756430356249996549 ) ) ;
#32312 = CARTESIAN_POINT ( 'NONE',  ( 16.87500000000000000, 4.330127018922191873, 2.499999999999999556 ) ) ;
#32313 = CARTESIAN_POINT ( 'NONE',  ( 11.10000000122903252, 5.773502691896255534, 3.535250795749688894E-16 ) ) ;
#32314 = CARTESIAN_POINT ( 'NONE',  ( 8.090625000614515727, 6.054752690667223547, 3.707466751127219781E-16 ) ) ;
#32315 = CARTESIAN_POINT ( 'NONE',  ( 12.14062500061451821, 6.054752690667223547, 3.707466751127219781E-16 ) ) ;
#32316 = CARTESIAN_POINT ( 'NONE',  ( 19.80000000122903359, -2.886751345948129988, 4.999999999999997335 ) ) ;
#32317 = CARTESIAN_POINT ( 'NONE',  ( 19.80937500061451573, 4.541064518000418104, -2.621784821874998173 ) ) ;
#32318 = CARTESIAN_POINT ( 'NONE',  ( 4.629056002857023344, -1.889931353889065413, 4.891133006415133266 ) ) ;
#32319 = EDGE_CURVE ( 'NONE', #61054, #23329, #65031, .T. ) ;
#32320 = CARTESIAN_POINT ( 'NONE',  ( 6.487500001229034474, 6.123233995736764310E-16, -4.999999999999998224 ) ) ;
#32321 = CARTESIAN_POINT ( 'NONE',  ( 5.221875000614519813, -6.054752690667223547, -1.112240025338166033E-15 ) ) ;
#32322 = CARTESIAN_POINT ( 'NONE',  ( 22.05937500061451573, 4.541064518000418104, -2.621784821874998173 ) ) ;
#32323 = CARTESIAN_POINT ( 'NONE',  ( 18.44062500061451715, 6.054752690667223547, 3.707466751127219781E-16 ) ) ;
#32324 = CARTESIAN_POINT ( 'NONE',  ( 23.18437500061451573, -4.541064518000419881, 2.621784821874995952 ) ) ;
#32325 = CARTESIAN_POINT ( 'NONE',  ( -1.878215178125001827, 20.25312499938548072, 33.25316411605952283 ) ) ;
#32326 = CARTESIAN_POINT ( 'NONE',  ( -4.000000000000000888, 14.56250000000000000, 32.30940107675850470 ) ) ;
#32327 = CARTESIAN_POINT ( 'NONE',  ( 29.82187500061451502, 3.027376345333611329, 5.243569643749999010 ) ) ;
#32328 = CARTESIAN_POINT ( 'NONE',  ( 21.04687500061451644, 4.119189519843966529, -2.378215178124998275 ) ) ;
#32329 = CARTESIAN_POINT ( 'NONE',  ( 14.01562500061451644, 3.027376345333611329, 5.243569643749999010 ) ) ;
#32330 = CARTESIAN_POINT ( 'NONE',  ( 12.38437500061451857, -4.541064518000419881, 2.621784821874995952 ) ) ;
#32331 = ORIENTED_EDGE ( 'NONE', *, *, #45231, .F. ) ;
#32332 = CARTESIAN_POINT ( 'NONE',  ( 23.47499999999999787, 6.123233995736764310E-16, -4.999999999999998224 ) ) ;
#32333 = CARTESIAN_POINT ( 'NONE',  ( 23.84062500061451928, 6.054752690667223547, 3.707466751127219781E-16 ) ) ;
#32334 = CARTESIAN_POINT ( 'NONE',  ( 11.55000000000000071, 0.000000000000000000, 4.999999999999998224 ) ) ;
#32335 = CARTESIAN_POINT ( 'NONE',  ( 30.00000000000000000, 0.000000000000000000, 4.999999999999998224 ) ) ;
#32336 = CARTESIAN_POINT ( 'NONE',  ( 14.02499999999999858, 6.123233995736764310E-16, -4.999999999999998224 ) ) ;
#32337 = CARTESIAN_POINT ( 'NONE',  ( 23.73750000122903359, 4.330127018922191873, 2.499999999999999556 ) ) ;
#32338 = CARTESIAN_POINT ( 'NONE',  ( 18.74062500061451431, -3.027376345333610441, -5.243569643749999898 ) ) ;
#32339 = VERTEX_POINT ( 'NONE', #6894 ) ;
#32340 = CARTESIAN_POINT ( 'NONE',  ( 21.60000000000000142, -4.330127018922190985, -2.500000000000001332 ) ) ;
#32341 = CARTESIAN_POINT ( 'NONE',  ( 23.37187500061451573, 3.027376345333613106, -5.243569643749998122 ) ) ;
#32342 = ORIENTED_EDGE ( 'NONE', *, *, #28737, .T. ) ;
#32343 = CARTESIAN_POINT ( 'NONE',  ( 18.97499999999999787, 6.123233995736764310E-16, -4.999999999999998224 ) ) ;
#32344 = CARTESIAN_POINT ( 'NONE',  ( 10.60312500061451679, -4.541064518000417216, -2.621784821875001281 ) ) ;
#32345 = CARTESIAN_POINT ( 'NONE',  ( 4.415625000614518569, 3.027376345333613106, -5.243569643749998122 ) ) ;
#32346 = CARTESIAN_POINT ( 'NONE',  ( 14.78437500061451537, 5.492252693125287522, 3.363034840372157021E-16 ) ) ;
#32347 = CARTESIAN_POINT ( 'NONE',  ( 26.46562500061451573, 3.027376345333613106, -5.243569643749998122 ) ) ;
#32348 = CARTESIAN_POINT ( 'NONE',  ( 16.27499999999999858, 6.123233995736764310E-16, -4.999999999999998224 ) ) ;
#32349 = CARTESIAN_POINT ( 'NONE',  ( 23.62500000000000000, 4.330127018922191873, 2.499999999999999556 ) ) ;
#32350 = CARTESIAN_POINT ( 'NONE',  ( 30.00000000000000000, 6.123233995736764310E-16, -4.999999999999998224 ) ) ;
#32351 = CARTESIAN_POINT ( 'NONE',  ( 7.396875000614519635, -3.027376345333614438, 5.243569643749998122 ) ) ;
#32352 = CARTESIAN_POINT ( 'NONE',  ( 18.15937500061451715, 0.000000000000000000, 5.243569643749999010 ) ) ;
#32353 = CARTESIAN_POINT ( 'NONE',  ( 28.73437500061451644, 6.421520780324663323E-16, -5.243569643749999010 ) ) ;
#32354 = ORIENTED_EDGE ( 'NONE', *, *, #51501, .T. ) ;
#32355 = CARTESIAN_POINT ( 'NONE',  ( 27.29062500061451502, -3.027376345333610441, -5.243569643749999898 ) ) ;
#32356 = CARTESIAN_POINT ( 'NONE',  ( 27.49687500061451217, 6.054752690667223547, 3.707466751127219781E-16 ) ) ;
#32357 = CARTESIAN_POINT ( 'NONE',  ( 2.859375000614519546, 0.000000000000000000, 5.243569643749999010 ) ) ;
#32358 = CARTESIAN_POINT ( 'NONE',  ( 13.46249999999999858, -5.773502691896255534, -1.060575238724906372E-15 ) ) ;
#32359 = CARTESIAN_POINT ( 'NONE',  ( 10.11562500061451608, -6.054752690667223547, -1.112240025338166033E-15 ) ) ;
#32360 = CARTESIAN_POINT ( 'NONE',  ( 30.00000000000000000, 0.000000000000000000, 0.000000000000000000 ) ) ;
#32361 = CARTESIAN_POINT ( 'NONE',  ( 5.810221930991193690E-16, 14.35624999877096464, 26.00000000000000000 ) ) ;
#32362 = CARTESIAN_POINT ( 'NONE',  ( 28.60312500061451502, -4.541064518000417216, -2.621784821875001281 ) ) ;
#32363 = CARTESIAN_POINT ( 'NONE',  ( 15.93750000122903110, 6.123233995736764310E-16, -4.999999999999998224 ) ) ;
#32364 = CARTESIAN_POINT ( 'NONE',  ( 15.98437500061451821, -4.119189519843968306, 2.378215178124996054 ) ) ;
#32365 = CARTESIAN_POINT ( 'NONE',  ( 6.028125000614517504, -4.541064518000419881, 2.621784821874995952 ) ) ;
#32366 = CARTESIAN_POINT ( 'NONE',  ( 22.92187500061451644, 3.027376345333613106, -5.243569643749998122 ) ) ;
#32367 = CARTESIAN_POINT ( 'NONE',  ( 4.243569643749999898, 15.99687500061451573, 32.45002607614398471 ) ) ;
#32368 = CARTESIAN_POINT ( 'NONE',  ( 20.74687500061451573, 6.054752690667223547, 3.707466751127219781E-16 ) ) ;
#32369 = CARTESIAN_POINT ( 'NONE',  ( 5.587500000000003020, 5.773502691896255534, 3.535250795749688894E-16 ) ) ;
#32370 = CARTESIAN_POINT ( 'NONE',  ( -3.000416591977282496E-16, 19.74687500061451928, 25.09994784771203058 ) ) ;
#32371 = CARTESIAN_POINT ( 'NONE',  ( 13.04062500061451502, 6.054752690667223547, 3.707466751127219781E-16 ) ) ;
#32372 = CARTESIAN_POINT ( 'NONE',  ( 4.050000001229035362, -2.886751345948129988, 4.999999999999997335 ) ) ;
#32373 = CARTESIAN_POINT ( 'NONE',  ( 6.571875000614517681, -6.054752690667223547, -1.112240025338166033E-15 ) ) ;
#32374 = CARTESIAN_POINT ( 'NONE',  ( 3.913234685210329467, 3.112428286967196200, -4.086165593540687091 ) ) ;
#32375 = CARTESIAN_POINT ( 'NONE',  ( 10.79062500061451679, 6.054752690667223547, 3.707466751127219781E-16 ) ) ;
#32376 = CARTESIAN_POINT ( 'NONE',  ( 15.23437500061451644, 6.421520780324663323E-16, -5.243569643749999010 ) ) ;
#32377 = CARTESIAN_POINT ( 'NONE',  ( 25.68750000000000000, -2.886751345948167735, -4.999999999999927169 ) ) ;
#32378 = CARTESIAN_POINT ( 'NONE',  ( 20.43750000122903643, 6.123233995736764310E-16, -4.999999999999998224 ) ) ;
#32379 = CARTESIAN_POINT ( 'NONE',  ( 7.546875000614517326, -3.027376345333610441, -5.243569643749999898 ) ) ;
#32380 = CARTESIAN_POINT ( 'NONE',  ( 12.96562500061451750, 3.027376345333613106, -5.243569643749998122 ) ) ;
#32381 = CARTESIAN_POINT ( 'NONE',  ( 26.38125000122903430, 4.330127018922191873, 2.499999999999999556 ) ) ;
#32382 = CARTESIAN_POINT ( 'NONE',  ( 21.94687500061451857, -3.027376345333610441, -5.243569643749999898 ) ) ;
#32383 = DIRECTION ( 'NONE',  ( -1.000000000000000000, 0.000000000000000000, 0.000000000000000000 ) ) ;
#32384 = CARTESIAN_POINT ( 'NONE',  ( -3.027546007007307249, 3.984809627175307067, 27.37408915144584398 ) ) ;
#32385 = DIRECTION ( 'NONE',  ( -1.000000000000000000, -0.000000000000000000, -0.000000000000000000 ) ) ;
#32386 = CARTESIAN_POINT ( 'NONE',  ( -2.121784821874996840, 12.73437500061451821, -26.32496088578401583 ) ) ;
#32387 = CARTESIAN_POINT ( 'NONE',  ( 14.58750000122903323, 6.123233995736764310E-16, -4.999999999999998224 ) ) ;
#32388 = EDGE_CURVE ( 'NONE', #38296, #49458, #12179, .T. ) ;
#32389 = CARTESIAN_POINT ( 'NONE',  ( -3.000416591977282496E-16, 15.19062500061451715, -34.90005215228797653 ) ) ;
#32390 = CARTESIAN_POINT ( 'NONE',  ( 18.18750000122903288, 6.123233995736764310E-16, -4.999999999999998224 ) ) ;
#32391 = CARTESIAN_POINT ( 'NONE',  ( 10.56562500061451715, -6.054752690667223547, -1.112240025338166033E-15 ) ) ;
#32392 = VECTOR ( 'NONE', #33410, 1000.000000000000000 ) ;
#32393 = VERTEX_POINT ( 'NONE', #46057 ) ;
#32394 = CARTESIAN_POINT ( 'NONE',  ( 16.27499999999999858, 6.123233995736764310E-16, -4.999999999999998224 ) ) ;
#32395 = DIRECTION ( 'NONE',  ( -1.000000000000000000, -0.000000000000000000, -0.000000000000000000 ) ) ;
#32396 = CARTESIAN_POINT ( 'NONE',  ( 21.59062500061451928, 6.054752690667223547, 3.707466751127219781E-16 ) ) ;
#32397 = CARTESIAN_POINT ( 'NONE',  ( 9.984375000614518214, 4.541064518000418104, 2.621784821874999949 ) ) ;
#32398 = EDGE_CURVE ( 'NONE', #70091, #17423, #46704, .T. ) ;
#32399 = DIRECTION ( 'NONE',  ( -1.000000000000000000, -0.000000000000000000, -0.000000000000000000 ) ) ;
#32400 = CARTESIAN_POINT ( 'NONE',  ( 9.225000001229034297, 2.886751345948129099, -4.999999999999998224 ) ) ;
#32401 = CARTESIAN_POINT ( 'NONE',  ( 19.01250000122903216, -4.330127018922190985, -2.500000000000001332 ) ) ;
#32402 = CARTESIAN_POINT ( 'NONE',  ( 16.07812500061451289, 6.421520780324663323E-16, -5.243569643749999010 ) ) ;
#32403 = EDGE_CURVE ( 'NONE', #43953, #57884, #63399, .T. ) ;
#32404 = CARTESIAN_POINT ( 'NONE',  ( 17.16562500061451502, 3.027376345333611329, 5.243569643749999010 ) ) ;
#32405 = CARTESIAN_POINT ( 'NONE',  ( 25.31250000122903288, -4.330127018922190985, -2.500000000000001332 ) ) ;
#32406 = CIRCLE ( 'NONE', #65397, 5.000000000000000000 ) ;
#32407 = CARTESIAN_POINT ( 'NONE',  ( 29.28750000122903074, -4.330127018922194537, 2.499999999999995559 ) ) ;
#32408 = CARTESIAN_POINT ( 'NONE',  ( 25.87500000000000000, 4.330127018922191873, 2.499999999999999556 ) ) ;
#32409 = CARTESIAN_POINT ( 'NONE',  ( -3.756430356250000102, 13.76562499938548356, 30.00000000000000000 ) ) ;
#32410 = VECTOR ( 'NONE', #70941, 1000.000000000000000 ) ;
#32411 = CARTESIAN_POINT ( 'NONE',  ( 26.74687500061451573, -3.027376345333614438, 5.243569643749998122 ) ) ;
#32412 = CARTESIAN_POINT ( 'NONE',  ( 45.00000000000000000, 0.000000000000000000, 0.000000000000000000 ) ) ;
#32413 = CARTESIAN_POINT ( 'NONE',  ( 11.92500000122903181, 2.886751345948129099, -4.999999999999998224 ) ) ;
#32414 = CARTESIAN_POINT ( 'NONE',  ( 3.000000000000002665, 0.000000000000000000, 4.999999999999998224 ) ) ;
#32415 =( BOUNDED_CURVE ( )  B_SPLINE_CURVE ( 2, ( #39697, #72943, #176, #67412, #17137, #39331, #61845 ),
 .UNSPECIFIED., .F., .F. ) 
 B_SPLINE_CURVE_WITH_KNOTS ( ( 3, 2, 2, 3 ),
 ( 0.2166666666666667296, 0.2194444444444444975, 0.2222222222222222654, 0.2250000000000000611 ),
 .UNSPECIFIED. ) 
 CURVE ( )  GEOMETRIC_REPRESENTATION_ITEM ( )  RATIONAL_B_SPLINE_CURVE ( ( 0.9999999999999973355, 0.8660254037844413721, 1.000000000000000000, 0.8660254037844387076, 1.000000000000000000, 0.8660254037844360431, 1.000000000000002665 ) ) 
 REPRESENTATION_ITEM ( '' )  );
#32416 = CARTESIAN_POINT ( 'NONE',  ( -1.999999999999999112, 18.44374999877096499, 26.53589838486224650 ) ) ;
#32417 = CARTESIAN_POINT ( 'NONE',  ( 6.384375000614516793, 4.541064518000418104, 2.621784821874999949 ) ) ;
#32418 = CARTESIAN_POINT ( 'NONE',  ( 26.31562500061451715, -6.054752690667223547, -1.112240025338166033E-15 ) ) ;
#32419 = CARTESIAN_POINT ( 'NONE',  ( 4.869423765992945796, -1.135214599616954256, -5.119209941160161037 ) ) ;
#32420 = CARTESIAN_POINT ( 'NONE',  ( 4.000000000000000000, 10.40000000122903323, 32.30940107675849760 ) ) ;
#32421 = CARTESIAN_POINT ( 'NONE',  ( 27.35625000122903216, 0.000000000000000000, 4.999999999999998224 ) ) ;
#32422 = CARTESIAN_POINT ( 'NONE',  ( 5.221875000614519813, -6.054752690667223547, -1.112240025338166033E-15 ) ) ;
#32423 = CARTESIAN_POINT ( 'NONE',  ( 9.721875000614517148, -6.054752690667223547, -1.112240025338166033E-15 ) ) ;
#32424 = CARTESIAN_POINT ( 'NONE',  ( 29.44687500061451857, -3.027376345333614438, 5.243569643749998122 ) ) ;
#32425 = EDGE_CURVE ( 'NONE', #13717, #57266, #4646, .T. ) ;
#32426 = CARTESIAN_POINT ( 'NONE',  ( -3.000416591977282496E-16, 11.59062500061459389, 25.09994784771203058 ) ) ;
#32427 = CARTESIAN_POINT ( 'NONE',  ( 21.26249999999999574, 2.886751345948129099, -4.999999999999998224 ) ) ;
#32428 = CARTESIAN_POINT ( 'NONE',  ( 29.13749999999999929, -2.886751345948129988, 4.999999999999997335 ) ) ;
#32429 = CARTESIAN_POINT ( 'NONE',  ( 5.137500000000000178, 5.773502691896255534, 3.535250795749688894E-16 ) ) ;
#32430 = ORIENTED_EDGE ( 'NONE', *, *, #4064, .F. ) ;
#32431 = CARTESIAN_POINT ( 'NONE',  ( 17.91562500061451502, 3.027376345333613106, -5.243569643749998122 ) ) ;
#32432 = CARTESIAN_POINT ( 'NONE',  ( 10.90312500061451928, 0.000000000000000000, 5.243569643749999010 ) ) ;
#32433 = CARTESIAN_POINT ( 'NONE',  ( 21.19687500061451502, 0.000000000000000000, 4.756430356249998326 ) ) ;
#32434 = CARTESIAN_POINT ( 'NONE',  ( 7.209375000614519635, 4.541064518000418104, -2.621784821874998173 ) ) ;
#32435 = CARTESIAN_POINT ( 'NONE',  ( 23.13749999999999929, 5.773502691896255534, 3.535250795749688894E-16 ) ) ;
#32436 = CARTESIAN_POINT ( 'NONE',  ( 19.68750000122903288, 4.330127018922191873, 2.499999999999999556 ) ) ;
#32437 = VECTOR ( 'NONE', #59983, 1000.000000000000000 ) ;
#32438 = CARTESIAN_POINT ( 'NONE',  ( 15.63749999999999751, -2.886751345948063374, 5.000000000000112799 ) ) ;
#32439 = CARTESIAN_POINT ( 'NONE',  ( 8.184375000614515727, 4.541064518000418104, 2.621784821874999949 ) ) ;
#32440 = CARTESIAN_POINT ( 'NONE',  ( 12.94687500061451857, -3.027376345333610441, -5.243569643749999898 ) ) ;
#32441 = CARTESIAN_POINT ( 'NONE',  ( 24.30937500061451573, 4.541064518000418104, -2.621784821874998173 ) ) ;
#32442 = CARTESIAN_POINT ( 'NONE',  ( 0.000000000000000000, 20.00000000000000000, 30.00000000000000000 ) ) ;
#32443 = ORIENTED_EDGE ( 'NONE', *, *, #19369, .T. ) ;
#32444 = CARTESIAN_POINT ( 'NONE',  ( 12.26249999999999929, 2.886751345948129099, -4.999999999999998224 ) ) ;
#32445 = CARTESIAN_POINT ( 'NONE',  ( 17.93437500061451928, 6.421520780324663323E-16, -5.243569643749999010 ) ) ;
#32446 = AXIS2_PLACEMENT_3D ( 'NONE', #36770, #59287, #2791 ) ;
#32447 = CARTESIAN_POINT ( 'NONE',  ( 9.271875000614516082, -6.054752690667223547, -1.112240025338166033E-15 ) ) ;
#32448 = CARTESIAN_POINT ( 'NONE',  ( 3.756430356249998770, 15.75312499938548427, 32.16877607737302469 ) ) ;
#32449 = CARTESIAN_POINT ( 'NONE',  ( 21.26249999999999574, 2.886751345948129099, -4.999999999999998224 ) ) ;
#32450 = CARTESIAN_POINT ( 'NONE',  ( 2.000000000000000444, 14.37500000000000000, 26.53589838486224650 ) ) ;
#32451 = CARTESIAN_POINT ( 'NONE',  ( -1.071796769724492115, 17.31740381056766864, 34.00000000000000000 ) ) ;
#32452 = CARTESIAN_POINT ( 'NONE',  ( 21.98437500061451644, 5.824947211148865298E-16, -4.756430356249998326 ) ) ;
#32453 = CARTESIAN_POINT ( 'NONE',  ( 12.17812500061451608, 4.541064518000418104, 2.621784821874999949 ) ) ;
#32454 = CARTESIAN_POINT ( 'NONE',  ( 28.54687500061451644, -3.027376345333614438, 5.243569643749998122 ) ) ;
#32455 = CARTESIAN_POINT ( 'NONE',  ( 6.825000001229035718, -5.773502691896255534, -1.060575238724906372E-15 ) ) ;
#32456 = CARTESIAN_POINT ( 'NONE',  ( 28.58437500061451786, -4.541064518000419881, 2.621784821874995952 ) ) ;
#32457 = CARTESIAN_POINT ( 'NONE',  ( 11.17500000000000071, -4.330127018922194537, 2.499999999999995559 ) ) ;
#32458 = CARTESIAN_POINT ( 'NONE',  ( -1.999999999999997113, 17.93750000122903288, 33.46410161513775705 ) ) ;
#32459 = CARTESIAN_POINT ( 'NONE',  ( 11.66250000122903430, 0.000000000000000000, 4.999999999999998224 ) ) ;
#32460 = VECTOR ( 'NONE', #65613, 1000.000000000000000 ) ;
#32461 = CARTESIAN_POINT ( 'NONE',  ( 22.58437500061451431, 4.541064518000418104, 2.621784821874999949 ) ) ;
#32462 = CARTESIAN_POINT ( 'NONE',  ( 17.78437500061451715, -4.541064518000419881, 2.621784821874995952 ) ) ;
#32463 = CARTESIAN_POINT ( 'NONE',  ( -5.810221930991193690E-16, 12.23750000000000071, 26.00000000000000355 ) ) ;
#32464 = ORIENTED_EDGE ( 'NONE', *, *, #47732, .F. ) ;
#32465 = CARTESIAN_POINT ( 'NONE',  ( 16.07812500061451289, 6.421520780324663323E-16, -5.243569643749999010 ) ) ;
#32466 = VECTOR ( 'NONE', #54505, 1000.000000000000000 ) ;
#32467 = CARTESIAN_POINT ( 'NONE',  ( 28.98750000122903359, 6.123233995736764310E-16, -4.999999999999998224 ) ) ;
#32468 = CARTESIAN_POINT ( 'NONE',  ( 18.04687500061451999, 6.054752690667223547, 3.707466751127219781E-16 ) ) ;
#32469 = CARTESIAN_POINT ( 'NONE',  ( 5.375648687660713243, 8.434199909737650103, -27.30640515792645928 ) ) ;
#32470 = CARTESIAN_POINT ( 'NONE',  ( 19.90312500061451573, 0.000000000000000000, 5.243569643749999010 ) ) ;
#32471 = LINE ( 'NONE', #55004, #18529 ) ;
#32472 = CARTESIAN_POINT ( 'NONE',  ( 29.40937500061451715, 0.000000000000000000, 5.243569643749999010 ) ) ;
#32473 = CARTESIAN_POINT ( 'NONE',  ( -4.243569643749999898, 13.91562500061451679, 27.54997392385601529 ) ) ;
#32474 = CARTESIAN_POINT ( 'NONE',  ( 17.48437500061451999, 6.421520780324663323E-16, -5.243569643749999010 ) ) ;
#32475 = CARTESIAN_POINT ( 'NONE',  ( 15.22500000122903252, 2.886751345948126879, 4.999999999999999112 ) ) ;
#32476 = CARTESIAN_POINT ( 'NONE',  ( 10.80937500061451928, 4.119189519843966529, -2.378215178124998275 ) ) ;
#32477 = CARTESIAN_POINT ( 'NONE',  ( -4.243569643749999898, 19.40937500061451715, -30.00000000000000000 ) ) ;
#32478 = CARTESIAN_POINT ( 'NONE',  ( 20.25937500061451857, 4.541064518000418104, -2.621784821874998173 ) ) ;
#32479 = CARTESIAN_POINT ( 'NONE',  ( 22.27500000122903145, 2.886751345948129099, -4.999999999999998224 ) ) ;
#32480 =( BOUNDED_CURVE ( )  B_SPLINE_CURVE ( 2, ( #50154, #16514, #23147, #51602, #44253, #67154, #22066 ),
 .UNSPECIFIED., .F., .F. ) 
 B_SPLINE_CURVE_WITH_KNOTS ( ( 3, 2, 2, 3 ),
 ( 0.01999999999999995878, 0.02333333333333328583, 0.02666666666666661634, 0.02999999999999993991 ),
 .UNSPECIFIED. ) 
 CURVE ( )  GEOMETRIC_REPRESENTATION_ITEM ( )  RATIONAL_B_SPLINE_CURVE ( ( 1.000000000000001554, 0.8660254037844370423, 1.000000000000000000, 0.8660254037844387076, 1.000000000000000000, 0.8660254037844410391, 0.9999999999999976685 ) ) 
 REPRESENTATION_ITEM ( '' )  );
#32481 = CARTESIAN_POINT ( 'NONE',  ( 17.44687500061451857, -3.027376345333610441, -5.243569643749999898 ) ) ;
#32482 = CARTESIAN_POINT ( 'NONE',  ( 11.20312500061451644, 4.541064518000418104, -2.621784821874998173 ) ) ;
#32483 = CARTESIAN_POINT ( 'NONE',  ( -2.121784821874996840, 13.63437500061451857, 33.67503911421598417 ) ) ;
#32484 = CARTESIAN_POINT ( 'NONE',  ( 17.27812500061451217, -4.541064518000419881, 2.621784821874995952 ) ) ;
#32485 = ORIENTED_EDGE ( 'NONE', *, *, #14319, .F. ) ;
#32486 = CARTESIAN_POINT ( 'NONE',  ( 23.81250000000000000, -5.773502691896255534, -1.060575238724906372E-15 ) ) ;
#32487 = CARTESIAN_POINT ( 'NONE',  ( 4.243569643749999898, 18.73437500061451644, -30.00000000000000000 ) ) ;
#32488 = CARTESIAN_POINT ( 'NONE',  ( 12.48749999999999893, -2.886751345948063374, 5.000000000000112799 ) ) ;
#32489 = CARTESIAN_POINT ( 'NONE',  ( 25.67812500061451431, 4.541064518000418104, 2.621784821874999949 ) ) ;
#32490 = CARTESIAN_POINT ( 'NONE',  ( 5.728125000614515905, 6.421520780324663323E-16, -5.243569643749999010 ) ) ;
#32491 = CARTESIAN_POINT ( 'NONE',  ( 18.26250000122903216, 4.330127018922192761, -2.499999999999997780 ) ) ;
#32492 = CARTESIAN_POINT ( 'NONE',  ( 23.16562500061451502, -6.054752690667223547, -1.112240025338166033E-15 ) ) ;
#32493 = CARTESIAN_POINT ( 'NONE',  ( 23.92499999999999716, 6.123233995736764310E-16, -4.999999999999998224 ) ) ;
#32494 = EDGE_CURVE ( 'NONE', #60311, #24417, #2084, .T. ) ;
#32495 = CARTESIAN_POINT ( 'NONE',  ( 26.27812500061451573, -4.541064518000419881, 2.621784821874995952 ) ) ;
#32496 = CARTESIAN_POINT ( 'NONE',  ( 9.290625000614515017, -3.027376345333610441, -5.243569643749999898 ) ) ;
#32497 = VERTEX_POINT ( 'NONE', #58568 ) ;
#32498 = CARTESIAN_POINT ( 'NONE',  ( 22.34062500061451573, -3.027376345333610441, -5.243569643749999898 ) ) ;
#32499 = CARTESIAN_POINT ( 'NONE',  ( 3.103125000614517237, 4.541064518000418104, -2.621784821874998173 ) ) ;
#32500 = VECTOR ( 'NONE', #49450, 1000.000000000000000 ) ;
#32501 = CARTESIAN_POINT ( 'NONE',  ( 12.57187500061451857, 2.746126346562645981, -4.756430356249997438 ) ) ;
#32502 = CARTESIAN_POINT ( 'NONE',  ( -1.071796769724475906, 11.02009619066136636, 25.99999999999999289 ) ) ;
#32503 = CARTESIAN_POINT ( 'NONE',  ( -3.999999999999997335, 14.75000000122903288, -27.69059892324149175 ) ) ;
#32504 = CARTESIAN_POINT ( 'NONE',  ( 11.47499999999999964, 4.330127018922191873, 2.499999999999999556 ) ) ;
#32506 = CARTESIAN_POINT ( 'NONE',  ( 10.92187500061451644, 3.027376345333611329, 5.243569643749999010 ) ) ;
#32505 = VECTOR ( 'NONE', #55794, 1000.000000000000000 ) ;
#32507 = CARTESIAN_POINT ( 'NONE',  ( 6.937500001229033764, 6.123233995736764310E-16, -4.999999999999998224 ) ) ;
#32508 = CARTESIAN_POINT ( 'NONE',  ( 15.34687500061451537, 6.054752690667223547, 3.707466751127219781E-16 ) ) ;
#32509 = CARTESIAN_POINT ( 'NONE',  ( 6.721875000614518925, 3.027376345333613106, -5.243569643749998122 ) ) ;
#32510 = VECTOR ( 'NONE', #43348, 1000.000000000000000 ) ;
#32511 = CARTESIAN_POINT ( 'NONE',  ( 1.626862140677534273E-15, 10.77500000122903323, 34.00000000000000000 ) ) ;
#32512 = CARTESIAN_POINT ( 'NONE',  ( 12.42187500061451821, -6.054752690667223547, -1.112240025338166033E-15 ) ) ;
#32513 = FACE_OUTER_BOUND ( 'NONE', #28276, .T. ) ;
#32514 = CARTESIAN_POINT ( 'NONE',  ( 21.40312500061451573, -4.541064518000417216, -2.621784821875001281 ) ) ;
#32515 = CARTESIAN_POINT ( 'NONE',  ( -3.999999999999997335, 12.50000000122903465, -27.69059892324149530 ) ) ;
#32516 = CARTESIAN_POINT ( 'NONE',  ( 4.243569643749999898, 18.64062500061459104, 32.45002607614398471 ) ) ;
#32517 = CARTESIAN_POINT ( 'NONE',  ( 22.62187500061451573, 3.027376345333611329, 5.243569643749999010 ) ) ;
#32518 = DIRECTION ( 'NONE',  ( 0.000000000000000000, 0.000000000000000000, -1.000000000000000000 ) ) ;
#32519 = CARTESIAN_POINT ( 'NONE',  ( 27.78750000122903074, 4.330127018922191873, 2.499999999999999556 ) ) ;
#32520 = CARTESIAN_POINT ( 'NONE',  ( 19.32187500061451857, 4.119189519843966529, 2.378215178124999607 ) ) ;
#32521 = CARTESIAN_POINT ( 'NONE',  ( 25.82812500061451644, -4.541064518000419881, 2.621784821874995952 ) ) ;
#32522 = CARTESIAN_POINT ( 'NONE',  ( 17.31562500061451715, -6.054752690667223547, -1.112240025338166033E-15 ) ) ;
#32523 = CARTESIAN_POINT ( 'NONE',  ( 14.41875000122903394, -5.773502691896255534, -1.060575238724906372E-15 ) ) ;
#32524 = CARTESIAN_POINT ( 'NONE',  ( 14.37187500061451928, 3.027376345333613106, -5.243569643749998122 ) ) ;
#32525 = CARTESIAN_POINT ( 'NONE',  ( 16.87500000000000000, 4.330127018922191873, 2.499999999999999556 ) ) ;
#32526 = CARTESIAN_POINT ( 'NONE',  ( 28.20000000122903216, 5.773502691896255534, 3.535250795749688894E-16 ) ) ;
#32527 = CARTESIAN_POINT ( 'NONE',  ( 4.809375000614516615, -4.541064518000417216, -2.621784821875001281 ) ) ;
#32528 = CARTESIAN_POINT ( 'NONE',  ( 15.79687500061451821, 6.054752690667223547, 3.707466751127219781E-16 ) ) ;
#32529 = CARTESIAN_POINT ( 'NONE',  ( 16.12500000000000000, -4.330127018922194537, 2.499999999999995559 ) ) ;
#32530 = EDGE_CURVE ( 'NONE', #50028, #45391, #69377, .T. ) ;
#32531 = CARTESIAN_POINT ( 'NONE',  ( 4.725000001229034297, 2.886751345948129099, -4.999999999999998224 ) ) ;
#32532 = CARTESIAN_POINT ( 'NONE',  ( 24.27187500061452141, 3.027376345333613106, -5.243569643749998122 ) ) ;
#32533 = CARTESIAN_POINT ( 'NONE',  ( 17.52187500061451431, 3.027376345333613106, -5.243569643749998122 ) ) ;
#32534 = CARTESIAN_POINT ( 'NONE',  ( -3.756430356249999214, 16.09062499938548285, 27.83122392262697531 ) ) ;
#32535 = CARTESIAN_POINT ( 'NONE',  ( 29.13749999999999929, -2.886751345948129988, 4.999999999999997335 ) ) ;
#32536 = CARTESIAN_POINT ( 'NONE',  ( 5.962500000000002132, 2.886751345948129099, -4.999999999999998224 ) ) ;
#32537 = CARTESIAN_POINT ( 'NONE',  ( 29.70937500061451431, 4.119189519843966529, -2.378215178124998275 ) ) ;
#32538 = CARTESIAN_POINT ( 'NONE',  ( 20.76562500061451644, 3.027376345333611329, 5.243569643749999010 ) ) ;
#32539 = CARTESIAN_POINT ( 'NONE',  ( 8.625000000000000000, 6.123233995736764310E-16, -4.999999999999998224 ) ) ;
#32540 = CARTESIAN_POINT ( 'NONE',  ( 4.903125000614516615, 4.541064518000418104, -2.621784821874998173 ) ) ;
#32541 = CARTESIAN_POINT ( 'NONE',  ( 20.24999999999999645, -4.330127018922190985, -2.500000000000001332 ) ) ;
#32542 = CARTESIAN_POINT ( 'NONE',  ( 1.999999999999997335, 16.41874999877096641, 33.46410161513775705 ) ) ;
#32543 = CARTESIAN_POINT ( 'NONE',  ( 24.33750000122903145, -4.330127018922194537, 2.499999999999995559 ) ) ;
#32544 = CARTESIAN_POINT ( 'NONE',  ( 5.192387018522387265, 8.549830518147031100, 33.03071326595781443 ) ) ;
#32545 = CARTESIAN_POINT ( 'NONE',  ( 3.037500000000002309, -2.886751345948129988, 4.999999999999997335 ) ) ;
#32546 = VECTOR ( 'NONE', #27493, 1000.000000000000227 ) ;
#32547 = ORIENTED_EDGE ( 'NONE', *, *, #11487, .F. ) ;
#32548 = CARTESIAN_POINT ( 'NONE',  ( 18.29062500061451502, -3.027376345333610441, -5.243569643749999898 ) ) ;
#32549 = CARTESIAN_POINT ( 'NONE',  ( 23.27812500061451573, 6.421520780324663323E-16, -5.243569643749999010 ) ) ;
#32550 = CARTESIAN_POINT ( 'NONE',  ( 23.67187500061451999, -6.054752690667223547, -1.112240025338166033E-15 ) ) ;
#32551 = CARTESIAN_POINT ( 'NONE',  ( 6.524999999999999467, 4.330127018922191873, 2.499999999999999556 ) ) ;
#32552 = CARTESIAN_POINT ( 'NONE',  ( 12.81562500061451537, -6.054752690667223547, -1.112240025338166033E-15 ) ) ;
#32553 = CARTESIAN_POINT ( 'NONE',  ( 25.64062500061451644, 6.054752690667223547, 3.707466751127219781E-16 ) ) ;
#32554 = CARTESIAN_POINT ( 'NONE',  ( 15.27187500061451786, 3.027376345333613106, -5.243569643749998122 ) ) ;
#32555 = CARTESIAN_POINT ( 'NONE',  ( 20.40937500061451715, 0.000000000000000000, 5.243569643749999010 ) ) ;
#32556 = CARTESIAN_POINT ( 'NONE',  ( 21.11250000122903359, 0.000000000000000000, 4.999999999999998224 ) ) ;
#32557 = CARTESIAN_POINT ( 'NONE',  ( 2.121784821875001281, 10.55937500061451750, 33.67503911421598417 ) ) ;
#32558 = CARTESIAN_POINT ( 'NONE',  ( 23.92500000122903359, -5.773502691896255534, -1.060575238724906372E-15 ) ) ;
#32559 = CARTESIAN_POINT ( 'NONE',  ( 18.04687500061451999, 5.492252693125287522, 3.363034840372157021E-16 ) ) ;
#32560 = CARTESIAN_POINT ( 'NONE',  ( 14.80312500061451608, 4.541064518000418104, -2.621784821874998173 ) ) ;
#32561 = CARTESIAN_POINT ( 'NONE',  ( 6.871875000614517504, 3.027376345333611329, 5.243569643749999010 ) ) ;
#32562 = CARTESIAN_POINT ( 'NONE',  ( 7.359375000614516438, 0.000000000000000000, 5.243569643749999010 ) ) ;
#32563 = VERTEX_POINT ( 'NONE', #35680 ) ;
#32564 = CARTESIAN_POINT ( 'NONE',  ( 28.09687500061451360, -3.027376345333614438, 5.243569643749998122 ) ) ;
#32565 = CARTESIAN_POINT ( 'NONE',  ( 18.85312500061451502, 4.541064518000418104, -2.621784821874998173 ) ) ;
#32566 = CARTESIAN_POINT ( 'NONE',  ( 29.62500000122903288, 2.886751345948126879, 4.999999999999999112 ) ) ;
#32567 = CARTESIAN_POINT ( 'NONE',  ( 29.46562500061451573, -6.054752690667223547, -1.112240025338166033E-15 ) ) ;
#32568 = CARTESIAN_POINT ( 'NONE',  ( 24.04687500061451644, -3.027376345333614438, 5.243569643749998122 ) ) ;
#32569 = CARTESIAN_POINT ( 'NONE',  ( 19.37812500061451715, 4.541064518000418104, 2.621784821874999949 ) ) ;
#32570 = CARTESIAN_POINT ( 'NONE',  ( -3.999999999999999112, 11.00000000000000178, 30.00000000000000000 ) ) ;
#32571 = CARTESIAN_POINT ( 'NONE',  ( 24.14062500061451289, -3.027376345333610441, -5.243569643749999898 ) ) ;
#32572 = CARTESIAN_POINT ( 'NONE',  ( 5.700000001229033941, 5.773502691896255534, 3.535250795749688894E-16 ) ) ;
#32573 = ORIENTED_EDGE ( 'NONE', *, *, #10710, .T. ) ;
#32574 = CARTESIAN_POINT ( 'NONE',  ( 29.06250000000000000, 2.886751345948126879, 4.999999999999999112 ) ) ;
#32575 = CARTESIAN_POINT ( 'NONE',  ( -1.999999999999997113, 15.57500000000000284, -26.53589838486224295 ) ) ;
#32576 = CARTESIAN_POINT ( 'NONE',  ( 22.57500000122903572, -5.773502691896255534, -1.060575238724906372E-15 ) ) ;
#32577 = CARTESIAN_POINT ( 'NONE',  ( 1.878215178124997609, 15.82812499938548356, 33.25316411605952993 ) ) ;
#32578 = CARTESIAN_POINT ( 'NONE',  ( 5.259375000614518569, -4.541064518000417216, -2.621784821875001281 ) ) ;
#32579 = CARTESIAN_POINT ( 'NONE',  ( 28.97812500061451502, -4.541064518000419881, 2.621784821874995952 ) ) ;
#32580 = CARTESIAN_POINT ( 'NONE',  ( 11.65312500061451573, 4.541064518000418104, -2.621784821874998173 ) ) ;
#32581 = CARTESIAN_POINT ( 'NONE',  ( 5.746875000614517504, -3.027376345333610441, -5.243569643749999898 ) ) ;
#32582 = CARTESIAN_POINT ( 'NONE',  ( 24.18750000122903288, 4.330127018922191873, 2.499999999999999556 ) ) ;
#32583 = CARTESIAN_POINT ( 'NONE',  ( 14.85937500061451644, 4.541064518000418104, -2.621784821874998173 ) ) ;
#32584 = CARTESIAN_POINT ( 'NONE',  ( 29.01562500061451644, -6.054752690667223547, -1.112240025338166033E-15 ) ) ;
#32585 = CARTESIAN_POINT ( 'NONE',  ( 7.950000001229033053, 5.773502691896255534, 3.535250795749688401E-16 ) ) ;
#32586 = CARTESIAN_POINT ( 'NONE',  ( 3.028125000614518392, 6.421520780324663323E-16, -5.243569643749999010 ) ) ;
#32587 = CARTESIAN_POINT ( 'NONE',  ( 15.25312500061451715, 4.541064518000418104, -2.621784821874998173 ) ) ;
#32588 = ADVANCED_FACE ( 'NONE', ( #30868 ), #59293, .T. ) ;
#32589 = ORIENTED_EDGE ( 'NONE', *, *, #26409, .T. ) ;
#32590 = CARTESIAN_POINT ( 'NONE',  ( 9.103125000614515017, 0.000000000000000000, 5.243569643749999010 ) ) ;
#32591 = CARTESIAN_POINT ( 'NONE',  ( 8.203125000614518214, 0.000000000000000000, 5.243569643749999010 ) ) ;
#32592 = CARTESIAN_POINT ( 'NONE',  ( 19.09687500061451360, -2.746126346562646425, 4.756430356249996549 ) ) ;
#32593 = CARTESIAN_POINT ( 'NONE',  ( 8.699999999999999289, 4.330127018922192761, -2.499999999999997780 ) ) ;
#32594 = CARTESIAN_POINT ( 'NONE',  ( 5.025000001229035895, -5.773502691896255534, -1.060575238724906372E-15 ) ) ;
#32595 = CARTESIAN_POINT ( 'NONE',  ( 18.75000000000000000, 0.000000000000000000, 4.999999999999998224 ) ) ;
#32596 = CARTESIAN_POINT ( 'NONE',  ( 19.50937500061451857, 0.000000000000000000, 5.243569643749999010 ) ) ;
#32597 = CARTESIAN_POINT ( 'NONE',  ( 13.57500000122903572, -5.773502691896255534, -1.060575238724906372E-15 ) ) ;
#32598 = CARTESIAN_POINT ( 'NONE',  ( 20.81250000000000000, 2.886751345948129099, -4.999999999999998224 ) ) ;
#32599 = CARTESIAN_POINT ( 'NONE',  ( -4.243569643749999898, 16.20312500061451644, -30.00000000000000000 ) ) ;
#32600 = LINE ( 'NONE', #60288, #11157 ) ;
#32601 = CARTESIAN_POINT ( 'NONE',  ( 3.486133158594716510E-16, 19.55000000122903359, 26.00000000000000355 ) ) ;
#32602 = CARTESIAN_POINT ( 'NONE',  ( 29.12812500061451715, 6.421520780324663323E-16, -5.243569643749999010 ) ) ;
#32603 = CARTESIAN_POINT ( 'NONE',  ( 3.999999999999999112, 19.77500000000000213, 30.00000000000000000 ) ) ;
#32604 = CARTESIAN_POINT ( 'NONE',  ( 3.999999999999999112, 16.17500000000000071, -30.00000000000000000 ) ) ;
#32605 = CARTESIAN_POINT ( 'NONE',  ( 13.05937500061451750, 4.541064518000418104, -2.621784821874998173 ) ) ;
#32606 = CARTESIAN_POINT ( 'NONE',  ( 26.17500000000000071, 6.123233995736764310E-16, -4.999999999999998224 ) ) ;
#32607 = CARTESIAN_POINT ( 'NONE',  ( 8.953125000614518214, 4.541064518000418104, -2.621784821874998173 ) ) ;
#32608 = CARTESIAN_POINT ( 'NONE',  ( 27.19687500061451502, -4.119189519843965641, -2.378215178125001383 ) ) ;
#32609 = CARTESIAN_POINT ( 'NONE',  ( 21.08437500061451786, 6.421520780324663323E-16, -5.243569643749999010 ) ) ;
#32610 = CARTESIAN_POINT ( 'NONE',  ( 12.90937500061451537, 2.746126346562645981, -4.756430356249997438 ) ) ;
#32611 = CARTESIAN_POINT ( 'NONE',  ( 7.565625000614518036, 3.027376345333613106, -5.243569643749998122 ) ) ;
#32612 = CARTESIAN_POINT ( 'NONE',  ( 14.33437500061451786, 6.421520780324663323E-16, -5.243569643749999010 ) ) ;
#32613 = VERTEX_POINT ( 'NONE', #2433 ) ;
#32614 = CARTESIAN_POINT ( 'NONE',  ( 22.69687500061451857, -3.027376345333614438, 5.243569643749998122 ) ) ;
#32615 = CARTESIAN_POINT ( 'NONE',  ( 1.838027276006276800, 4.657088507379087083, -26.43727524967973608 ) ) ;
#32616 = DIRECTION ( 'NONE',  ( 0.000000000000000000, 0.000000000000000000, 1.000000000000000000 ) ) ;
#32617 = CARTESIAN_POINT ( 'NONE',  ( 5.325000000000000178, -4.330127018922194537, 2.499999999999995559 ) ) ;
#32618 = CARTESIAN_POINT ( 'NONE',  ( 16.27500000122903501, -5.773502691896255534, -1.060575238724906372E-15 ) ) ;
#32619 = LINE ( 'NONE', #38152, #64351 ) ;
#32620 = CARTESIAN_POINT ( 'NONE',  ( 19.08749999999999858, 5.773502691896255534, 3.535250795749688401E-16 ) ) ;
#32621 = ORIENTED_EDGE ( 'NONE', *, *, #68031, .F. ) ;
#32622 = CARTESIAN_POINT ( 'NONE',  ( 12.82499999999999929, 4.330127018922191873, 2.499999999999999556 ) ) ;
#32623 = CARTESIAN_POINT ( 'NONE',  ( 16.91250000000000142, 2.886751345948126879, 4.999999999999999112 ) ) ;
#32624 = CARTESIAN_POINT ( 'NONE',  ( 13.76250000122903394, 4.330127018922192761, -2.499999999999997780 ) ) ;
#32625 = CARTESIAN_POINT ( 'NONE',  ( 10.75312500061451715, 4.541064518000418104, -2.621784821874998173 ) ) ;
#32626 = ORIENTED_EDGE ( 'NONE', *, *, #70340, .T. ) ;
#32627 = DIRECTION ( 'NONE',  ( -1.000000000000000000, -0.000000000000000000, -0.000000000000000000 ) ) ;
#32628 = CARTESIAN_POINT ( 'NONE',  ( -3.000416591977282496E-16, 13.89687500061451786, -34.90005215228797653 ) ) ;
#32629 = CARTESIAN_POINT ( 'NONE',  ( 3.703125000614516882, 0.000000000000000000, 5.243569643749999010 ) ) ;
#32630 = CARTESIAN_POINT ( 'NONE',  ( -3.756430356250000990, 13.80312499938548321, 32.16877607737301048 ) ) ;
#32631 = CARTESIAN_POINT ( 'NONE',  ( 9.899999999999998579, -4.330127018922190985, -2.500000000000001332 ) ) ;
#32632 = DIRECTION ( 'NONE',  ( -1.000000000000000000, -0.000000000000000000, -0.000000000000000000 ) ) ;
#32633 = ORIENTED_EDGE ( 'NONE', *, *, #1892, .F. ) ;
#32634 = CARTESIAN_POINT ( 'NONE',  ( 24.89062500061451644, -3.027376345333614438, 5.243569643749998122 ) ) ;
#32635 = CARTESIAN_POINT ( 'NONE',  ( 4.196964255440878588, -2.717639258240006406, 4.484364939275536699 ) ) ;
#32636 = CARTESIAN_POINT ( 'NONE',  ( -3.756430356249999214, 20.02812499938548285, 27.83122392262697531 ) ) ;
#32637 = CARTESIAN_POINT ( 'NONE',  ( 21.00937500061451857, -4.541064518000417216, -2.621784821875001281 ) ) ;
#32638 = CARTESIAN_POINT ( 'NONE',  ( 18.77812500061451573, 6.421520780324663323E-16, -5.243569643749999010 ) ) ;
#32639 = CARTESIAN_POINT ( 'NONE',  ( 2.121784821875001281, 15.00312500061459531, -26.32496088578401938 ) ) ;
#32640 = CARTESIAN_POINT ( 'NONE',  ( 6.515625000614516438, -6.054752690667223547, -1.112240025338166033E-15 ) ) ;
#32641 = CARTESIAN_POINT ( 'NONE',  ( 5.278125000614516615, 6.421520780324663323E-16, -5.243569643749999010 ) ) ;
#32642 = CARTESIAN_POINT ( 'NONE',  ( 25.28437500061451715, 4.119189519843966529, 2.378215178124999607 ) ) ;
#32643 = CARTESIAN_POINT ( 'NONE',  ( 20.54062500061451502, -3.027376345333610441, -5.243569643749999898 ) ) ;
#32644 = CARTESIAN_POINT ( 'NONE',  ( 8.071875000614518569, 2.746126346562645981, -4.756430356249997438 ) ) ;
#32645 = CARTESIAN_POINT ( 'NONE',  ( -7.967954043666661671E-16, 17.47812499938548214, 34.33755215474603517 ) ) ;
#32646 = CARTESIAN_POINT ( 'NONE',  ( 15.53437500061451715, -4.541064518000419881, 2.621784821874995952 ) ) ;
#32647 = CARTESIAN_POINT ( 'NONE',  ( 14.85937500061451644, 4.541064518000418104, -2.621784821874998173 ) ) ;
#32648 = CARTESIAN_POINT ( 'NONE',  ( 22.80937500061451573, -4.541064518000417216, -2.621784821875001281 ) ) ;
#32649 = ORIENTED_EDGE ( 'NONE', *, *, #22474, .T. ) ;
#32650 = CARTESIAN_POINT ( 'NONE',  ( 4.243569643749999010, 11.57187500061451679, 27.54997392385601174 ) ) ;
#32651 = CARTESIAN_POINT ( 'NONE',  ( -1.071796769724491005, 14.62009619066136779, -34.00000000000000000 ) ) ;
#32652 = CARTESIAN_POINT ( 'NONE',  ( 27.51562500061451644, 3.027376345333611329, 5.243569643749999010 ) ) ;
#32653 = EDGE_CURVE ( 'NONE', #19034, #14527, #24455, .T. ) ;
#32654 = CARTESIAN_POINT ( 'NONE',  ( 27.32812500061451644, 6.421520780324663323E-16, -5.243569643749999010 ) ) ;
#32655 = CARTESIAN_POINT ( 'NONE',  ( 2.000000000000001332, 16.21250000122903501, -26.53589838486224650 ) ) ;
#32656 = CARTESIAN_POINT ( 'NONE',  ( -2.828200636599751609E-16, 19.43750000000000000, 25.38119784648299770 ) ) ;
#32657 = AXIS2_PLACEMENT_3D ( 'NONE', #58730, #12591, #1160 ) ;
#32658 = CARTESIAN_POINT ( 'NONE',  ( 3.684375000614518836, 4.541064518000418104, 2.621784821874999949 ) ) ;
#32659 = CARTESIAN_POINT ( 'NONE',  ( 14.43750000122903288, -4.330127018922194537, 2.499999999999995559 ) ) ;
#32660 = CARTESIAN_POINT ( 'NONE',  ( 9.937500001229032875, -4.330127018922194537, 2.499999999999995559 ) ) ;
#32661 = CARTESIAN_POINT ( 'NONE',  ( 3.515625000614516882, 3.027376345333613106, -5.243569643749998122 ) ) ;
#32662 = CARTESIAN_POINT ( 'NONE',  ( -1.999999999999999112, 15.74374999877096570, 26.53589838486224650 ) ) ;
#32663 = CARTESIAN_POINT ( 'NONE',  ( 18.35625000122903216, 0.000000000000000000, 4.999999999999998224 ) ) ;
#32664 = CARTESIAN_POINT ( 'NONE',  ( 10.95937500061451964, 0.000000000000000000, 5.243569643749999010 ) ) ;
#32665 = CARTESIAN_POINT ( 'NONE',  ( 21.43125000122903145, 4.330127018922191873, 2.499999999999999556 ) ) ;
#32666 = VERTEX_POINT ( 'NONE', #25325 ) ;
#32667 = CARTESIAN_POINT ( 'NONE',  ( 20.50312500061451715, -4.541064518000417216, -2.621784821875001281 ) ) ;
#32668 = CARTESIAN_POINT ( 'NONE',  ( 14.78437500061451715, 6.421520780324663323E-16, -5.243569643749999010 ) ) ;
#32669 = CARTESIAN_POINT ( 'NONE',  ( 5.390625000614518214, 6.054752690667223547, 3.707466751127219781E-16 ) ) ;
#32670 = CARTESIAN_POINT ( 'NONE',  ( 21.90937500061451715, -4.541064518000417216, -2.621784821875001281 ) ) ;
#32671 = CARTESIAN_POINT ( 'NONE',  ( 5.203125000614518214, -4.541064518000417216, -2.621784821875001281 ) ) ;
#32672 = CARTESIAN_POINT ( 'NONE',  ( -1.071796769724486120, 16.36115380933863150, 34.00000000000000000 ) ) ;
#32673 = CARTESIAN_POINT ( 'NONE',  ( 7.912500001229033408, 4.330127018922192761, -2.499999999999997780 ) ) ;
#32674 = CARTESIAN_POINT ( 'NONE',  ( 22.97812500061451857, 4.541064518000418104, 2.621784821874999949 ) ) ;
#32675 = EDGE_CURVE ( 'NONE', #38481, #55366, #7006, .T. ) ;
#32676 = CARTESIAN_POINT ( 'NONE',  ( -3.999999999999997335, 18.80000000122903359, -27.69059892324149175 ) ) ;
#32677 = CARTESIAN_POINT ( 'NONE',  ( 7.875000001229034652, 2.886751345948129099, -4.999999999999998224 ) ) ;
#32678 = CARTESIAN_POINT ( 'NONE',  ( 19.52812500061451573, -4.541064518000419881, 2.621784821874995952 ) ) ;
#32679 = CARTESIAN_POINT ( 'NONE',  ( 14.76562500061451821, 3.027376345333613106, -5.243569643749998122 ) ) ;
#32680 = CARTESIAN_POINT ( 'NONE',  ( 27.00937500061451857, 4.119189519843966529, -2.378215178124998275 ) ) ;
#32681 = CARTESIAN_POINT ( 'NONE',  ( 15.33750000000000036, -2.886751345948125991, -5.000000000000000000 ) ) ;
#32682 = CARTESIAN_POINT ( 'NONE',  ( 12.56250000122903465, 0.000000000000000000, 4.999999999999998224 ) ) ;
#32683 = CARTESIAN_POINT ( 'NONE',  ( 7.003125000614518036, -4.541064518000417216, -2.621784821875001281 ) ) ;
#32684 = CARTESIAN_POINT ( 'NONE',  ( 11.27812500061451573, 4.541064518000418104, 2.621784821874999949 ) ) ;
#32685 = EDGE_CURVE ( 'NONE', #52965, #40553, #14239, .T. ) ;
#32686 = CARTESIAN_POINT ( 'NONE',  ( 21.00000000122903288, 5.773502691896255534, 3.535250795749688894E-16 ) ) ;
#32687 = CARTESIAN_POINT ( 'NONE',  ( 2.121784821874999061, 13.40937500061451892, -33.67503911421598417 ) ) ;
#32688 = CARTESIAN_POINT ( 'NONE',  ( 20.52187500061451786, -6.054752690667223547, -1.112240025338166033E-15 ) ) ;
#32689 = CARTESIAN_POINT ( 'NONE',  ( 4.990567482066851746, 0.3502114279239787464, 5.133889258466388661 ) ) ;
#32690 = VECTOR ( 'NONE', #7334, 1000.000000000000000 ) ;
#32691 = CARTESIAN_POINT ( 'NONE',  ( 5.437500001229035540, -4.330127018922194537, 2.499999999999995559 ) ) ;
#32692 = CIRCLE ( 'NONE', #51581, 14.99999999999999822 ) ;
#32693 = CARTESIAN_POINT ( 'NONE',  ( 3.384375000614517237, -4.541064518000419881, 2.621784821874995952 ) ) ;
#32694 = CARTESIAN_POINT ( 'NONE',  ( 21.23437500061451644, 4.541064518000418104, 2.621784821874999949 ) ) ;
#32695 =( BOUNDED_CURVE ( )  B_SPLINE_CURVE ( 2, ( #32102, #26565, #29991, #49105, #46631, #1575, #15459, #18533, #41098 ),
 .UNSPECIFIED., .F., .F. ) 
 B_SPLINE_CURVE_WITH_KNOTS ( ( 3, 2, 2, 2, 3 ),
 ( 0.2934782608695652439, 0.2971014492753623060, 0.3043478260869565410, 0.3115942028985507206, 0.3152173913043478382 ),
 .UNSPECIFIED. ) 
 CURVE ( )  GEOMETRIC_REPRESENTATION_ITEM ( )  RATIONAL_B_SPLINE_CURVE ( ( 0.9330127018922194093, 0.9330127018922198534, 1.000000000000000000, 0.8660254037844387076, 1.000000000000000000, 0.8660254037844387076, 1.000000000000000000, 0.9330127018922188542, 0.9330127018922194093 ) ) 
 REPRESENTATION_ITEM ( '' )  );
#32696 = CARTESIAN_POINT ( 'NONE',  ( 19.75312500061451360, 4.541064518000418104, -2.621784821874998173 ) ) ;
#32697 = CARTESIAN_POINT ( 'NONE',  ( 10.93125000122903501, 6.123233995736764310E-16, -4.999999999999998224 ) ) ;
#32698 = CARTESIAN_POINT ( 'NONE',  ( 23.21250000000000213, 2.886751345948126879, 4.999999999999998224 ) ) ;
#32699 = CARTESIAN_POINT ( 'NONE',  ( 13.12500000000000178, 6.123233995736764310E-16, -4.999999999999998224 ) ) ;
#32700 = CARTESIAN_POINT ( 'NONE',  ( 29.85937500061451644, 0.000000000000000000, 5.243569643749999010 ) ) ;
#32701 = CARTESIAN_POINT ( 'NONE',  ( 20.07187500061451502, 5.824947211148865298E-16, -4.756430356249998326 ) ) ;
#32702 = CARTESIAN_POINT ( 'NONE',  ( 15.66562500061451857, 3.027376345333613106, -5.243569643749998122 ) ) ;
#32703 = CARTESIAN_POINT ( 'NONE',  ( 12.12187500061451573, 3.027376345333613106, -5.243569643749998122 ) ) ;
#32704 = VERTEX_POINT ( 'NONE', #8703 ) ;
#32705 = CARTESIAN_POINT ( 'NONE',  ( 3.999999999999999112, 17.07499999999999929, -30.00000000000000000 ) ) ;
#32706 = CARTESIAN_POINT ( 'NONE',  ( 22.37812500061451360, 6.421520780324663323E-16, -5.243569643749999010 ) ) ;
#32707 = DIRECTION ( 'NONE',  ( 0.000000000000000000, 0.000000000000000000, -1.000000000000000000 ) ) ;
#32708 = CARTESIAN_POINT ( 'NONE',  ( 14.66249999999999787, 2.886751345948193936, 4.999999999999883649 ) ) ;
#32709 = CARTESIAN_POINT ( 'NONE',  ( 13.46249999999999858, -5.773502691896255534, -1.060575238724906372E-15 ) ) ;
#32710 = CARTESIAN_POINT ( 'NONE',  ( 24.45000000122903572, -2.886751345948125991, -5.000000000000000000 ) ) ;
#32711 = CARTESIAN_POINT ( 'NONE',  ( 17.76562500061451644, -6.054752690667223547, -1.112240025338166033E-15 ) ) ;
#32712 = ORIENTED_EDGE ( 'NONE', *, *, #31576, .F. ) ;
#32713 = CARTESIAN_POINT ( 'NONE',  ( 21.97500000000000142, -4.330127018922194537, 2.499999999999995559 ) ) ;
#32714 = CARTESIAN_POINT ( 'NONE',  ( 23.93437500061451573, 4.541064518000418104, 2.621784821874999949 ) ) ;
#32715 = VERTEX_POINT ( 'NONE', #31236 ) ;
#32716 = CARTESIAN_POINT ( 'NONE',  ( 21.28125000122903288, 6.123233995736764310E-16, -4.999999999999998224 ) ) ;
#32717 = CARTESIAN_POINT ( 'NONE',  ( 11.42812500061451608, -4.541064518000419881, 2.621784821874995952 ) ) ;
#32718 = CARTESIAN_POINT ( 'NONE',  ( 10.87500000000000000, 6.123233995736764310E-16, -4.999999999999998224 ) ) ;
#32719 = CARTESIAN_POINT ( 'NONE',  ( 13.32187500061451502, 5.824947211148865298E-16, -4.756430356249998326 ) ) ;
#32720 = CARTESIAN_POINT ( 'NONE',  ( 18.03749999999999787, -2.886751345948125991, -5.000000000000000000 ) ) ;
#32721 = CARTESIAN_POINT ( 'NONE',  ( 23.47499999999999787, 6.123233995736764310E-16, -4.999999999999998224 ) ) ;
#32722 = DIRECTION ( 'NONE',  ( 0.000000000000000000, 0.000000000000000000, 1.000000000000000000 ) ) ;
#32723 = CARTESIAN_POINT ( 'NONE',  ( 5.559375000614517504, 0.000000000000000000, 5.243569643749999010 ) ) ;
#32724 = CARTESIAN_POINT ( 'NONE',  ( 27.53437500061451360, 4.541064518000418104, 2.621784821874999949 ) ) ;
#32725 = VERTEX_POINT ( 'NONE', #48236 ) ;
#32726 = CARTESIAN_POINT ( 'NONE',  ( 25.26562500061451289, 3.027376345333611329, 5.243569643749999010 ) ) ;
#32727 = CARTESIAN_POINT ( 'NONE',  ( 27.60937500061451644, 0.000000000000000000, 5.243569643749999010 ) ) ;
#32728 = CARTESIAN_POINT ( 'NONE',  ( 16.89375000122903359, 5.773502691896255534, 3.535250795749688401E-16 ) ) ;
#32729 = CARTESIAN_POINT ( 'NONE',  ( 13.01249999999999929, -5.773502691896255534, -1.060575238724906372E-15 ) ) ;
#32730 = CARTESIAN_POINT ( 'NONE',  ( 11.27812500061451573, 4.541064518000418104, 2.621784821874999949 ) ) ;
#32731 = CARTESIAN_POINT ( 'NONE',  ( 30.00000000000000000, 0.000000000000000000, 4.999999999999998224 ) ) ;
#32732 = CARTESIAN_POINT ( 'NONE',  ( 7.200000000000001954, -4.330127018922190985, -2.500000000000001332 ) ) ;
#32733 = CARTESIAN_POINT ( 'NONE',  ( 29.42812500061451431, -4.541064518000419881, 2.621784821874995952 ) ) ;
#32734 = CARTESIAN_POINT ( 'NONE',  ( 15.97500000122903430, 2.886751345948129099, -4.999999999999998224 ) ) ;
#32735 = CARTESIAN_POINT ( 'NONE',  ( 29.44687500061451146, -4.119189519843965641, -2.378215178125001383 ) ) ;
#32736 = CARTESIAN_POINT ( 'NONE',  ( 15.00937500061451679, 0.000000000000000000, 4.756430356249998326 ) ) ;
#32737 = CARTESIAN_POINT ( 'NONE',  ( 4.303125000614516971, -4.541064518000417216, -2.621784821875001281 ) ) ;
#32738 = CARTESIAN_POINT ( 'NONE',  ( 22.17187500061451644, 3.027376345333611329, 5.243569643749999010 ) ) ;
#32739 = CARTESIAN_POINT ( 'NONE',  ( -2.121784821874999949, 14.83437500061451786, 26.32496088578401938 ) ) ;
#32740 = CARTESIAN_POINT ( 'NONE',  ( 21.94687500061451857, -3.027376345333610441, -5.243569643749999898 ) ) ;
#32741 = CARTESIAN_POINT ( 'NONE',  ( 29.44687500061451857, -3.027376345333614438, 5.243569643749998122 ) ) ;
#32742 = CARTESIAN_POINT ( 'NONE',  ( -2.121784821874996840, 18.58437500061451786, 33.67503911421598417 ) ) ;
#32743 = CARTESIAN_POINT ( 'NONE',  ( 9.365625000614519635, 3.027376345333613106, -5.243569643749998122 ) ) ;
#32744 = CARTESIAN_POINT ( 'NONE',  ( 2.925000001229034918, 2.886751345948129099, -4.999999999999998224 ) ) ;
#32745 = CARTESIAN_POINT ( 'NONE',  ( 7.509375000614517681, -4.541064518000417216, -2.621784821875001281 ) ) ;
#32746 = CARTESIAN_POINT ( 'NONE',  ( 3.999999999999998668, 15.76250000000000107, -32.30940107675850470 ) ) ;
#32747 = CARTESIAN_POINT ( 'NONE',  ( 10.56562500061451715, -6.054752690667223547, -1.112240025338166033E-15 ) ) ;
#32748 = CARTESIAN_POINT ( 'NONE',  ( 15.34687500061451537, 6.054752690667223547, 3.707466751127219781E-16 ) ) ;
#32749 = CARTESIAN_POINT ( 'NONE',  ( -1.071796769724502107, 18.93259618943233491, 26.00000000000000711 ) ) ;
#32750 = CARTESIAN_POINT ( 'NONE',  ( 21.26250000122903572, -4.330127018922190985, -2.500000000000001332 ) ) ;
#32751 = CARTESIAN_POINT ( 'NONE',  ( 7.771875000614516971, 3.027376345333611329, 5.243569643749999010 ) ) ;
#32752 = CARTESIAN_POINT ( 'NONE',  ( 10.11562500061451608, -6.054752690667223547, -1.112240025338166033E-15 ) ) ;
#32753 = EDGE_CURVE ( 'NONE', #30305, #30532, #42691, .T. ) ;
#32754 = CARTESIAN_POINT ( 'NONE',  ( 26.71875000122903288, 2.886751345948129099, -4.999999999999998224 ) ) ;
#32755 = CARTESIAN_POINT ( 'NONE',  ( 19.54687500061451644, -3.027376345333614438, 5.243569643749998122 ) ) ;
#32756 = CARTESIAN_POINT ( 'NONE',  ( 25.53750000122903074, 4.330127018922191873, 2.499999999999999556 ) ) ;
#32757 = CARTESIAN_POINT ( 'NONE',  ( -4.243569643749999898, 19.80312500061451786, -30.00000000000000000 ) ) ;
#32758 = CARTESIAN_POINT ( 'NONE',  ( 29.10937500061451644, -4.541064518000417216, -2.621784821875001281 ) ) ;
#32759 = CARTESIAN_POINT ( 'NONE',  ( 9.001249775931846008E-16, 10.97187500061451715, -25.09994784771203058 ) ) ;
#32760 = CARTESIAN_POINT ( 'NONE',  ( 15.11250000122903359, 4.330127018922192761, -2.499999999999997780 ) ) ;
#32761 = CARTESIAN_POINT ( 'NONE',  ( -4.243569643749999898, 14.36562500061451786, -32.45002607614398471 ) ) ;
#32762 = CARTESIAN_POINT ( 'NONE',  ( 15.60000000122903607, 5.773502691896255534, 3.535250795749688894E-16 ) ) ;
#32763 = CARTESIAN_POINT ( 'NONE',  ( 9.815625000614518925, 3.027376345333613106, -5.243569643749998122 ) ) ;
#32764 = ORIENTED_EDGE ( 'NONE', *, *, #13900, .T. ) ;
#32765 = CARTESIAN_POINT ( 'NONE',  ( 13.35000000000000142, 0.000000000000000000, 4.999999999999998224 ) ) ;
#32766 = CARTESIAN_POINT ( 'NONE',  ( 45.00000000000000000, 0.000000000000000000, 0.000000000000000000 ) ) ;
#32767 = CARTESIAN_POINT ( 'NONE',  ( 23.46562500061451573, 3.027376345333611329, 5.243569643749999010 ) ) ;
#32768 = CARTESIAN_POINT ( 'NONE',  ( 10.77187500061451786, 3.027376345333612662, -5.243569643749998122 ) ) ;
#32769 = FACE_OUTER_BOUND ( 'NONE', #2269, .T. ) ;
#32770 = CARTESIAN_POINT ( 'NONE',  ( 10.87500000122903288, -5.773502691896255534, -1.060575238724906372E-15 ) ) ;
#32771 = CARTESIAN_POINT ( 'NONE',  ( 18.97500000122903074, -5.773502691896255534, -1.060575238724906372E-15 ) ) ;
#32772 = CARTESIAN_POINT ( 'NONE',  ( 16.04062500061451857, -3.027376345333610441, -5.243569643749999898 ) ) ;
#32773 = CARTESIAN_POINT ( 'NONE',  ( 17.72812500061451502, -4.541064518000419881, 2.621784821874995952 ) ) ;
#32774 = CARTESIAN_POINT ( 'NONE',  ( 26.25000000122903288, -2.886751345948125991, -5.000000000000000000 ) ) ;
#32775 = CARTESIAN_POINT ( 'NONE',  ( 28.20000000122903216, 5.773502691896255534, 3.535250795749688894E-16 ) ) ;
#32776 = CARTESIAN_POINT ( 'NONE',  ( 21.82499999999999574, 4.330127018922191873, 2.499999999999999556 ) ) ;
#32777 = CARTESIAN_POINT ( 'NONE',  ( -1.878215178125001827, 12.94062499938548427, 33.25316411605952283 ) ) ;
#32778 = CARTESIAN_POINT ( 'NONE',  ( 25.73437500061451644, 4.541064518000418104, 2.621784821874999949 ) ) ;
#32779 = CARTESIAN_POINT ( 'NONE',  ( -1.999999999999997113, 16.02500000000000213, 33.46410161513775705 ) ) ;
#32780 = CARTESIAN_POINT ( 'NONE',  ( 11.62500000122903465, 2.886751345948126879, 4.999999999999999112 ) ) ;
#32781 = CARTESIAN_POINT ( 'NONE',  ( 27.98437500061451289, 4.541064518000418104, 2.621784821874999949 ) ) ;
#32782 = CARTESIAN_POINT ( 'NONE',  ( 12.67499999999999893, 6.123233995736764310E-16, -4.999999999999998224 ) ) ;
#32783 = CARTESIAN_POINT ( 'NONE',  ( 5.521875000614517859, 3.027376345333611329, 5.243569643749999010 ) ) ;
#32784 = CARTESIAN_POINT ( 'NONE',  ( 26.09062500061451573, 6.054752690667223547, 3.707466751127219781E-16 ) ) ;
#32785 = CARTESIAN_POINT ( 'NONE',  ( 4.771875000614516971, -6.054752690667223547, -1.112240025338166033E-15 ) ) ;
#32786 = CARTESIAN_POINT ( 'NONE',  ( 26.08125000122903003, -4.330127018922194537, 2.499999999999995559 ) ) ;
#32787 = CARTESIAN_POINT ( 'NONE',  ( 10.20937500061451786, -4.541064518000417216, -2.621784821875001281 ) ) ;
#32788 = CARTESIAN_POINT ( 'NONE',  ( 22.23750000122903003, 6.123233995736764310E-16, -4.999999999999998224 ) ) ;
#32789 = CARTESIAN_POINT ( 'NONE',  ( 3.946875000614517681, -3.027376345333610441, -5.243569643749999898 ) ) ;
#32790 = CARTESIAN_POINT ( 'NONE',  ( 7.884375000614517681, -4.541064518000419881, 2.621784821874995952 ) ) ;
#32791 = CARTESIAN_POINT ( 'NONE',  ( 28.65937500061451715, -4.541064518000417216, -2.621784821875001281 ) ) ;
#32792 = CARTESIAN_POINT ( 'NONE',  ( 2.121784821874999061, 12.00312500061459531, 26.32496088578401583 ) ) ;
#32793 = CARTESIAN_POINT ( 'NONE',  ( 20.40000000000000213, 4.330127018922192761, -2.499999999999997780 ) ) ;
#32794 = VERTEX_POINT ( 'NONE', #14603 ) ;
#32795 = CARTESIAN_POINT ( 'NONE',  ( 29.06250000000000000, 2.886751345948126879, 4.999999999999999112 ) ) ;
#32796 = CARTESIAN_POINT ( 'NONE',  ( 4.012500000000001954, -5.773502691896255534, -1.060575238724906372E-15 ) ) ;
#32797 = ADVANCED_FACE ( 'NONE', ( #37139 ), #59667, .F. ) ;
#32798 = ORIENTED_EDGE ( 'NONE', *, *, #48942, .T. ) ;
#32799 = CARTESIAN_POINT ( 'NONE',  ( 17.31562500061451715, -6.054752690667223547, -1.112240025338166033E-15 ) ) ;
#32800 = CARTESIAN_POINT ( 'NONE',  ( 7.940625000614518036, -3.027376345333610441, -5.243569643749999898 ) ) ;
#32801 = CARTESIAN_POINT ( 'NONE',  ( 22.24687500061451573, -4.119189519843965641, -2.378215178125001383 ) ) ;
#32802 = CARTESIAN_POINT ( 'NONE',  ( 7.021875000614518747, -6.054752690667223547, -1.112240025338166033E-15 ) ) ;
#32803 = CARTESIAN_POINT ( 'NONE',  ( 16.83750000122903145, 6.123233995736764310E-16, -4.999999999999998224 ) ) ;
#32804 = CARTESIAN_POINT ( 'NONE',  ( 7.546875000614517326, -3.027376345333610441, -5.243569643749999898 ) ) ;
#32805 = CARTESIAN_POINT ( 'NONE',  ( 12.87187500061451750, -6.054752690667223547, -1.112240025338166033E-15 ) ) ;
#32806 = CARTESIAN_POINT ( 'NONE',  ( 23.07187500061451857, 3.027376345333611329, 5.243569643749999010 ) ) ;
#32807 = CARTESIAN_POINT ( 'NONE',  ( 26.73749999999999716, 5.773502691896255534, 3.535250795749688401E-16 ) ) ;
#32808 = EDGE_LOOP ( 'NONE', ( #56553, #27895, #55249, #45585 ) ) ;
#32809 = CARTESIAN_POINT ( 'NONE',  ( 13.35000000000000142, 0.000000000000000000, 4.999999999999998224 ) ) ;
#32810 = CARTESIAN_POINT ( 'NONE',  ( 17.82187500061451502, -6.054752690667223547, -1.112240025338166033E-15 ) ) ;
#32811 = CARTESIAN_POINT ( 'NONE',  ( 9.609375000614518214, 0.000000000000000000, 5.243569643749999010 ) ) ;
#32812 = CARTESIAN_POINT ( 'NONE',  ( 1.878215178125000495, 15.41562499938548392, 26.74683588394047007 ) ) ;
#32813 = CARTESIAN_POINT ( 'NONE',  ( 21.30000000000000071, 4.330127018922192761, -2.499999999999997780 ) ) ;
#32814 = CARTESIAN_POINT ( 'NONE',  ( 2.000000000000000444, 17.52499999999999858, 26.53589838486224650 ) ) ;
#32815 = CARTESIAN_POINT ( 'NONE',  ( -4.000000000000000888, 17.26249999999999929, 32.30940107675850470 ) ) ;
#32816 = CARTESIAN_POINT ( 'NONE',  ( 22.28437500061451715, -4.119189519843968306, 2.378215178124996054 ) ) ;
#32817 = CARTESIAN_POINT ( 'NONE',  ( 13.30312500061451786, -4.541064518000417216, -2.621784821875001281 ) ) ;
#32818 = CARTESIAN_POINT ( 'NONE',  ( 3.374999999999999556, 4.330127018922191873, 2.499999999999999556 ) ) ;
#32819 = CARTESIAN_POINT ( 'NONE',  ( -3.999999999999997335, 19.25000000122903288, -27.69059892324149530 ) ) ;
#32820 = CARTESIAN_POINT ( 'NONE',  ( 28.02187500061451431, 3.027376345333611329, 5.243569643749999010 ) ) ;
#32821 = CARTESIAN_POINT ( 'NONE',  ( 10.87500000000000000, 6.123233995736764310E-16, -4.999999999999998224 ) ) ;
#32822 = CARTESIAN_POINT ( 'NONE',  ( -3.999999999999999556, 16.47500000122903430, 27.69059892324149530 ) ) ;
#32823 = CARTESIAN_POINT ( 'NONE',  ( 8.925000001229033586, 2.886751345948126879, 4.999999999999999112 ) ) ;
#32824 = B_SPLINE_CURVE_WITH_KNOTS ( 'NONE', 3,
 ( #13864, #48591, #3529, #19763, #14227, #14590, #19388, #8690, #53393, #53765 ),
 .UNSPECIFIED., .F., .F.,
 ( 4, 3, 3, 4 ),
 ( 5.217251150924370361E-16, 0.0001572577921159111416, 0.0003064946508897742989, 0.0004559760873501511732 ),
 .UNSPECIFIED. ) ;
#32825 = CARTESIAN_POINT ( 'NONE',  ( 21.42187500061451644, -6.054752690667223547, -1.112240025338166033E-15 ) ) ;
#32826 = CARTESIAN_POINT ( 'NONE',  ( 13.69687500061451679, -3.027376345333614438, 5.243569643749998122 ) ) ;
#32827 = LINE ( 'NONE', #44659, #10036 ) ;
#32828 = ORIENTED_EDGE ( 'NONE', *, *, #43413, .T. ) ;
#32829 = CARTESIAN_POINT ( 'NONE',  ( 16.64062500061451289, 6.054752690667223547, 3.707466751127219781E-16 ) ) ;
#32830 = CARTESIAN_POINT ( 'NONE',  ( 28.05000000122903359, -2.886751345948125991, -5.000000000000000000 ) ) ;
#32831 = CARTESIAN_POINT ( 'NONE',  ( 15.34687500061451537, 6.054752690667223547, 3.707466751127219781E-16 ) ) ;
#32832 = CARTESIAN_POINT ( 'NONE',  ( 27.35625000122903216, 0.000000000000000000, 4.999999999999998224 ) ) ;
#32833 = CARTESIAN_POINT ( 'NONE',  ( 16.22812500061451857, 4.541064518000418104, 2.621784821874999949 ) ) ;
#32834 = EDGE_CURVE ( 'NONE', #8302, #23570, #46782, .T. ) ;
#32835 = CARTESIAN_POINT ( 'NONE',  ( 29.33437500061451431, 4.541064518000418104, 2.621784821874999949 ) ) ;
#32836 = CARTESIAN_POINT ( 'NONE',  ( -2.121784821874996840, 11.77812500061451750, 33.67503911421598417 ) ) ;
#32837 = CARTESIAN_POINT ( 'NONE',  ( 18.34687500061451715, -3.027376345333610441, -5.243569643749999898 ) ) ;
#32838 = CARTESIAN_POINT ( 'NONE',  ( 13.80000000122903181, 5.773502691896255534, 3.535250795749688894E-16 ) ) ;
#32839 = CARTESIAN_POINT ( 'NONE',  ( 11.10937500061451644, -4.119189519843965641, -2.378215178125001383 ) ) ;
#32840 = CARTESIAN_POINT ( 'NONE',  ( 3.317152244841671926, -3.741199378463153646, 3.674032409778095420 ) ) ;
#32841 = CARTESIAN_POINT ( 'NONE',  ( 19.84687500061451360, 6.054752690667223547, 3.707466751127219781E-16 ) ) ;
#32842 = CARTESIAN_POINT ( 'NONE',  ( 21.33750000122903145, 6.123233995736764310E-16, -4.999999999999998224 ) ) ;
#32843 = CARTESIAN_POINT ( 'NONE',  ( 18.19687500061451502, -3.027376345333614438, 5.243569643749998122 ) ) ;
#32844 = CARTESIAN_POINT ( 'NONE',  ( 13.26562500061451644, -6.054752690667223547, -1.112240025338166033E-15 ) ) ;
#32845 = CARTESIAN_POINT ( 'NONE',  ( -3.000416591977282496E-16, 12.09687500061451715, 25.09994784771203058 ) ) ;
#32846 = CARTESIAN_POINT ( 'NONE',  ( 18.55312500061451431, 0.000000000000000000, 5.243569643749999010 ) ) ;
#32847 = ORIENTED_EDGE ( 'NONE', *, *, #35944, .T. ) ;
#32848 = ORIENTED_EDGE ( 'NONE', *, *, #6200, .F. ) ;
#32849 = CARTESIAN_POINT ( 'NONE',  ( 19.50000000000000000, 4.330127018922192761, -2.499999999999997780 ) ) ;
#32850 = CARTESIAN_POINT ( 'NONE',  ( 7.162500001229032520, 0.000000000000000000, 4.999999999999998224 ) ) ;
#32851 = CARTESIAN_POINT ( 'NONE',  ( 25.26562500061451289, 3.027376345333611329, 5.243569643749999010 ) ) ;
#32852 = CARTESIAN_POINT ( 'NONE',  ( 5.278125000614516615, 6.421520780324663323E-16, -5.243569643749999010 ) ) ;
#32853 = CARTESIAN_POINT ( 'NONE',  ( 17.21250000122903145, -4.330127018922190985, -2.500000000000001332 ) ) ;
#32854 = EDGE_CURVE ( 'NONE', #72158, #885, #38617, .T. ) ;
#32855 = CARTESIAN_POINT ( 'NONE',  ( 23.20312500061451644, -4.541064518000417216, -2.621784821875001281 ) ) ;
#32856 = CARTESIAN_POINT ( 'NONE',  ( 22.42500000000000071, -4.330127018922194537, 2.499999999999995559 ) ) ;
#32857 =( BOUNDED_CURVE ( )  B_SPLINE_CURVE ( 2, ( #14223, #19759, #60377, #31218, #36759, #25684, #54492, #71485, #8686 ),
 .UNSPECIFIED., .F., .F. ) 
 B_SPLINE_CURVE_WITH_KNOTS ( ( 3, 2, 2, 2, 3 ),
 ( 0.7361111111111111605, 0.7407407407407406996, 0.7500000000000000000, 0.7592592592592593004, 0.7638888888888889506 ),
 .UNSPECIFIED. ) 
 CURVE ( )  GEOMETRIC_REPRESENTATION_ITEM ( )  RATIONAL_B_SPLINE_CURVE ( ( 0.9330127018922192983, 0.9330127018922200755, 1.000000000000000000, 0.8660254037844387076, 1.000000000000000000, 0.8660254037844387076, 1.000000000000000000, 0.9330127018922185211, 0.9330127018922192983 ) ) 
 REPRESENTATION_ITEM ( '' )  );
#32858 = CARTESIAN_POINT ( 'NONE',  ( 24.81562500061451715, 3.027376345333611329, 5.243569643749999010 ) ) ;
#32859 = CARTESIAN_POINT ( 'NONE',  ( 5.090625000614516615, -3.027376345333614438, 5.243569643749998122 ) ) ;
#32860 = EDGE_LOOP ( 'NONE', ( #10097, #66465, #46663, #19637 ) ) ;
#32861 = CARTESIAN_POINT ( 'NONE',  ( 29.69999999999999574, -4.330127018922190985, -2.500000000000001332 ) ) ;
#32862 = CARTESIAN_POINT ( 'NONE',  ( 4.003125000614518925, 4.541064518000418104, -2.621784821874998173 ) ) ;
#32863 = CARTESIAN_POINT ( 'NONE',  ( 12.08437500061451608, 5.824947211148865298E-16, -4.756430356249998326 ) ) ;
#32864 = CARTESIAN_POINT ( 'NONE',  ( 4.000000000000000000, 12.98749999999999893, 32.30940107675849760 ) ) ;
#32865 = CARTESIAN_POINT ( 'NONE',  ( -3.999999999999999112, 14.26250000122903572, -30.00000000000000000 ) ) ;
#32866 = CARTESIAN_POINT ( 'NONE',  ( -2.121784821874999949, 18.43437500061451928, -33.67503911421598417 ) ) ;
#32867 = CARTESIAN_POINT ( 'NONE',  ( 10.08749999999999858, 5.773502691896255534, 3.535250795749688894E-16 ) ) ;
#32868 = CARTESIAN_POINT ( 'NONE',  ( 12.15937500061451892, 4.541064518000418104, -2.621784821874998173 ) ) ;
#32869 = CARTESIAN_POINT ( 'NONE',  ( 7.575000001229033053, 2.886751345948126879, 4.999999999999999112 ) ) ;
#32870 = CARTESIAN_POINT ( 'NONE',  ( 12.98437500061451821, 6.421520780324663323E-16, -5.243569643749999010 ) ) ;
#32871 = CARTESIAN_POINT ( 'NONE',  ( 6.946875000614517681, -3.027376345333614438, 5.243569643749998122 ) ) ;
#32872 = CARTESIAN_POINT ( 'NONE',  ( 16.94999999999999929, 0.000000000000000000, 4.999999999999998224 ) ) ;
#32873 = FACE_OUTER_BOUND ( 'NONE', #57085, .T. ) ;
#32874 = CARTESIAN_POINT ( 'NONE',  ( 9.571875000614518569, 3.027376345333611329, 5.243569643749999010 ) ) ;
#32875 = CARTESIAN_POINT ( 'NONE',  ( 20.50312500061451715, -4.541064518000417216, -2.621784821875001281 ) ) ;
#32876 = CARTESIAN_POINT ( 'NONE',  ( 19.50000000000000000, 4.330127018922192761, -2.499999999999997780 ) ) ;
#32877 = CARTESIAN_POINT ( 'NONE',  ( -4.243569643749999898, 19.76562500061459104, 27.54997392385601529 ) ) ;
#32878 = CARTESIAN_POINT ( 'NONE',  ( 24.27187500061452141, 3.027376345333613106, -5.243569643749998122 ) ) ;
#32879 = FACE_OUTER_BOUND ( 'NONE', #10039, .T. ) ;
#32880 = CARTESIAN_POINT ( 'NONE',  ( 28.46250000122903145, -4.330127018922190985, -2.500000000000001332 ) ) ;
#32881 = CARTESIAN_POINT ( 'NONE',  ( 20.59687500061451715, 4.119189519843966529, -2.378215178124998275 ) ) ;
#32882 = CARTESIAN_POINT ( 'NONE',  ( 25.60312500061451502, 4.541064518000418104, -2.621784821874998173 ) ) ;
#32883 = CARTESIAN_POINT ( 'NONE',  ( 16.94062500061451715, -3.027376345333610441, -5.243569643749999898 ) ) ;
#32884 = CARTESIAN_POINT ( 'NONE',  ( 13.25625000122903074, 4.330127018922192761, -2.499999999999997780 ) ) ;
#32885 = CARTESIAN_POINT ( 'NONE',  ( 13.62187500061451750, 3.027376345333611329, 5.243569643749999010 ) ) ;
#32886 = CARTESIAN_POINT ( 'NONE',  ( 7.347880794884120722E-16, 20.00000000000000000, 36.00000000000000000 ) ) ;
#32887 = CARTESIAN_POINT ( 'NONE',  ( 26.85000000122903430, 5.773502691896255534, 3.535250795749688894E-16 ) ) ;
#32888 = CARTESIAN_POINT ( 'NONE',  ( 0.000000000000000000, 20.00000000000000000, 30.00000000000000000 ) ) ;
#32889 = CARTESIAN_POINT ( 'NONE',  ( 14.33437500061451786, 6.421520780324663323E-16, -5.243569643749999010 ) ) ;
#32890 = CARTESIAN_POINT ( 'NONE',  ( 15.03749999999999964, 5.773502691896255534, 3.535250795749688401E-16 ) ) ;
#32891 = CARTESIAN_POINT ( 'NONE',  ( 21.71249999999999858, 2.886751345948129099, -4.999999999999997335 ) ) ;
#32892 = CARTESIAN_POINT ( 'NONE',  ( 4.425000001229032698, 2.886751345948126879, 4.999999999999999112 ) ) ;
#32893 = CARTESIAN_POINT ( 'NONE',  ( 24.34687500061451715, 6.054752690667223547, 3.707466751127219781E-16 ) ) ;
#32894 = CARTESIAN_POINT ( 'NONE',  ( 17.14687500061451786, 6.054752690667223547, 3.707466751127219781E-16 ) ) ;
#32895 = CARTESIAN_POINT ( 'NONE',  ( -1.878215178125001827, 15.30312499938548321, 33.25316411605952283 ) ) ;
#32896 = CARTESIAN_POINT ( 'NONE',  ( 27.75000000000000000, 0.000000000000000000, 4.999999999999998224 ) ) ;
#32897 = CARTESIAN_POINT ( 'NONE',  ( 2.887500001229035274, 6.123233995736764310E-16, -4.999999999999998224 ) ) ;
#32898 = CARTESIAN_POINT ( 'NONE',  ( 6.112499999999999822, 2.886751345948126879, 4.999999999999999112 ) ) ;
#32899 = CARTESIAN_POINT ( 'NONE',  ( 28.43437500061451573, 4.119189519843966529, 2.378215178124999607 ) ) ;
#32900 = CARTESIAN_POINT ( 'NONE',  ( 19.71562500061451928, 3.027376345333613106, -5.243569643749998122 ) ) ;
#32901 = CARTESIAN_POINT ( 'NONE',  ( 9.825000000000001066, -4.330127018922194537, 2.499999999999995559 ) ) ;
#32902 = EDGE_CURVE ( 'NONE', #70914, #68959, #65954, .T. ) ;
#32903 = CARTESIAN_POINT ( 'NONE',  ( 4.753125000614515372, -4.541064518000417216, -2.621784821875001281 ) ) ;
#32904 =( BOUNDED_CURVE ( )  B_SPLINE_CURVE ( 2, ( #24524, #57051, #6819, #17880, #46710, #68163, #63680, #52246, #6457 ),
 .UNSPECIFIED., .F., .F. ) 
 B_SPLINE_CURVE_WITH_KNOTS ( ( 3, 2, 2, 2, 3 ),
 ( 0.4021739130434782705, 0.4057971014492753881, 0.4130434782608695676, 0.4202898550724637472, 0.4239130434782608647 ),
 .UNSPECIFIED. ) 
 CURVE ( )  GEOMETRIC_REPRESENTATION_ITEM ( )  RATIONAL_B_SPLINE_CURVE ( ( 0.9330127018922194093, 0.9330127018922194093, 1.000000000000000000, 0.8660254037844387076, 1.000000000000000000, 0.8660254037844387076, 1.000000000000000000, 0.9330127018922194093, 0.9330127018922194093 ) ) 
 REPRESENTATION_ITEM ( '' )  );
#32905 = CARTESIAN_POINT ( 'NONE',  ( 17.17500000000000071, 6.123233995736764310E-16, -4.999999999999998224 ) ) ;
#32906 = CARTESIAN_POINT ( 'NONE',  ( 15.67500000122903359, 2.886751345948060266, 5.000000000000114575 ) ) ;
#32907 = CARTESIAN_POINT ( 'NONE',  ( 20.77500000122903145, -5.773502691896255534, -1.060575238724906372E-15 ) ) ;
#32908 = FACE_OUTER_BOUND ( 'NONE', #5989, .T. ) ;
#32909 = CARTESIAN_POINT ( 'NONE',  ( 28.69687500061451502, -3.027376345333610441, -5.243569643749999898 ) ) ;
#32910 = EDGE_LOOP ( 'NONE', ( #37934, #56952, #72288, #27552 ) ) ;
#32911 = CARTESIAN_POINT ( 'NONE',  ( 16.22812500061451857, 4.541064518000418104, 2.621784821874999949 ) ) ;
#32912 = CARTESIAN_POINT ( 'NONE',  ( 25.22812500061451502, 4.541064518000418104, 2.621784821874999949 ) ) ;
#32913 = CARTESIAN_POINT ( 'NONE',  ( 21.87187500061451573, -6.054752690667223547, -1.112240025338166033E-15 ) ) ;
#32914 = CARTESIAN_POINT ( 'NONE',  ( 7.237500000000000711, -2.886751345948125991, -5.000000000000000000 ) ) ;
#32915 = CARTESIAN_POINT ( 'NONE',  ( 10.56562500061451715, -6.054752690667223547, -1.112240025338166033E-15 ) ) ;
#32916 = CARTESIAN_POINT ( 'NONE',  ( 27.74062500061451431, -3.027376345333610441, -5.243569643749999898 ) ) ;
#32917 = CARTESIAN_POINT ( 'NONE',  ( 14.48437500061451821, 4.541064518000418104, 2.621784821874999949 ) ) ;
#32918 = CARTESIAN_POINT ( 'NONE',  ( 19.17187500061451999, -6.054752690667223547, -1.112240025338166033E-15 ) ) ;
#32919 = CARTESIAN_POINT ( 'NONE',  ( 4.000000000000000000, 11.75000000122903643, -27.69059892324149885 ) ) ;
#32920 = CARTESIAN_POINT ( 'NONE',  ( 4.243569643749999898, 10.14687500061451786, 32.45002607614398471 ) ) ;
#32921 = CARTESIAN_POINT ( 'NONE',  ( 21.97500000122903074, 2.886751345948126879, 4.999999999999999112 ) ) ;
#32922 = CARTESIAN_POINT ( 'NONE',  ( 16.95937500061451786, -4.119189519843965641, -2.378215178125001383 ) ) ;
#32923 = CARTESIAN_POINT ( 'NONE',  ( 11.12812500061451715, 6.421520780324663323E-16, -5.243569643749999010 ) ) ;
#32924 = CARTESIAN_POINT ( 'NONE',  ( 7.959375000614516971, -4.541064518000417216, -2.621784821875001281 ) ) ;
#32925 = CARTESIAN_POINT ( 'NONE',  ( 7.134375000614516793, 6.421520780324663323E-16, -5.243569643749999010 ) ) ;
#32926 = ORIENTED_EDGE ( 'NONE', *, *, #71109, .F. ) ;
#32927 = CARTESIAN_POINT ( 'NONE',  ( 28.54687500061451644, -3.027376345333614438, 5.243569643749998122 ) ) ;
#32928 = CARTESIAN_POINT ( 'NONE',  ( 19.37812500061451715, 4.541064518000418104, 2.621784821874999949 ) ) ;
#32929 = CARTESIAN_POINT ( 'NONE',  ( 28.53750000122903074, 6.123233995736764310E-16, -4.999999999999998224 ) ) ;
#32930 = CARTESIAN_POINT ( 'NONE',  ( 3.759375000614517681, 0.000000000000000000, 5.243569643749999010 ) ) ;
#32931 = CARTESIAN_POINT ( 'NONE',  ( 24.49687500061451573, -3.027376345333614438, 5.243569643749998122 ) ) ;
#32932 = CARTESIAN_POINT ( 'NONE',  ( 20.42812500061451431, -4.541064518000419881, 2.621784821874995952 ) ) ;
#32933 = CARTESIAN_POINT ( 'NONE',  ( 4.243569643749999898, 18.69687500061451857, 32.45002607614398471 ) ) ;
#32934 = CARTESIAN_POINT ( 'NONE',  ( 23.84062500061451928, 6.054752690667223547, 3.707466751127219781E-16 ) ) ;
#32935 = CARTESIAN_POINT ( 'NONE',  ( 3.675000001229035362, -5.773502691896255534, -1.060575238724906372E-15 ) ) ;
#32936 = VERTEX_POINT ( 'NONE', #55603 ) ;
#32937 = CARTESIAN_POINT ( 'NONE',  ( 4.465851277537014496, 2.248593419656078840, -4.736966354317482697 ) ) ;
#32938 = CARTESIAN_POINT ( 'NONE',  ( -2.000000000000000000, 15.42500000000000071, -33.46410161513775705 ) ) ;
#32939 = CARTESIAN_POINT ( 'NONE',  ( 1.878215178124997609, 16.72812499938548214, 33.25316411605952993 ) ) ;
#32940 = CARTESIAN_POINT ( 'NONE',  ( 4.134375000614517681, 4.541064518000418104, 2.621784821874999949 ) ) ;
#32941 = CARTESIAN_POINT ( 'NONE',  ( 11.72812500061451857, 4.541064518000418104, 2.621784821874999949 ) ) ;
#32942 = CARTESIAN_POINT ( 'NONE',  ( 7.021875000614518747, -6.054752690667223547, -1.112240025338166033E-15 ) ) ;
#32943 = CARTESIAN_POINT ( 'NONE',  ( 25.46250000122903501, 4.330127018922192761, -2.499999999999997780 ) ) ;
#32944 = CARTESIAN_POINT ( 'NONE',  ( 15.53437500061451715, -4.541064518000419881, 2.621784821874995952 ) ) ;
#32945 = CARTESIAN_POINT ( 'NONE',  ( 28.45312500061451289, 0.000000000000000000, 5.243569643749999010 ) ) ;
#32946 = CARTESIAN_POINT ( 'NONE',  ( 29.09999999999999787, 0.000000000000000000, 4.999999999999998224 ) ) ;
#32947 = CARTESIAN_POINT ( 'NONE',  ( 25.77187500061451075, 3.027376345333611329, 5.243569643749999010 ) ) ;
#32948 = CARTESIAN_POINT ( 'NONE',  ( 14.32500000000000107, -4.330127018922194537, 2.499999999999995559 ) ) ;
#32949 = CARTESIAN_POINT ( 'NONE',  ( 12.81562500061451537, -6.054752690667223547, -1.112240025338166033E-15 ) ) ;
#32950 = ORIENTED_EDGE ( 'NONE', *, *, #9558, .F. ) ;
#32951 = CARTESIAN_POINT ( 'NONE',  ( 10.90312500061451928, 0.000000000000000000, 5.243569643749999010 ) ) ;
#32952 = CARTESIAN_POINT ( 'NONE',  ( 8.840625000614515727, -3.027376345333610441, -5.243569643749999898 ) ) ;
#32953 = CARTESIAN_POINT ( 'NONE',  ( 19.24687500061452283, -2.746126346562642428, -4.756430356249999214 ) ) ;
#32954 = CARTESIAN_POINT ( 'NONE',  ( 9.637499999999999289, 5.773502691896255534, 3.535250795749688894E-16 ) ) ;
#32955 = EDGE_CURVE ( 'NONE', #61789, #51427, #11764, .T. ) ;
#32956 = CARTESIAN_POINT ( 'NONE',  ( 3.037500001229032964, 4.330127018922191873, 2.499999999999999556 ) ) ;
#32957 = CARTESIAN_POINT ( 'NONE',  ( 17.25000000000000000, 4.330127018922192761, -2.499999999999997780 ) ) ;
#32958 = CARTESIAN_POINT ( 'NONE',  ( 18.72187500061451360, -6.054752690667223547, -1.112240025338166033E-15 ) ) ;
#32959 = CARTESIAN_POINT ( 'NONE',  ( 14.77500000122903501, 2.886751345948126879, 4.999999999999999112 ) ) ;
#32960 = CARTESIAN_POINT ( 'NONE',  ( 20.62499999999999645, -4.330127018922194537, 2.499999999999995559 ) ) ;
#32961 = CARTESIAN_POINT ( 'NONE',  ( -4.243569643749999898, 15.75312500061451537, -30.00000000000000000 ) ) ;
#32962 = CARTESIAN_POINT ( 'NONE',  ( 17.28750000122903430, 6.123233995736764310E-16, -4.999999999999998224 ) ) ;
#32963 = CARTESIAN_POINT ( 'NONE',  ( 29.46562500061451573, -6.054752690667223547, -1.112240025338166033E-15 ) ) ;
#32964 = DIRECTION ( 'NONE',  ( 0.000000000000000000, 0.000000000000000000, 1.000000000000000000 ) ) ;
#32965 = CARTESIAN_POINT ( 'NONE',  ( 17.58749999999999858, -2.886751345948070480, -5.000000000000095923 ) ) ;
#32966 = CARTESIAN_POINT ( 'NONE',  ( 12.79687500061451821, -3.027376345333614438, 5.243569643749998122 ) ) ;
#32967 = CARTESIAN_POINT ( 'NONE',  ( 25.98750000000000071, -2.886751345948129988, 4.999999999999997335 ) ) ;
#32968 = CARTESIAN_POINT ( 'NONE',  ( 8.878125000614515372, 6.421520780324663323E-16, -5.243569643749999010 ) ) ;
#32969 = CARTESIAN_POINT ( 'NONE',  ( 27.53437500061451715, -2.746126346562646425, 4.756430356249996549 ) ) ;
#32970 = CARTESIAN_POINT ( 'NONE',  ( 20.85937500061451644, 0.000000000000000000, 5.243569643749999010 ) ) ;
#32971 = CARTESIAN_POINT ( 'NONE',  ( 12.60937500061451289, 2.746126346562643317, 4.756430356249998326 ) ) ;
#32972 = CARTESIAN_POINT ( 'NONE',  ( 7.265625000614516438, 3.027376345333611329, 5.243569643749999010 ) ) ;
#32973 = CARTESIAN_POINT ( 'NONE',  ( 9.834375000614517859, 6.421520780324663323E-16, -5.243569643749999010 ) ) ;
#32974 = VERTEX_POINT ( 'NONE', #26064 ) ;
#32975 = CARTESIAN_POINT ( 'NONE',  ( 20.97187500061451715, -6.054752690667223547, -1.112240025338166033E-15 ) ) ;
#32976 = CARTESIAN_POINT ( 'NONE',  ( 3.859048791629765773, 3.180512981247727300, -31.08635514026660474 ) ) ;
#32977 = CARTESIAN_POINT ( 'NONE',  ( 17.23125000122903572, 6.123233995736764310E-16, -4.999999999999998224 ) ) ;
#32978 = CARTESIAN_POINT ( 'NONE',  ( 4.349999999999999645, 0.000000000000000000, 4.999999999999998224 ) ) ;
#32979 = CARTESIAN_POINT ( 'NONE',  ( 14.62500000122903288, 2.886751345948129099, -4.999999999999998224 ) ) ;
#32980 = CARTESIAN_POINT ( 'NONE',  ( 45.00000000000000000, 0.000000000000000000, 0.000000000000000000 ) ) ;
#32981 = CARTESIAN_POINT ( 'NONE',  ( 18.56250000000000000, 2.886751345948129099, -4.999999999999997335 ) ) ;
#32982 = ORIENTED_EDGE ( 'NONE', *, *, #17622, .T. ) ;
#32983 = CARTESIAN_POINT ( 'NONE',  ( 12.00000000000000000, 0.000000000000000000, 4.999999999999998224 ) ) ;
#32984 = CARTESIAN_POINT ( 'NONE',  ( 16.76249999999999929, 2.886751345948129099, -4.999999999999998224 ) ) ;
#32985 = CARTESIAN_POINT ( 'NONE',  ( 12.56250000122903465, 0.000000000000000000, 4.999999999999998224 ) ) ;
#32986 = CARTESIAN_POINT ( 'NONE',  ( 10.52812500061451750, -4.541064518000419881, 2.621784821874995952 ) ) ;
#32987 = ORIENTED_EDGE ( 'NONE', *, *, #42238, .F. ) ;
#32988 = CARTESIAN_POINT ( 'NONE',  ( 9.862500000000000711, -5.773502691896255534, -1.060575238724906372E-15 ) ) ;
#32989 = CARTESIAN_POINT ( 'NONE',  ( 18.45000000122903216, -2.886751345948096681, 5.000000000000054179 ) ) ;
#32990 = CARTESIAN_POINT ( 'NONE',  ( 2.121784821875001281, 14.15937500061451715, -26.32496088578401938 ) ) ;
#32991 = CARTESIAN_POINT ( 'NONE',  ( 3.590625000614518836, 6.054752690667223547, 3.707466751127219781E-16 ) ) ;
#32992 = CARTESIAN_POINT ( 'NONE',  ( 1.878215178125000495, 14.51562499938548356, 26.74683588394047007 ) ) ;
#32993 = CARTESIAN_POINT ( 'NONE',  ( 8.925000000000002487, -4.330127018922194537, 2.499999999999995559 ) ) ;
#32994 = CARTESIAN_POINT ( 'NONE',  ( 3.900000001229035451, 5.773502691896255534, 3.535250795749688401E-16 ) ) ;
#32995 = ORIENTED_EDGE ( 'NONE', *, *, #33946, .T. ) ;
#32996 = CARTESIAN_POINT ( 'NONE',  ( 24.96562500061451573, -6.054752690667223547, -1.112240025338166033E-15 ) ) ;
#32997 = CARTESIAN_POINT ( 'NONE',  ( 1.071796769724489895, 13.56740381056766687, -34.00000000000000000 ) ) ;
#32998 = CARTESIAN_POINT ( 'NONE',  ( -1.878215178124999163, 20.44062499938548072, 26.74683588394047007 ) ) ;
#32999 = CARTESIAN_POINT ( 'NONE',  ( 21.79687500061451644, -3.027376345333614438, 5.243569643749998122 ) ) ;
#33000 = CARTESIAN_POINT ( 'NONE',  ( 16.75312500061451715, 0.000000000000000000, 5.243569643749999010 ) ) ;
#33001 = CARTESIAN_POINT ( 'NONE',  ( -4.243569643749999898, 12.15312500061459389, -30.00000000000000000 ) ) ;
#33002 = CARTESIAN_POINT ( 'NONE',  ( 5.878125000614517148, 4.541064518000418104, 2.621784821874999949 ) ) ;
#33003 = CARTESIAN_POINT ( 'NONE',  ( 28.76250000122903216, 0.000000000000000000, 4.999999999999998224 ) ) ;
#33004 = CARTESIAN_POINT ( 'NONE',  ( 24.53437500061451715, -4.119189519843968306, 2.378215178124996054 ) ) ;
#33005 = CARTESIAN_POINT ( 'NONE',  ( 20.24062500061451786, 6.054752690667223547, 3.707466751127219781E-16 ) ) ;
#33006 = CARTESIAN_POINT ( 'NONE',  ( 8.259375000614518569, 0.000000000000000000, 4.756430356249998326 ) ) ;
#33007 = CARTESIAN_POINT ( 'NONE',  ( 3.756430356250000102, 18.04062499938548214, 30.00000000000000000 ) ) ;
#33008 = CARTESIAN_POINT ( 'NONE',  ( 14.18437500061451750, -4.541064518000419881, 2.621784821874995952 ) ) ;
#33009 = CARTESIAN_POINT ( 'NONE',  ( 13.99687500061451928, 6.054752690667223547, 3.707466751127219781E-16 ) ) ;
#33010 = CARTESIAN_POINT ( 'NONE',  ( 21.79687500061451644, -3.027376345333614438, 5.243569643749998122 ) ) ;
#33011 = ORIENTED_EDGE ( 'NONE', *, *, #32685, .F. ) ;
#33012 = CARTESIAN_POINT ( 'NONE',  ( 4.243569643749999010, 12.02187500061451786, 27.54997392385601174 ) ) ;
#33013 = CARTESIAN_POINT ( 'NONE',  ( 3.628125000614518036, 4.541064518000418104, 2.621784821874999949 ) ) ;
#33014 = CARTESIAN_POINT ( 'NONE',  ( 25.75312500061451715, 0.000000000000000000, 5.243569643749999010 ) ) ;
#33015 = CARTESIAN_POINT ( 'NONE',  ( 26.65312500061451573, 0.000000000000000000, 5.243569643749999010 ) ) ;
#33016 = CYLINDRICAL_SURFACE ( 'NONE', #17135, 4.999999999999998224 ) ;
#33017 = CARTESIAN_POINT ( 'NONE',  ( 3.999999999999999112, 18.42500000000000071, 30.00000000000000000 ) ) ;
#33018 = CARTESIAN_POINT ( 'NONE',  ( 5.821875000614519458, 3.027376345333613106, -5.243569643749998122 ) ) ;
#33019 = CONTEXT_DEPENDENT_SHAPE_REPRESENTATION ( #15313, #4319 ) ;
#33020 = CARTESIAN_POINT ( 'NONE',  ( 12.90000000122903145, 5.773502691896255534, 3.535250795749688894E-16 ) ) ;
#33021 = CARTESIAN_POINT ( 'NONE',  ( 8.250000001229034652, -2.886751345948125991, -5.000000000000000000 ) ) ;
#33022 = CARTESIAN_POINT ( 'NONE',  ( 2.915625000614516793, -6.054752690667223547, -1.112240025338166033E-15 ) ) ;
#33023 = CARTESIAN_POINT ( 'NONE',  ( -3.999999999999999556, 15.78124999877096535, 27.69059892324149175 ) ) ;
#33024 = CARTESIAN_POINT ( 'NONE',  ( 19.81875000122903430, -5.773502691896255534, -1.060575238724906372E-15 ) ) ;
#33025 = CARTESIAN_POINT ( 'NONE',  ( 11.89687500061451608, -3.027376345333614438, 5.243569643749998122 ) ) ;
#33026 = CARTESIAN_POINT ( 'NONE',  ( 0.000000000000000000, 27.50000000000000000, 30.00000000000000000 ) ) ;
#33027 = ORIENTED_EDGE ( 'NONE', *, *, #56499, .F. ) ;
#33028 = CARTESIAN_POINT ( 'NONE',  ( 20.95312500061451999, -4.541064518000417216, -2.621784821875001281 ) ) ;
#33029 = CARTESIAN_POINT ( 'NONE',  ( 12.72187500061451537, 3.027376345333611329, 5.243569643749999010 ) ) ;
#33030 = CARTESIAN_POINT ( 'NONE',  ( 5.465625000614517504, 3.027376345333611329, 5.243569643749999010 ) ) ;
#33031 = CARTESIAN_POINT ( 'NONE',  ( 22.62187500061451573, 3.027376345333611329, 5.243569643749999010 ) ) ;
#33032 = CARTESIAN_POINT ( 'NONE',  ( 5.465625000614517504, 3.027376345333611329, 5.243569643749999010 ) ) ;
#33033 = CARTESIAN_POINT ( 'NONE',  ( 6.637500001229035718, 4.330127018922191873, 2.499999999999999556 ) ) ;
#33034 = CARTESIAN_POINT ( 'NONE',  ( 6.675000001229034474, 2.886751345948126879, 4.999999999999999112 ) ) ;
#33035 = CARTESIAN_POINT ( 'NONE',  ( 20.31562500061451715, 3.027376345333611329, 5.243569643749999010 ) ) ;
#33036 = CARTESIAN_POINT ( 'NONE',  ( 2.000000000000001332, 17.56250000122903288, -26.53589838486224650 ) ) ;
#33037 = CARTESIAN_POINT ( 'NONE',  ( 7.912500001229033408, 4.330127018922192761, -2.499999999999997780 ) ) ;
#33038 = CARTESIAN_POINT ( 'NONE',  ( 16.37812500061451715, -4.541064518000419881, 2.621784821874995952 ) ) ;
#33039 = CARTESIAN_POINT ( 'NONE',  ( 14.80312500061451608, 4.541064518000418104, -2.621784821874998173 ) ) ;
#33040 = CARTESIAN_POINT ( 'NONE',  ( 26.37187500061451217, -5.492252693125287522, -1.008910452111647106E-15 ) ) ;
#33041 = CARTESIAN_POINT ( 'NONE',  ( 15.75000000000000000, -4.330127018922190985, -2.500000000000001332 ) ) ;
#33042 = CARTESIAN_POINT ( 'NONE',  ( 12.48750000122903359, 4.330127018922191873, 2.499999999999999556 ) ) ;
#33043 = CARTESIAN_POINT ( 'NONE',  ( 8.353125000614518569, -4.541064518000417216, -2.621784821875001281 ) ) ;
#33044 = CARTESIAN_POINT ( 'NONE',  ( 10.64062500061451644, -3.027376345333610441, -5.243569643749999898 ) ) ;
#33045 = EDGE_CURVE ( 'NONE', #49855, #5101, #4226, .T. ) ;
#33046 = CARTESIAN_POINT ( 'NONE',  ( 21.67500000122903359, -5.773502691896255534, -1.060575238724906372E-15 ) ) ;
#33047 = CARTESIAN_POINT ( 'NONE',  ( -4.243569643749999898, 12.65937500061451715, -30.00000000000000000 ) ) ;
#33048 = DIRECTION ( 'NONE',  ( -0.000000000000000000, -1.000000000000000000, -0.000000000000000000 ) ) ;
#33049 = CARTESIAN_POINT ( 'NONE',  ( 4.537500001229034297, -4.330127018922194537, 2.499999999999995559 ) ) ;
#33050 = CARTESIAN_POINT ( 'NONE',  ( 3.796875000614517326, -3.027376345333614438, 5.243569643749998122 ) ) ;
#33051 = CARTESIAN_POINT ( 'NONE',  ( 20.89687500061452141, -3.027376345333614438, 5.243569643749998122 ) ) ;
#33052 =( BOUNDED_CURVE ( )  B_SPLINE_CURVE ( 2, ( #54146, #10172, #25699, #60766, #14238, #60030, #71501, #54872, #48235 ),
 .UNSPECIFIED., .F., .F. ) 
 B_SPLINE_CURVE_WITH_KNOTS ( ( 3, 2, 2, 2, 3 ),
 ( 0.8586956521739130821, 0.8623188405797101996, 0.8695652173913043237, 0.8768115942028985588, 0.8804347826086956763 ),
 .UNSPECIFIED. ) 
 CURVE ( )  GEOMETRIC_REPRESENTATION_ITEM ( )  RATIONAL_B_SPLINE_CURVE ( ( 0.9330127018922194093, 0.9330127018922194093, 1.000000000000000000, 0.8660254037844387076, 1.000000000000000000, 0.8660254037844387076, 1.000000000000000000, 0.9330127018922194093, 0.9330127018922194093 ) ) 
 REPRESENTATION_ITEM ( '' )  );
#33053 = CARTESIAN_POINT ( 'NONE',  ( 16.71562500061451573, 3.027376345333611329, 5.243569643749999010 ) ) ;
#33054 = CARTESIAN_POINT ( 'NONE',  ( 11.15625000122903288, 0.000000000000000000, 4.999999999999998224 ) ) ;
#33055 = CARTESIAN_POINT ( 'NONE',  ( -3.999999999999997335, 15.53750000000000142, -27.69059892324149530 ) ) ;
#33056 = CARTESIAN_POINT ( 'NONE',  ( 14.08125000122903181, 6.123233995736764310E-16, -4.999999999999998224 ) ) ;
#33057 = CARTESIAN_POINT ( 'NONE',  ( 28.84687500061452070, 6.054752690667223547, 3.707466751127219781E-16 ) ) ;
#33058 = CARTESIAN_POINT ( 'NONE',  ( 19.77187500061451786, 4.119189519843966529, 2.378215178124999607 ) ) ;
#33059 = CARTESIAN_POINT ( 'NONE',  ( 14.39062500061451821, 6.054752690667223547, 3.707466751127219781E-16 ) ) ;
#33060 = CARTESIAN_POINT ( 'NONE',  ( 14.07187500061451679, 3.027376345333611329, 5.243569643749999010 ) ) ;
#33061 = ORIENTED_EDGE ( 'NONE', *, *, #15468, .T. ) ;
#33062 = CARTESIAN_POINT ( 'NONE',  ( 3.999999999999998668, 17.11250000000000071, -32.30940107675850470 ) ) ;
#33063 = CARTESIAN_POINT ( 'NONE',  ( 21.74062500061451431, -3.027376345333614438, 5.243569643749998122 ) ) ;
#33064 = CARTESIAN_POINT ( 'NONE',  ( -1.999999999999997113, 11.63750000122903394, -26.53589838486224295 ) ) ;
#33065 = CARTESIAN_POINT ( 'NONE',  ( 12.03749999999999964, -2.886751345948129988, 4.999999999999997335 ) ) ;
#33066 = CARTESIAN_POINT ( 'NONE',  ( 21.00000000122903288, 5.773502691896255534, 3.535250795749688894E-16 ) ) ;
#33067 = CARTESIAN_POINT ( 'NONE',  ( 16.60312500061451857, 4.541064518000418104, -2.621784821874998173 ) ) ;
#33068 = CARTESIAN_POINT ( 'NONE',  ( 11.89687500061451608, -4.119189519843965641, -2.378215178125001383 ) ) ;
#33069 = ORIENTED_EDGE ( 'NONE', *, *, #16136, .F. ) ;
#33070 = CARTESIAN_POINT ( 'NONE',  ( 21.11249999999999716, -5.773502691896255534, -1.060575238724906372E-15 ) ) ;
#33071 = CARTESIAN_POINT ( 'NONE',  ( 22.28437500061451715, -4.541064518000419881, 2.621784821874995952 ) ) ;
#33072 = CARTESIAN_POINT ( 'NONE',  ( 27.32812500061451644, 6.421520780324663323E-16, -5.243569643749999010 ) ) ;
#33073 = EDGE_CURVE ( 'NONE', #44824, #60913, #55245, .T. ) ;
#33074 = VERTEX_POINT ( 'NONE', #4640 ) ;
#33075 = CARTESIAN_POINT ( 'NONE',  ( 3.999999999999999112, 17.97500000000000142, -30.00000000000000000 ) ) ;
#33076 = CARTESIAN_POINT ( 'NONE',  ( 10.82812500061451644, 4.541064518000418104, 2.621784821874999949 ) ) ;
#33077 = CARTESIAN_POINT ( 'NONE',  ( 34.99999999999999289, 4.500000000000000888, -5.500000000000000888 ) ) ;
#33078 = CARTESIAN_POINT ( 'NONE',  ( 14.29687500061451644, 4.119189519843966529, -2.378215178124998275 ) ) ;
#33079 = CARTESIAN_POINT ( 'NONE',  ( 17.73750000000000071, 5.773502691896255534, 3.535250795749688894E-16 ) ) ;
#33080 = CARTESIAN_POINT ( 'NONE',  ( 24.71250000000000213, -5.773502691896255534, -1.060575238724906372E-15 ) ) ;
#33081 = CARTESIAN_POINT ( 'NONE',  ( 4.096875000614518925, 6.054752690667223547, 3.707466751127219781E-16 ) ) ;
#33082 = CARTESIAN_POINT ( 'NONE',  ( 27.98437500061451289, 4.541064518000418104, 2.621784821874999949 ) ) ;
#33083 = ORIENTED_EDGE ( 'NONE', *, *, #49669, .F. ) ;
#33084 = CARTESIAN_POINT ( 'NONE',  ( 26.99062500061451431, 6.054752690667223547, 3.707466751127219781E-16 ) ) ;
#33085 = CARTESIAN_POINT ( 'NONE',  ( 25.99687500061451928, -3.027376345333610441, -5.243569643749999898 ) ) ;
#33086 = CARTESIAN_POINT ( 'NONE',  ( -4.243569643749998122, 17.59062500061459389, -27.54997392385601174 ) ) ;
#33087 = CARTESIAN_POINT ( 'NONE',  ( 14.43750000000000000, -2.886751345948125991, -5.000000000000000000 ) ) ;
#33088 = CARTESIAN_POINT ( 'NONE',  ( 12.14062500061451821, 6.054752690667223547, 3.707466751127219781E-16 ) ) ;
#33089 = CARTESIAN_POINT ( 'NONE',  ( 4.000000000000000000, 17.43124999877096570, 27.69059892324149885 ) ) ;
#33090 = DIRECTION ( 'NONE',  ( 0.000000000000000000, 0.000000000000000000, -1.000000000000000000 ) ) ;
#33091 = CARTESIAN_POINT ( 'NONE',  ( 27.92812500061451431, 4.541064518000418104, 2.621784821874999949 ) ) ;
#33092 = CARTESIAN_POINT ( 'NONE',  ( 15.71250000122903501, 0.000000000000000000, 4.999999999999998224 ) ) ;
#33093 = CARTESIAN_POINT ( 'NONE',  ( 29.18437500061451217, 5.492252693125287522, 3.363034840372157021E-16 ) ) ;
#33094 = CARTESIAN_POINT ( 'NONE',  ( 15.64687500061451608, -2.746126346562642428, -4.756430356249999214 ) ) ;
#33095 = CARTESIAN_POINT ( 'NONE',  ( 5.728125000614515905, 6.421520780324663323E-16, -5.243569643749999010 ) ) ;
#33096 = CARTESIAN_POINT ( 'NONE',  ( 22.09687500061451715, 6.054752690667223547, 3.707466751127219781E-16 ) ) ;
#33097 = CARTESIAN_POINT ( 'NONE',  ( -2.121784821874999949, 13.93437500061451750, 26.32496088578401938 ) ) ;
#33098 = CARTESIAN_POINT ( 'NONE',  ( 22.58437500061451431, 4.541064518000418104, 2.621784821874999949 ) ) ;
#33099 = CARTESIAN_POINT ( 'NONE',  ( 3.487500000000000711, -2.886751345948129988, 4.999999999999997335 ) ) ;
#33100 = CARTESIAN_POINT ( 'NONE',  ( 4.243569643749999010, 19.22187500061452070, 27.54997392385601174 ) ) ;
#33101 = CARTESIAN_POINT ( 'NONE',  ( 8.840625000614515727, -3.027376345333610441, -5.243569643749999898 ) ) ;
#33102 = CARTESIAN_POINT ( 'NONE',  ( 1.999999999999998668, 17.26250000122903572, 26.53589838486224650 ) ) ;
#33103 = CARTESIAN_POINT ( 'NONE',  ( 6.646875000614518747, -3.027376345333610441, -5.243569643749999898 ) ) ;
#33104 = CARTESIAN_POINT ( 'NONE',  ( 13.10625000122903394, -4.330127018922190985, -2.500000000000001332 ) ) ;
#33105 = CARTESIAN_POINT ( 'NONE',  ( 8.615625000614517859, 3.027376345333611329, 5.243569643749999010 ) ) ;
#33106 = CARTESIAN_POINT ( 'NONE',  ( 13.17187500061451999, 3.027376345333611329, 5.243569643749999010 ) ) ;
#33107 = CARTESIAN_POINT ( 'NONE',  ( 21.54375000122902861, -2.886751345948130876, 4.999999999999996447 ) ) ;
#33108 = CARTESIAN_POINT ( 'NONE',  ( 19.83750000122903145, -4.330127018922194537, 2.499999999999995559 ) ) ;
#33109 = CARTESIAN_POINT ( 'NONE',  ( 7.696875000614516793, 6.054752690667223547, 3.707466751127219781E-16 ) ) ;
#33110 = CARTESIAN_POINT ( 'NONE',  ( 10.67812500061451608, 6.421520780324663323E-16, -5.243569643749999010 ) ) ;
#33111 = CARTESIAN_POINT ( 'NONE',  ( 6.290625000614517681, 6.054752690667223547, 3.707466751127219781E-16 ) ) ;
#33112 = CARTESIAN_POINT ( 'NONE',  ( 25.96875000122903288, 2.886751345948126879, 4.999999999999999112 ) ) ;
#33113 = CARTESIAN_POINT ( 'NONE',  ( 18.72187500061451360, -6.054752690667223547, -1.112240025338166033E-15 ) ) ;
#33114 = CARTESIAN_POINT ( 'NONE',  ( 4.500855584045652336, 2.177941268590406043, 4.634382331106658093 ) ) ;
#33116 = CARTESIAN_POINT ( 'NONE',  ( 12.40312500061451573, -4.541064518000417216, -2.621784821875001281 ) ) ;
#33115 =( BOUNDED_CURVE ( )  B_SPLINE_CURVE ( 2, ( #28764, #57192, #68664, #69027, #29494, #56829, #12138 ),
 .UNSPECIFIED., .F., .F. ) 
 B_SPLINE_CURVE_WITH_KNOTS ( ( 3, 2, 2, 3 ),
 ( 0.9341357058143047176, 0.9361111111111111160, 0.9388888888888888840, 0.9405958805770093800 ),
 .UNSPECIFIED. ) 
 CURVE ( )  GEOMETRIC_REPRESENTATION_ITEM ( )  RATIONAL_B_SPLINE_CURVE ( ( 0.9449585719455479982, 0.9047245142793810535, 1.000000000000000000, 0.8660254037844387076, 1.000000000000000000, 0.9176703320226651250, 0.9365266264699128040 ) ) 
 REPRESENTATION_ITEM ( '' )  );
#33117 = CARTESIAN_POINT ( 'NONE',  ( 28.32187500061451502, 3.027376345333612662, -5.243569643749998122 ) ) ;
#33118 = CARTESIAN_POINT ( 'NONE',  ( 4.243569643749999010, 12.02187500061451786, -32.45002607614398471 ) ) ;
#33119 = CARTESIAN_POINT ( 'NONE',  ( 12.07500000122903216, 2.886751345948126879, 4.999999999999999112 ) ) ;
#33120 = CARTESIAN_POINT ( 'NONE',  ( 4.243569643749999010, 14.21562500061451928, -32.45002607614398471 ) ) ;
#33121 = CARTESIAN_POINT ( 'NONE',  ( 14.13750000122903394, 6.123233995736764310E-16, -4.999999999999998224 ) ) ;
#33122 = CARTESIAN_POINT ( 'NONE',  ( 10.26562500061451644, 3.027376345333613106, -5.243569643749998122 ) ) ;
#33123 = ORIENTED_EDGE ( 'NONE', *, *, #28491, .F. ) ;
#33124 = CARTESIAN_POINT ( 'NONE',  ( 14.43750000000000000, -2.886751345948125991, -5.000000000000000000 ) ) ;
#33125 = FACE_OUTER_BOUND ( 'NONE', #64647, .T. ) ;
#33126 = CARTESIAN_POINT ( 'NONE',  ( 22.97812500061451857, 4.541064518000418104, 2.621784821874999949 ) ) ;
#33127 = CARTESIAN_POINT ( 'NONE',  ( 7.884375000614517681, -4.541064518000419881, 2.621784821874995952 ) ) ;
#33128 = CARTESIAN_POINT ( 'NONE',  ( 10.91250000122903252, -4.330127018922190985, -2.500000000000001332 ) ) ;
#33129 = CARTESIAN_POINT ( 'NONE',  ( 17.47500000122903430, 2.886751345948126879, 4.999999999999999112 ) ) ;
#33130 = CARTESIAN_POINT ( 'NONE',  ( 16.11562500061451786, 3.027376345333613106, -5.243569643749998122 ) ) ;
#33131 = CARTESIAN_POINT ( 'NONE',  ( 17.95312500061451644, 4.541064518000418104, -2.621784821874998173 ) ) ;
#33132 = CARTESIAN_POINT ( 'NONE',  ( 25.72500000122903074, -5.773502691896255534, -1.060575238724906372E-15 ) ) ;
#33133 =( BOUNDED_CURVE ( )  B_SPLINE_CURVE ( 2, ( #27281, #20619, #10285, #26547, #49446, #37258, #20989 ),
 .UNSPECIFIED., .F., .F. ) 
 B_SPLINE_CURVE_WITH_KNOTS ( ( 3, 2, 2, 3 ),
 ( 0.000000000000000000, 0.002777777777777771812, 0.005555555555555543625, 0.008333333333333315870 ),
 .UNSPECIFIED. ) 
 CURVE ( )  GEOMETRIC_REPRESENTATION_ITEM ( )  RATIONAL_B_SPLINE_CURVE ( ( 1.000000000000000000, 0.8660254037844387076, 1.000000000000000000, 0.8660254037844387076, 1.000000000000000000, 0.8660254037844395958, 0.9999999999999991118 ) ) 
 REPRESENTATION_ITEM ( '' )  );
#33134 = CARTESIAN_POINT ( 'NONE',  ( 27.67500000122903359, 2.886751345948129099, -4.999999999999998224 ) ) ;
#33135 = CARTESIAN_POINT ( 'NONE',  ( 21.75000000000000000, 4.330127018922192761, -2.499999999999997780 ) ) ;
#33136 = CARTESIAN_POINT ( 'NONE',  ( 3.756430356250000102, 13.99062499938548498, 30.00000000000000000 ) ) ;
#33137 = CARTESIAN_POINT ( 'NONE',  ( 25.43437500061451573, -4.541064518000419881, 2.621784821874995952 ) ) ;
#33138 = CARTESIAN_POINT ( 'NONE',  ( 25.72500000122903074, -5.773502691896255534, -1.060575238724906372E-15 ) ) ;
#33139 = CARTESIAN_POINT ( 'NONE',  ( 11.88750000122903216, 6.123233995736764310E-16, -4.999999999999998224 ) ) ;
#33140 = CARTESIAN_POINT ( 'NONE',  ( 28.24687500061451573, -3.027376345333610441, -5.243569643749999898 ) ) ;
#33141 = CARTESIAN_POINT ( 'NONE',  ( 22.68750000000000000, 5.773502691896255534, 3.535250795749688401E-16 ) ) ;
#33142 = CARTESIAN_POINT ( 'NONE',  ( 6.159375000614517148, -4.541064518000417216, -2.621784821875001281 ) ) ;
#33143 = CARTESIAN_POINT ( 'NONE',  ( 22.60312500061451857, 0.000000000000000000, 5.243569643749999010 ) ) ;
#33144 =( BOUNDED_CURVE ( )  B_SPLINE_CURVE ( 2, ( #46379, #18640, #53001, #41204, #63712, #53364, #30831 ),
 .UNSPECIFIED., .F., .F. ) 
 B_SPLINE_CURVE_WITH_KNOTS ( ( 3, 2, 2, 3 ),
 ( 0.08333333333333328707, 0.08611111111111106886, 0.08888888888888883677, 0.09166666666666660468 ),
 .UNSPECIFIED. ) 
 CURVE ( )  GEOMETRIC_REPRESENTATION_ITEM ( )  RATIONAL_B_SPLINE_CURVE ( ( 1.000000000000001998, 0.8660254037844365982, 1.000000000000000000, 0.8660254037844387076, 1.000000000000000000, 0.8660254037844413721, 0.9999999999999973355 ) ) 
 REPRESENTATION_ITEM ( '' )  );
#33145 = CARTESIAN_POINT ( 'NONE',  ( 2.655984681222220721E-16, 14.66562499938548214, 25.66244784525396483 ) ) ;
#33146 = CARTESIAN_POINT ( 'NONE',  ( 3.999999999999999112, 19.77500000000000213, -30.00000000000000000 ) ) ;
#33147 = CARTESIAN_POINT ( 'NONE',  ( 11.22187500061451892, 3.027376345333613106, -5.243569643749998122 ) ) ;
#33148 = CARTESIAN_POINT ( 'NONE',  ( 14.92500000000000071, 6.123233995736764310E-16, -4.999999999999998224 ) ) ;
#33149 = CARTESIAN_POINT ( 'NONE',  ( 3.159375000614518036, 4.541064518000418104, -2.621784821874998173 ) ) ;
#33150 = CARTESIAN_POINT ( 'NONE',  ( 5.671875000614519102, -6.054752690667223547, -1.112240025338166033E-15 ) ) ;
#33151 = CARTESIAN_POINT ( 'NONE',  ( 28.95937500061451431, 0.000000000000000000, 5.243569643749999010 ) ) ;
#33152 = CARTESIAN_POINT ( 'NONE',  ( -4.243569643749999898, 9.903125000614593887, 30.00000000000000000 ) ) ;
#33153 = CARTESIAN_POINT ( 'NONE',  ( 20.47500000000000142, 4.330127018922191873, 2.499999999999999556 ) ) ;
#33154 = VERTEX_POINT ( 'NONE', #20878 ) ;
#33155 = CARTESIAN_POINT ( 'NONE',  ( 26.62500000000000000, 6.123233995736764310E-16, -4.999999999999998224 ) ) ;
#33156 = CARTESIAN_POINT ( 'NONE',  ( 28.65937500061451715, -4.541064518000417216, -2.621784821875001281 ) ) ;
#33157 = EDGE_CURVE ( 'NONE', #25475, #40213, #23047, .T. ) ;
#33158 = ORIENTED_EDGE ( 'NONE', *, *, #65932, .F. ) ;
#33159 = CARTESIAN_POINT ( 'NONE',  ( 18.36562500061451431, 3.027376345333613106, -5.243569643749998122 ) ) ;
#33160 = CARTESIAN_POINT ( 'NONE',  ( 8.465625000614515727, 3.027376345333613106, -5.243569643749998122 ) ) ;
#33161 = CARTESIAN_POINT ( 'NONE',  ( 20.37187500061451217, -4.119189519843968306, 2.378215178124996054 ) ) ;
#33162 = CARTESIAN_POINT ( 'NONE',  ( 4.171875000614517326, 3.027376345333611329, 5.243569643749999010 ) ) ;
#33163 = CARTESIAN_POINT ( 'NONE',  ( 16.98750000122903359, 4.330127018922191873, 2.499999999999999556 ) ) ;
#33164 = CARTESIAN_POINT ( 'NONE',  ( 1.999999999999998668, 14.00000000000000178, -33.46410161513775705 ) ) ;
#33165 = CARTESIAN_POINT ( 'NONE',  ( 6.534375000614517148, -4.541064518000419881, 2.621784821874995952 ) ) ;
#33166 = CARTESIAN_POINT ( 'NONE',  ( 12.38437500061451857, -4.541064518000419881, 2.621784821874995952 ) ) ;
#33167 = CARTESIAN_POINT ( 'NONE',  ( 24.57187500061451502, -6.054752690667223547, -1.112240025338166033E-15 ) ) ;
#33168 = CARTESIAN_POINT ( 'NONE',  ( -3.999999999999999112, 14.60000000000000142, -30.00000000000000000 ) ) ;
#33169 = ORIENTED_EDGE ( 'NONE', *, *, #26658, .T. ) ;
#33170 = CARTESIAN_POINT ( 'NONE',  ( 10.49999999999999822, 4.330127018922192761, -2.499999999999997780 ) ) ;
#33171 = CARTESIAN_POINT ( 'NONE',  ( 16.80937500061451573, 0.000000000000000000, 5.243569643749999010 ) ) ;
#33172 = CARTESIAN_POINT ( 'NONE',  ( 10.17187500061451999, -6.054752690667223547, -1.112240025338166033E-15 ) ) ;
#33173 = CARTESIAN_POINT ( 'NONE',  ( -3.756430356250000102, 14.21562499938548285, 30.00000000000000000 ) ) ;
#33174 = CARTESIAN_POINT ( 'NONE',  ( 21.52499999999999858, -4.330127018922194537, 2.499999999999995559 ) ) ;
#33175 = CARTESIAN_POINT ( 'NONE',  ( -2.000000000000001776, 16.85000000000000142, 33.46410161513775705 ) ) ;
#33176 = DIRECTION ( 'NONE',  ( -0.000000000000000000, -1.000000000000000000, -0.000000000000000000 ) ) ;
#33177 = CARTESIAN_POINT ( 'NONE',  ( 21.42187500061451644, -5.492252693125287522, -1.008910452111647106E-15 ) ) ;
#33178 = CARTESIAN_POINT ( 'NONE',  ( 11.57812500061451644, 6.421520780324663323E-16, -5.243569643749999010 ) ) ;
#33179 = CARTESIAN_POINT ( 'NONE',  ( 29.85937500061451644, 0.000000000000000000, 5.243569643749999010 ) ) ;
#33180 = CARTESIAN_POINT ( 'NONE',  ( 28.33125000122903359, -4.330127018922194537, 2.499999999999995559 ) ) ;
#33181 = CARTESIAN_POINT ( 'NONE',  ( 29.78437500061451715, 4.541064518000418104, 2.621784821874999949 ) ) ;
#33182 = CARTESIAN_POINT ( 'NONE',  ( 9.862500000000000711, -5.773502691896255534, -1.060575238724906372E-15 ) ) ;
#33183 = CARTESIAN_POINT ( 'NONE',  ( -2.000000000000000000, 16.43750000122903643, 26.53589838486224650 ) ) ;
#33184 = CARTESIAN_POINT ( 'NONE',  ( 9.112500001229033586, -4.330127018922190985, -2.500000000000001332 ) ) ;
#33185 = CARTESIAN_POINT ( 'NONE',  ( 20.25937500061451857, 4.541064518000418104, -2.621784821874998173 ) ) ;
#33186 = CARTESIAN_POINT ( 'NONE',  ( 14.33437500061451786, 6.421520780324663323E-16, -5.243569643749999010 ) ) ;
#33187 = CARTESIAN_POINT ( 'NONE',  ( 9.375000001229036428, 2.886751345948126879, 4.999999999999998224 ) ) ;
#33188 = EDGE_LOOP ( 'NONE', ( #22481, #72317, #9721, #25720 ) ) ;
#33189 = CARTESIAN_POINT ( 'NONE',  ( 15.21562500061451750, 3.027376345333613106, -5.243569643749998122 ) ) ;
#33190 = CARTESIAN_POINT ( 'NONE',  ( 2.803125000614518747, 0.000000000000000000, 5.243569643749999010 ) ) ;
#33191 = CARTESIAN_POINT ( 'NONE',  ( 16.32187500061451502, 3.027376345333611329, 5.243569643749999010 ) ) ;
#33192 = CARTESIAN_POINT ( 'NONE',  ( 2.878125000614517592, -4.541064518000419881, 2.621784821874995952 ) ) ;
#33193 = CARTESIAN_POINT ( 'NONE',  ( 16.60312500061451857, 4.541064518000418104, -2.621784821874998173 ) ) ;
#33194 = CARTESIAN_POINT ( 'NONE',  ( 18.03750000122903430, -4.330127018922194537, 2.499999999999995559 ) ) ;
#33195 = CARTESIAN_POINT ( 'NONE',  ( 27.49687500061451217, 6.054752690667223547, 3.707466751127219781E-16 ) ) ;
#33196 = CARTESIAN_POINT ( 'NONE',  ( 4.243569643749999898, 10.12812500061451715, 30.00000000000000000 ) ) ;
#33197 = CARTESIAN_POINT ( 'NONE',  ( 15.79687500061451821, 6.054752690667223547, 3.707466751127219781E-16 ) ) ;
#33198 = CARTESIAN_POINT ( 'NONE',  ( 13.57500000122903572, -5.773502691896255534, -1.060575238724906372E-15 ) ) ;
#33199 = CARTESIAN_POINT ( 'NONE',  ( 9.121875000614517504, 2.746126346562643317, 4.756430356249998326 ) ) ;
#33200 = CARTESIAN_POINT ( 'NONE',  ( 9.001249775931846008E-16, 18.17187500061451999, -25.09994784771203058 ) ) ;
#33201 = CARTESIAN_POINT ( 'NONE',  ( 20.22187500061451715, 3.027376345333613106, -5.243569643749998122 ) ) ;
#33202 = CARTESIAN_POINT ( 'NONE',  ( 21.93750000122903288, 4.330127018922191873, 2.499999999999999556 ) ) ;
#33203 = CARTESIAN_POINT ( 'NONE',  ( 15.87187500061451573, 3.027376345333611329, 5.243569643749999010 ) ) ;
#33204 = CARTESIAN_POINT ( 'NONE',  ( -3.000416591977282496E-16, 12.54687500061451999, 25.09994784771203058 ) ) ;
#33205 = CARTESIAN_POINT ( 'NONE',  ( 17.65312500061451573, 0.000000000000000000, 5.243569643749999010 ) ) ;
#33206 = ORIENTED_EDGE ( 'NONE', *, *, #3605, .F. ) ;
#33207 = ORIENTED_EDGE ( 'NONE', *, *, #62697, .T. ) ;
#33208 = CARTESIAN_POINT ( 'NONE',  ( 20.99999999999999645, 0.000000000000000000, 4.999999999999998224 ) ) ;
#33209 = CARTESIAN_POINT ( 'NONE',  ( 17.47499999999999787, -4.330127018922194537, 2.499999999999995559 ) ) ;
#33210 = CARTESIAN_POINT ( 'NONE',  ( 23.91562500061451502, 3.027376345333611329, 5.243569643749999010 ) ) ;
#33211 = CARTESIAN_POINT ( 'NONE',  ( 4.453125000614517326, 4.541064518000418104, -2.621784821874998173 ) ) ;
#33212 = CARTESIAN_POINT ( 'NONE',  ( 17.70000000122903216, -2.886751345948125991, -5.000000000000000000 ) ) ;
#33213 = CARTESIAN_POINT ( 'NONE',  ( 22.11562500061451786, 3.027376345333611329, 5.243569643749999010 ) ) ;
#33214 = CARTESIAN_POINT ( 'NONE',  ( 19.91250000000000142, 2.886751345948129099, -4.999999999999998224 ) ) ;
#33215 = CARTESIAN_POINT ( 'NONE',  ( 25.30312500061451431, 0.000000000000000000, 5.243569643749999010 ) ) ;
#33216 = CARTESIAN_POINT ( 'NONE',  ( 6.890625000614516438, -3.027376345333614438, 5.243569643749998122 ) ) ;
#33217 = ORIENTED_EDGE ( 'NONE', *, *, #21308, .F. ) ;
#33218 = EDGE_CURVE ( 'NONE', #49981, #55550, #14553, .T. ) ;
#33219 = CARTESIAN_POINT ( 'NONE',  ( -3.999999999999999112, 20.28124999877096712, 27.69059892324149530 ) ) ;
#33220 = CARTESIAN_POINT ( 'NONE',  ( 3.178125000614515638, 4.541064518000418104, 2.621784821874999949 ) ) ;
#33221 = EDGE_CURVE ( 'NONE', #64403, #18194, #38984, .T. ) ;
#33222 = CARTESIAN_POINT ( 'NONE',  ( 12.68437500061451573, 4.119189519843966529, 2.378215178124999607 ) ) ;
#33223 = CARTESIAN_POINT ( 'NONE',  ( 1.999999999999998668, 18.95000000000000284, 26.53589838486224650 ) ) ;
#33224 = CARTESIAN_POINT ( 'NONE',  ( 3.999999999999999112, 10.88750000122903394, -30.00000000000000000 ) ) ;
#33225 = CARTESIAN_POINT ( 'NONE',  ( 2.121784821874999061, 17.45937500061451786, -33.67503911421598417 ) ) ;
#33226 = STYLED_ITEM ( 'NONE', ( #72638 ), #47954 ) ;
#33227 = CARTESIAN_POINT ( 'NONE',  ( 8.849999999999999645, 0.000000000000000000, 4.999999999999998224 ) ) ;
#33228 = EDGE_CURVE ( 'NONE', #14078, #4525, #16926, .T. ) ;
#33229 = CARTESIAN_POINT ( 'NONE',  ( 7.996875000614519280, -3.027376345333610441, -5.243569643749999898 ) ) ;
#33230 = CARTESIAN_POINT ( 'NONE',  ( 6.900000001229035007, -2.886751345948125991, -5.000000000000000000 ) ) ;
#33231 = CARTESIAN_POINT ( 'NONE',  ( 13.02187500061451608, 3.027376345333613106, -5.243569643749998122 ) ) ;
#33232 = CARTESIAN_POINT ( 'NONE',  ( 4.000000000000000000, 20.18750000000000000, 27.69059892324149885 ) ) ;
#33233 = CARTESIAN_POINT ( 'NONE',  ( 3.234375000614516438, 4.541064518000418104, 2.621784821874999949 ) ) ;
#33234 = CARTESIAN_POINT ( 'NONE',  ( 3.999999999999999112, 18.98750000122903359, 30.00000000000000000 ) ) ;
#33235 = CARTESIAN_POINT ( 'NONE',  ( 19.79999999999999716, -4.330127018922190985, -2.500000000000001332 ) ) ;
#33236 = EDGE_CURVE ( 'NONE', #46607, #59952, #24477, .T. ) ;
#33237 = CARTESIAN_POINT ( 'NONE',  ( 9.271875000614516082, -6.054752690667223547, -1.112240025338166033E-15 ) ) ;
#33238 = CARTESIAN_POINT ( 'NONE',  ( 20.99999999999999645, 0.000000000000000000, 4.999999999999998224 ) ) ;
#33239 = CARTESIAN_POINT ( 'NONE',  ( 20.57812500061451644, 6.421520780324663323E-16, -5.243569643749999010 ) ) ;
#33240 = CARTESIAN_POINT ( 'NONE',  ( 4.575000001229033053, -5.773502691896255534, -1.060575238724906372E-15 ) ) ;
#33241 = CARTESIAN_POINT ( 'NONE',  ( 2.121784821874999061, 16.05312500061459247, 26.32496088578401583 ) ) ;
#33242 = CARTESIAN_POINT ( 'NONE',  ( 23.67187500061451999, -6.054752690667223547, -1.112240025338166033E-15 ) ) ;
#33243 = CARTESIAN_POINT ( 'NONE',  ( 4.311958327294343363, 2.531208285321026263, 4.311958327294242999 ) ) ;
#33244 = CARTESIAN_POINT ( 'NONE',  ( 2.803125000614518747, 0.000000000000000000, 5.243569643749999010 ) ) ;
#33245 = CARTESIAN_POINT ( 'NONE',  ( 21.15937500061451715, 2.746126346562643317, 4.756430356249998326 ) ) ;
#33246 = CARTESIAN_POINT ( 'NONE',  ( 25.64062500061451644, 6.054752690667223547, 3.707466751127219781E-16 ) ) ;
#33247 = CARTESIAN_POINT ( 'NONE',  ( 16.64062500061451289, 6.054752690667223547, 3.707466751127219781E-16 ) ) ;
#33248 = CARTESIAN_POINT ( 'NONE',  ( 13.63125000122903252, 6.123233995736764310E-16, -4.999999999999998224 ) ) ;
#33249 = CARTESIAN_POINT ( 'NONE',  ( 15.19687500061451857, -3.027376345333610441, -5.243569643749999898 ) ) ;
#33250 = CARTESIAN_POINT ( 'NONE',  ( -4.000000000000000000, 15.87500000000000000, 30.00000000000000000 ) ) ;
#33251 = CARTESIAN_POINT ( 'NONE',  ( 25.87500000122903288, 2.886751345948129099, -4.999999999999998224 ) ) ;
#33252 = FACE_OUTER_BOUND ( 'NONE', #50582, .T. ) ;
#33253 = CARTESIAN_POINT ( 'NONE',  ( 13.24687500061451750, -3.027376345333614438, 5.243569643749998122 ) ) ;
#33254 = CARTESIAN_POINT ( 'NONE',  ( -1.999999999999997113, 11.97500000000000142, 33.46410161513775705 ) ) ;
#33255 = DIRECTION ( 'NONE',  ( 0.000000000000000000, 0.000000000000000000, 1.000000000000000000 ) ) ;
#33256 = CARTESIAN_POINT ( 'NONE',  ( -1.071796769724491005, 12.25759618943233775, -34.00000000000000000 ) ) ;
#33257 = CARTESIAN_POINT ( 'NONE',  ( 25.84687500061451360, -3.027376345333614438, 5.243569643749998122 ) ) ;
#33258 = CARTESIAN_POINT ( 'NONE',  ( 15.60937500061451644, -4.541064518000417216, -2.621784821875001281 ) ) ;
#33259 = CARTESIAN_POINT ( 'NONE',  ( -3.756430356250000102, 15.67812499938548143, 30.00000000000000000 ) ) ;
#33260 = CARTESIAN_POINT ( 'NONE',  ( 27.71250000000000568, 2.886751345948126879, 4.999999999999999112 ) ) ;
#33261 = CARTESIAN_POINT ( 'NONE',  ( 3.637500001229036162, -4.330127018922194537, 2.499999999999995559 ) ) ;
#33262 = CARTESIAN_POINT ( 'NONE',  ( 4.500000000000000888, -4.330127018922190985, -2.500000000000001332 ) ) ;
#33263 = CARTESIAN_POINT ( 'NONE',  ( 7.809375000614515727, -5.492252693125287522, -1.008910452111647106E-15 ) ) ;
#33264 = CARTESIAN_POINT ( 'NONE',  ( 19.79062500061451502, 6.054752690667223547, 3.707466751127219781E-16 ) ) ;
#33265 = CARTESIAN_POINT ( 'NONE',  ( 8.699999999999999289, 4.330127018922192761, -2.499999999999997780 ) ) ;
#33266 = DIRECTION ( 'NONE',  ( -0.000000000000000000, -1.000000000000000000, -0.000000000000000000 ) ) ;
#33267 = CARTESIAN_POINT ( 'NONE',  ( 17.73750000000000071, 5.773502691896255534, 3.535250795749688894E-16 ) ) ;
#33268 = DIRECTION ( 'NONE',  ( -1.000000000000000000, -0.000000000000000000, -0.000000000000000000 ) ) ;
#33269 = CARTESIAN_POINT ( 'NONE',  ( 20.06250000122903643, 4.330127018922192761, -2.499999999999997780 ) ) ;
#33270 = CARTESIAN_POINT ( 'NONE',  ( 2.692168354449049339, 9.632460402479559036, 35.36566372828262672 ) ) ;
#33271 = CARTESIAN_POINT ( 'NONE',  ( 27.27187500061451431, -6.054752690667223547, -1.112240025338166033E-15 ) ) ;
#33272 = VERTEX_POINT ( 'NONE', #50789 ) ;
#33273 = CARTESIAN_POINT ( 'NONE',  ( 17.65312500061451573, 0.000000000000000000, 5.243569643749999010 ) ) ;
#33274 = CARTESIAN_POINT ( 'NONE',  ( 23.50312500061451360, 0.000000000000000000, 5.243569643749999010 ) ) ;
#33275 = CARTESIAN_POINT ( 'NONE',  ( 23.40937500061451715, 4.541064518000418104, -2.621784821874998173 ) ) ;
#33276 = CARTESIAN_POINT ( 'NONE',  ( 5.700000000000000178, 0.000000000000000000, 4.999999999999998224 ) ) ;
#33277 = CARTESIAN_POINT ( 'NONE',  ( 8.803125000614517859, -4.541064518000417216, -2.621784821875001281 ) ) ;
#33278 = CARTESIAN_POINT ( 'NONE',  ( 24.59062500061451573, -3.027376345333610441, -5.243569643749999898 ) ) ;
#33279 = CARTESIAN_POINT ( 'NONE',  ( 15.87187500061451573, 3.027376345333611329, 5.243569643749999010 ) ) ;
#33280 = CARTESIAN_POINT ( 'NONE',  ( 20.22187500061451715, 3.027376345333613106, -5.243569643749998122 ) ) ;
#33281 = CARTESIAN_POINT ( 'NONE',  ( 4.243569643749999898, 11.04687500061451999, 32.45002607614398471 ) ) ;
#33282 = CARTESIAN_POINT ( 'NONE',  ( 20.70000000122903216, -2.886751345948129988, 4.999999999999997335 ) ) ;
#33283 = CARTESIAN_POINT ( 'NONE',  ( 16.39687500061451786, -2.746126346562646425, 4.756430356249996549 ) ) ;
#33284 = CARTESIAN_POINT ( 'NONE',  ( 11.99062500061451608, -3.027376345333610441, -5.243569643749999898 ) ) ;
#33285 = CARTESIAN_POINT ( 'NONE',  ( 8.709375000614517859, 0.000000000000000000, 5.243569643749999010 ) ) ;
#33286 = CARTESIAN_POINT ( 'NONE',  ( 6.346875000614517148, 6.054752690667223547, 3.707466751127219781E-16 ) ) ;
#33287 =( BOUNDED_CURVE ( )  B_SPLINE_CURVE ( 2, ( #48963, #20870, #4271, #64474, #65945, #32326, #27890, #183, #4631 ),
 .UNSPECIFIED., .F., .F. ) 
 B_SPLINE_CURVE_WITH_KNOTS ( ( 3, 2, 2, 2, 3 ),
 ( 0.2361111111111111049, 0.2407407407407407274, 0.2500000000000000000, 0.2592592592592592449, 0.2638888888888888951 ),
 .UNSPECIFIED. ) 
 CURVE ( )  GEOMETRIC_REPRESENTATION_ITEM ( )  RATIONAL_B_SPLINE_CURVE ( ( 0.9330127018922194093, 0.9330127018922194093, 1.000000000000000000, 0.8660254037844387076, 1.000000000000000000, 0.8660254037844387076, 1.000000000000000000, 0.9330127018922194093, 0.9330127018922194093 ) ) 
 REPRESENTATION_ITEM ( '' )  );
#33288 = ORIENTED_EDGE ( 'NONE', *, *, #1071, .F. ) ;
#33289 = CARTESIAN_POINT ( 'NONE',  ( 27.30937500061451573, -4.541064518000417216, -2.621784821875001281 ) ) ;
#33290 = CARTESIAN_POINT ( 'NONE',  ( 19.67812500061451786, 6.421520780324663323E-16, -5.243569643749999010 ) ) ;
#33291 = CARTESIAN_POINT ( 'NONE',  ( 29.51250000122903216, 4.330127018922192761, -2.499999999999997780 ) ) ;
#33292 = CARTESIAN_POINT ( 'NONE',  ( 28.64062500061451289, -3.027376345333610441, -5.243569643749999898 ) ) ;
#33293 = VECTOR ( 'NONE', #4951, 1000.000000000000000 ) ;
#33294 = CARTESIAN_POINT ( 'NONE',  ( 24.34687500061451715, 6.054752690667223547, 3.707466751127219781E-16 ) ) ;
#33295 = CARTESIAN_POINT ( 'NONE',  ( 19.82812500061451644, 4.541064518000418104, 2.621784821874999949 ) ) ;
#33296 = CARTESIAN_POINT ( 'NONE',  ( 2.000000000000001332, 10.25000000000000000, 33.46410161513774995 ) ) ;
#33297 = CARTESIAN_POINT ( 'NONE',  ( 24.66562500061451502, 3.027376345333613106, -5.243569643749998122 ) ) ;
#33298 = CARTESIAN_POINT ( 'NONE',  ( 5.250000001229035540, 5.773502691896255534, 3.535250795749688894E-16 ) ) ;
#33299 = ORIENTED_EDGE ( 'NONE', *, *, #36205, .T. ) ;
#33300 = CARTESIAN_POINT ( 'NONE',  ( 28.12499999999999645, 4.330127018922191873, 2.499999999999999556 ) ) ;
#33301 = CARTESIAN_POINT ( 'NONE',  ( 3.999999999999999112, 15.27500000000000036, -30.00000000000000000 ) ) ;
#33302 = CARTESIAN_POINT ( 'NONE',  ( -3.756430356250001434, 16.61562499938548143, 32.16877607737301048 ) ) ;
#33303 = CARTESIAN_POINT ( 'NONE',  ( 3.684375000614518836, 4.541064518000418104, 2.621784821874999949 ) ) ;
#33304 = CARTESIAN_POINT ( 'NONE',  ( 12.40312500061451573, -4.541064518000417216, -2.621784821875001281 ) ) ;
#33305 = CARTESIAN_POINT ( 'NONE',  ( 6.346875000614517148, 6.054752690667223547, 3.707466751127219781E-16 ) ) ;
#33306 = CARTESIAN_POINT ( 'NONE',  ( 24.03750000122903430, 6.123233995736764310E-16, -4.999999999999998224 ) ) ;
#33307 = CARTESIAN_POINT ( 'NONE',  ( 14.18437500061451750, -4.541064518000419881, 2.621784821874995952 ) ) ;
#33308 = CARTESIAN_POINT ( 'NONE',  ( 3.309375000614518836, 0.000000000000000000, 5.243569643749999010 ) ) ;
#33309 = CARTESIAN_POINT ( 'NONE',  ( 7.912500001229033408, 4.330127018922192761, -2.499999999999997780 ) ) ;
#33310 = CARTESIAN_POINT ( 'NONE',  ( 25.88437500061451502, -4.541064518000419881, 2.621784821874995952 ) ) ;
#33311 = CARTESIAN_POINT ( 'NONE',  ( 3.103125000614517237, 4.541064518000418104, -2.621784821874998173 ) ) ;
#33312 = CARTESIAN_POINT ( 'NONE',  ( 12.32812500061451821, -4.541064518000419881, 2.621784821874995952 ) ) ;
#33313 = ORIENTED_EDGE ( 'NONE', *, *, #2528, .T. ) ;
#33314 = CARTESIAN_POINT ( 'NONE',  ( 9.890625000614516438, 6.054752690667223547, 3.707466751127219781E-16 ) ) ;
#33315 = CARTESIAN_POINT ( 'NONE',  ( 8.915625000614515017, 3.027376345333613106, -5.243569643749998122 ) ) ;
#33316 = CARTESIAN_POINT ( 'NONE',  ( 19.80937500061451573, 4.119189519843966529, -2.378215178124998275 ) ) ;
#33317 = CARTESIAN_POINT ( 'NONE',  ( 2.775000001229033675, -5.773502691896255534, -1.060575238724906372E-15 ) ) ;
#33318 = CARTESIAN_POINT ( 'NONE',  ( 15.67500000000000071, -4.330127018922194537, 2.499999999999995559 ) ) ;
#33319 = EDGE_CURVE ( 'NONE', #58630, #20653, #34395, .T. ) ;
#33320 = CARTESIAN_POINT ( 'NONE',  ( 16.24687500061451573, 6.054752690667223547, 3.707466751127219781E-16 ) ) ;
#33321 = CARTESIAN_POINT ( 'NONE',  ( 12.93750000122903465, 4.330127018922191873, 2.499999999999999556 ) ) ;
#33322 = CARTESIAN_POINT ( 'NONE',  ( 19.34999999999999787, -4.330127018922190985, -2.500000000000001332 ) ) ;
#33323 = CARTESIAN_POINT ( 'NONE',  ( 20.10937500061451289, -4.541064518000417216, -2.621784821875001281 ) ) ;
#33324 = CARTESIAN_POINT ( 'NONE',  ( 2.121784821874999061, 13.35312500061451679, -33.67503911421598417 ) ) ;
#33325 = DIRECTION ( 'NONE',  ( 0.000000000000000000, 0.000000000000000000, -1.000000000000000000 ) ) ;
#33326 = CARTESIAN_POINT ( 'NONE',  ( 25.05937500061451217, 2.746126346562645981, -4.756430356249997438 ) ) ;
#33327 = CARTESIAN_POINT ( 'NONE',  ( 18.99375000122903501, -2.886751345948209480, -4.999999999999856115 ) ) ;
#33328 = CARTESIAN_POINT ( 'NONE',  ( 26.69062500061451715, -3.027376345333614438, 5.243569643749998122 ) ) ;
#33329 = CARTESIAN_POINT ( 'NONE',  ( -1.394453263437886604E-15, 19.66249999999999787, 33.99999999999999289 ) ) ;
#33330 = CARTESIAN_POINT ( 'NONE',  ( 24.14999999999999858, 0.000000000000000000, 4.999999999999998224 ) ) ;
#33331 =( BOUNDED_CURVE ( )  B_SPLINE_CURVE ( 2, ( #69245, #47068, #23794, #29353, #24157, #46345, #2013 ),
 .UNSPECIFIED., .F., .F. ) 
 B_SPLINE_CURVE_WITH_KNOTS ( ( 3, 2, 2, 3 ),
 ( 0.9854705224330112534, 0.9861111111111111605, 0.9888888888888889284, 0.9894640555095505219 ),
 .UNSPECIFIED. ) 
 CURVE ( )  GEOMETRIC_REPRESENTATION_ITEM ( )  RATIONAL_B_SPLINE_CURVE ( ( 0.9524577574850663364, 0.9691038605840708309, 1.000000000000000000, 0.8660254037844387076, 1.000000000000000000, 0.9722592223264697742, 0.9560064545842259509 ) ) 
 REPRESENTATION_ITEM ( '' )  );
#33332 = CARTESIAN_POINT ( 'NONE',  ( 25.64999999999999858, -4.330127018922190985, -2.500000000000001332 ) ) ;
#33333 = CARTESIAN_POINT ( 'NONE',  ( 10.19062500061451892, -3.027376345333610441, -5.243569643749999898 ) ) ;
#33334 = CARTESIAN_POINT ( 'NONE',  ( 26.18437500061451573, -2.746126346562646425, 4.756430356249996549 ) ) ;
#33335 = CARTESIAN_POINT ( 'NONE',  ( 21.90937500061451715, -4.541064518000417216, -2.621784821875001281 ) ) ;
#33336 = CARTESIAN_POINT ( 'NONE',  ( 14.70937500061451608, 2.746126346562645981, -4.756430356249997438 ) ) ;
#33337 = CARTESIAN_POINT ( 'NONE',  ( 4.828125000614518214, 6.421520780324663323E-16, -5.243569643749999010 ) ) ;
#33338 = CARTESIAN_POINT ( 'NONE',  ( 11.14687500061451608, -3.027376345333610441, -5.243569643749999898 ) ) ;
#33339 = ORIENTED_EDGE ( 'NONE', *, *, #40326, .F. ) ;
#33340 = CARTESIAN_POINT ( 'NONE',  ( 21.83437500061451786, -4.541064518000419881, 2.621784821874995952 ) ) ;
#33341 = CARTESIAN_POINT ( 'NONE',  ( 23.13750000122903216, 6.123233995736764310E-16, -4.999999999999998224 ) ) ;
#33342 = CARTESIAN_POINT ( 'NONE',  ( 29.47499999999999787, 4.330127018922191873, 2.499999999999999556 ) ) ;
#33344 = EDGE_CURVE ( 'NONE', #45665, #29422, #32043, .T. ) ;
#33343 = CARTESIAN_POINT ( 'NONE',  ( 4.312500000000000000, 2.886751345948126879, 4.999999999999999112 ) ) ;
#33345 = CARTESIAN_POINT ( 'NONE',  ( 15.03750000122903252, 6.123233995736764310E-16, -4.999999999999998224 ) ) ;
#33346 = CARTESIAN_POINT ( 'NONE',  ( 18.52499999999999858, 6.123233995736764310E-16, -4.999999999999998224 ) ) ;
#33347 = ORIENTED_EDGE ( 'NONE', *, *, #6059, .T. ) ;
#33348 = CARTESIAN_POINT ( 'NONE',  ( 11.62500000000000000, -4.330127018922194537, 2.499999999999995559 ) ) ;
#33349 = CARTESIAN_POINT ( 'NONE',  ( 15.86250000000000249, 2.886751345948129099, -4.999999999999998224 ) ) ;
#33350 = CARTESIAN_POINT ( 'NONE',  ( 13.12500000122903288, -5.773502691896255534, -1.060575238724906372E-15 ) ) ;
#33351 = CARTESIAN_POINT ( 'NONE',  ( 10.79062500061451679, 6.054752690667223547, 3.707466751127219781E-16 ) ) ;
#33352 = CARTESIAN_POINT ( 'NONE',  ( 9.525000000000002132, 6.123233995736764310E-16, -4.999999999999998224 ) ) ;
#33353 = CARTESIAN_POINT ( 'NONE',  ( 1.592000809091587073E-14, 16.85000000122903785, -34.00000000000000000 ) ) ;
#33354 = CARTESIAN_POINT ( 'NONE',  ( -3.000416591977282496E-16, 14.34687500061451715, -34.90005215228797653 ) ) ;
#33355 = CARTESIAN_POINT ( 'NONE',  ( 28.65000000122903145, 5.773502691896255534, 3.535250795749688894E-16 ) ) ;
#33356 = CARTESIAN_POINT ( 'NONE',  ( -3.756430356250000990, 14.70312499938548179, 32.16877607737301048 ) ) ;
#33357 = CARTESIAN_POINT ( 'NONE',  ( 6.787500000000001421, -2.886751345948125991, -5.000000000000000000 ) ) ;
#33358 = CARTESIAN_POINT ( 'NONE',  ( 20.78732959644809952, 4.500000000000000888, -5.500000000000000888 ) ) ;
#33359 = VERTEX_POINT ( 'NONE', #67782 ) ;
#33360 = CARTESIAN_POINT ( 'NONE',  ( 23.65312500061451573, -4.541064518000417216, -2.621784821875001281 ) ) ;
#33361 = CARTESIAN_POINT ( 'NONE',  ( 45.00000000000000000, 0.000000000000000000, 0.000000000000000000 ) ) ;
#33362 = CARTESIAN_POINT ( 'NONE',  ( 29.10937500061451644, -4.541064518000417216, -2.621784821875001281 ) ) ;
#33363 = CARTESIAN_POINT ( 'NONE',  ( 20.93437500061451573, -4.541064518000419881, 2.621784821874995952 ) ) ;
#33364 = CARTESIAN_POINT ( 'NONE',  ( 17.05312500061451786, 4.541064518000418104, -2.621784821874998173 ) ) ;
#33365 = EDGE_CURVE ( 'NONE', #66904, #68293, #41949, .T. ) ;
#33366 = CARTESIAN_POINT ( 'NONE',  ( -2.121784821874999949, 12.07812500061459637, -33.67503911421598417 ) ) ;
#33367 = CARTESIAN_POINT ( 'NONE',  ( 7.603125000614517681, 4.541064518000418104, -2.621784821874998173 ) ) ;
#33368 = CARTESIAN_POINT ( 'NONE',  ( 28.53750000122903074, 6.123233995736764310E-16, -4.999999999999998224 ) ) ;
#33369 = CARTESIAN_POINT ( 'NONE',  ( 24.60937500061451644, -4.119189519843965641, -2.378215178125001383 ) ) ;
#33370 = CARTESIAN_POINT ( 'NONE',  ( 19.60312500061451502, -4.541064518000417216, -2.621784821875001281 ) ) ;
#33371 = CARTESIAN_POINT ( 'NONE',  ( 7.584375000614516082, 5.824947211148865298E-16, -4.756430356249998326 ) ) ;
#33372 = CARTESIAN_POINT ( 'NONE',  ( 3.756430356249998770, 19.35312499938548214, 32.16877607737302469 ) ) ;
#33373 = CARTESIAN_POINT ( 'NONE',  ( 15.30937500061451750, 4.541064518000418104, -2.621784821874998173 ) ) ;
#33374 = CARTESIAN_POINT ( 'NONE',  ( 15.08437500061451786, -4.541064518000419881, 2.621784821874995952 ) ) ;
#33375 = CARTESIAN_POINT ( 'NONE',  ( 22.43437500061451573, 6.421520780324663323E-16, -5.243569643749999010 ) ) ;
#33376 = ORIENTED_EDGE ( 'NONE', *, *, #14874, .F. ) ;
#33377 = CARTESIAN_POINT ( 'NONE',  ( 27.11250000000000071, 2.886751345948115333, -5.000000000000023093 ) ) ;
#33378 = CARTESIAN_POINT ( 'NONE',  ( 26.80312500061451431, -4.541064518000417216, -2.621784821875001281 ) ) ;
#33379 = CARTESIAN_POINT ( 'NONE',  ( 26.35312500061451857, -4.541064518000417216, -2.621784821875001281 ) ) ;
#33380 = CARTESIAN_POINT ( 'NONE',  ( 7.743750001229034119, -2.886751345948126435, -5.000000000000000000 ) ) ;
#33381 = CARTESIAN_POINT ( 'NONE',  ( -3.999999999999999556, 17.71249999999999858, 27.69059892324149530 ) ) ;
#33382 = CARTESIAN_POINT ( 'NONE',  ( 5.334375000614517859, 6.421520780324663323E-16, -5.243569643749999010 ) ) ;
#33383 = CARTESIAN_POINT ( 'NONE',  ( 11.36250000122903536, -4.330127018922190985, -2.500000000000001332 ) ) ;
#33384 = CARTESIAN_POINT ( 'NONE',  ( 6.262500001229034829, 0.000000000000000000, 4.999999999999998224 ) ) ;
#33385 = CARTESIAN_POINT ( 'NONE',  ( 3.365625000614516082, -6.054752690667223547, -1.112240025338166033E-15 ) ) ;
#33386 = CARTESIAN_POINT ( 'NONE',  ( -8.484601909799255319E-16, 19.53124999877096712, 34.61880215351700940 ) ) ;
#33387 = CARTESIAN_POINT ( 'NONE',  ( 17.94375000122903074, -2.886751345948129988, 4.999999999999997335 ) ) ;
#33388 = CARTESIAN_POINT ( 'NONE',  ( 12.94687500061451857, -3.027376345333610441, -5.243569643749999898 ) ) ;
#33389 = CARTESIAN_POINT ( 'NONE',  ( 1.071796769724489673, 13.04240381056766829, 26.00000000000000000 ) ) ;
#33390 = ORIENTED_EDGE ( 'NONE', *, *, #37910, .F. ) ;
#33391 = CARTESIAN_POINT ( 'NONE',  ( 19.15312500061451573, -4.541064518000417216, -2.621784821875001281 ) ) ;
#33392 = CARTESIAN_POINT ( 'NONE',  ( 14.03437500061451715, 4.541064518000418104, 2.621784821874999949 ) ) ;
#33393 = CARTESIAN_POINT ( 'NONE',  ( 4.490625000614516971, 6.054752690667223547, 3.707466751127219781E-16 ) ) ;
#33394 = CARTESIAN_POINT ( 'NONE',  ( 22.28437500061451715, -4.541064518000419881, 2.621784821874995952 ) ) ;
#33395 = CARTESIAN_POINT ( 'NONE',  ( 10.69687500061451679, -3.027376345333610441, -5.243569643749999898 ) ) ;
#33396 = CARTESIAN_POINT ( 'NONE',  ( 5.503125000614516260, 0.000000000000000000, 5.243569643749999010 ) ) ;
#33397 = CARTESIAN_POINT ( 'NONE',  ( 10.76250000122903572, 0.000000000000000000, 4.999999999999998224 ) ) ;
#33398 = CARTESIAN_POINT ( 'NONE',  ( 5.475000001229035185, -5.773502691896255534, -1.060575238724906372E-15 ) ) ;
#33399 = CARTESIAN_POINT ( 'NONE',  ( 19.11562500061451431, -6.054752690667223547, -1.112240025338166033E-15 ) ) ;
#33400 = CARTESIAN_POINT ( 'NONE',  ( 7.312500001229033764, -4.330127018922190985, -2.500000000000001332 ) ) ;
#33401 = CARTESIAN_POINT ( 'NONE',  ( 17.39062500061451644, -3.027376345333610441, -5.243569643749999898 ) ) ;
#33402 = CARTESIAN_POINT ( 'NONE',  ( 15.10312500061451502, -4.541064518000417216, -2.621784821875001281 ) ) ;
#33403 = CARTESIAN_POINT ( 'NONE',  ( 25.09687500061451715, -2.746126346562642428, -4.756430356249999214 ) ) ;
#33404 = CARTESIAN_POINT ( 'NONE',  ( 16.05000000000000071, 0.000000000000000000, 4.999999999999998224 ) ) ;
#33405 = CARTESIAN_POINT ( 'NONE',  ( 8.625000001229034652, -5.773502691896255534, -1.060575238724906372E-15 ) ) ;
#33406 = CARTESIAN_POINT ( 'NONE',  ( 4.903125000614516615, 4.541064518000418104, -2.621784821874998173 ) ) ;
#33407 = CARTESIAN_POINT ( 'NONE',  ( 20.81250000122903643, -4.330127018922190985, -2.500000000000001332 ) ) ;
#33408 = CARTESIAN_POINT ( 'NONE',  ( 26.51249999999999929, -5.773502691896255534, -1.060575238724906372E-15 ) ) ;
#33409 = CARTESIAN_POINT ( 'NONE',  ( 9.001249775931846008E-16, 13.67187500061451999, -25.09994784771203058 ) ) ;
#33410 = DIRECTION ( 'NONE',  ( -1.000000000000000000, -0.000000000000000000, -0.000000000000000000 ) ) ;
#33411 = CARTESIAN_POINT ( 'NONE',  ( 3.225000001229033408, -5.773502691896255534, -1.060575238724906372E-15 ) ) ;
#33412 = CARTESIAN_POINT ( 'NONE',  ( 4.659375000614518925, 0.000000000000000000, 5.243569643749999010 ) ) ;
#33413 = CARTESIAN_POINT ( 'NONE',  ( 20.40937500061451715, 0.000000000000000000, 5.243569643749999010 ) ) ;
#33414 = CARTESIAN_POINT ( 'NONE',  ( 15.36562500061451608, 3.027376345333611329, 5.243569643749999010 ) ) ;
#33415 = CARTESIAN_POINT ( 'NONE',  ( 11.08125000122903181, 4.330127018922191873, 2.499999999999999556 ) ) ;
#33416 = CARTESIAN_POINT ( 'NONE',  ( 26.77499999999999858, 4.330127018922191873, 2.499999999999999556 ) ) ;
#33417 = CARTESIAN_POINT ( 'NONE',  ( 29.22187500061451715, 3.027376345333613106, -5.243569643749998122 ) ) ;
#33418 = CARTESIAN_POINT ( 'NONE',  ( 20.78437500061451715, -2.746126346562646425, 4.756430356249996549 ) ) ;
#33419 = CARTESIAN_POINT ( 'NONE',  ( 13.75312500061451715, -4.541064518000417216, -2.621784821875001281 ) ) ;
#33420 = CARTESIAN_POINT ( 'NONE',  ( 10.73437500061451644, 6.421520780324663323E-16, -5.243569643749999010 ) ) ;
#33421 = ORIENTED_EDGE ( 'NONE', *, *, #55194, .F. ) ;
#33422 = CARTESIAN_POINT ( 'NONE',  ( 29.31562500061451715, 3.027376345333611329, 5.243569643749999010 ) ) ;
#33423 = CARTESIAN_POINT ( 'NONE',  ( 22.60312500061451857, 0.000000000000000000, 5.243569643749999010 ) ) ;
#33424 = CARTESIAN_POINT ( 'NONE',  ( 7.320879633048903241E-15, 18.20000000122903216, 26.00000000000000355 ) ) ;
#33425 = CARTESIAN_POINT ( 'NONE',  ( 11.58750000000000036, -2.886751345948129988, 4.999999999999997335 ) ) ;
#33426 = CARTESIAN_POINT ( 'NONE',  ( 22.57500000122903572, -5.773502691896255534, -1.060575238724906372E-15 ) ) ;
#33427 = CARTESIAN_POINT ( 'NONE',  ( 16.90312500061451573, -4.541064518000417216, -2.621784821875001281 ) ) ;
#33428 = CARTESIAN_POINT ( 'NONE',  ( 12.15937500061451360, 2.746126346562643317, 4.756430356249998326 ) ) ;
#33429 = ORIENTED_EDGE ( 'NONE', *, *, #72450, .F. ) ;
#33430 = CARTESIAN_POINT ( 'NONE',  ( 20.02500000000000213, 4.330127018922191873, 2.499999999999999556 ) ) ;
#33431 = CARTESIAN_POINT ( 'NONE',  ( 21.64687500061451786, 6.054752690667223547, 3.707466751127219781E-16 ) ) ;
#33432 = CARTESIAN_POINT ( 'NONE',  ( 26.61562500061451786, 3.027376345333611329, 5.243569643749999010 ) ) ;
#33433 = VERTEX_POINT ( 'NONE', #12337 ) ;
#33434 = CARTESIAN_POINT ( 'NONE',  ( 7.978125000614517681, 6.421520780324663323E-16, -5.243569643749999010 ) ) ;
#33435 = CARTESIAN_POINT ( 'NONE',  ( 6.150000000000003020, 0.000000000000000000, 4.999999999999998224 ) ) ;
#33436 = CARTESIAN_POINT ( 'NONE',  ( 17.88749999999999929, -2.886751345948129988, 4.999999999999997335 ) ) ;
#33437 = CARTESIAN_POINT ( 'NONE',  ( 25.08749999999999858, -2.886751345948129988, 4.999999999999997335 ) ) ;
#33438 = CARTESIAN_POINT ( 'NONE',  ( 3.479729569495786379, -3.590471016896914946, -3.821457900550485398 ) ) ;
#33439 = CARTESIAN_POINT ( 'NONE',  ( 4.509375000614518569, 4.541064518000418104, -2.621784821874998173 ) ) ;
#33440 = CARTESIAN_POINT ( 'NONE',  ( 29.14687500061451075, -3.027376345333610441, -5.243569643749999898 ) ) ;
#33441 = ORIENTED_EDGE ( 'NONE', *, *, #38783, .F. ) ;
#33442 = CARTESIAN_POINT ( 'NONE',  ( 24.74062500061451786, 6.054752690667223547, 3.707466751127219781E-16 ) ) ;
#33443 = CARTESIAN_POINT ( 'NONE',  ( 24.30937500061451573, 4.541064518000418104, -2.621784821874998173 ) ) ;
#33444 = EDGE_CURVE ( 'NONE', #26592, #2667, #27899, .T. ) ;
#33445 = CARTESIAN_POINT ( 'NONE',  ( 3.756430356250000102, 12.75312499938548427, 30.00000000000000000 ) ) ;
#33446 = CARTESIAN_POINT ( 'NONE',  ( 13.27500000000000213, 4.330127018922191873, 2.499999999999999556 ) ) ;
#33447 = CARTESIAN_POINT ( 'NONE',  ( 9.703125000614514661, -4.541064518000417216, -2.621784821875001281 ) ) ;
#33448 = DIRECTION ( 'NONE',  ( 0.000000000000000000, 0.000000000000000000, 1.000000000000000000 ) ) ;
#33449 = DIRECTION ( 'NONE',  ( 0.000000000000000000, 1.000000000000000000, -0.000000000000000000 ) ) ;
#33450 = CARTESIAN_POINT ( 'NONE',  ( 25.26562500061451644, 3.027376345333611329, 5.243569643749999010 ) ) ;
#33451 = CARTESIAN_POINT ( 'NONE',  ( 20.32499999999999929, 6.123233995736764310E-16, -4.999999999999998224 ) ) ;
#33452 = CARTESIAN_POINT ( 'NONE',  ( 14.59687500061452070, -2.746126346562646425, 4.756430356249996549 ) ) ;
#33453 = CARTESIAN_POINT ( 'NONE',  ( 3.778125000614519280, -4.541064518000419881, 2.621784821874995952 ) ) ;
#33454 = CARTESIAN_POINT ( 'NONE',  ( 19.58437500061451786, -4.541064518000419881, 2.621784821874995952 ) ) ;
#33455 = CARTESIAN_POINT ( 'NONE',  ( -4.243569643749997233, 13.59687500061451715, 32.45002607614398471 ) ) ;
#33456 = CARTESIAN_POINT ( 'NONE',  ( 22.77187500061451786, -6.054752690667223547, -1.112240025338166033E-15 ) ) ;
#33457 = CARTESIAN_POINT ( 'NONE',  ( 29.85937500061451644, 0.000000000000000000, 5.243569643749999010 ) ) ;
#33458 = CARTESIAN_POINT ( 'NONE',  ( 9.703125000614514661, -4.541064518000417216, -2.621784821875001281 ) ) ;
#33459 = CARTESIAN_POINT ( 'NONE',  ( -2.000000000000000000, 15.08750000122903501, 26.53589838486224650 ) ) ;
#33460 = CARTESIAN_POINT ( 'NONE',  ( 8.109375000614518214, 4.541064518000418104, -2.621784821874998173 ) ) ;
#33461 = CARTESIAN_POINT ( 'NONE',  ( 3.943184062799388823, 3.074387202984122602, -4.182138569239902459 ) ) ;
#33462 = CARTESIAN_POINT ( 'NONE',  ( 7.978125000614517681, 6.421520780324663323E-16, -5.243569643749999010 ) ) ;
#33463 = CARTESIAN_POINT ( 'NONE',  ( 13.20937500061451786, 0.000000000000000000, 5.243569643749999010 ) ) ;
#33464 = CARTESIAN_POINT ( 'NONE',  ( 18.75000000122903288, 5.773502691896255534, 3.535250795749688894E-16 ) ) ;
#33465 = CARTESIAN_POINT ( 'NONE',  ( 8.971875000614515372, 3.027376345333613106, -5.243569643749998122 ) ) ;
#33466 = CARTESIAN_POINT ( 'NONE',  ( 9.853125000614516793, 4.541064518000418104, -2.621784821874998173 ) ) ;
#33467 = CARTESIAN_POINT ( 'NONE',  ( 5.128125000614516260, -4.541064518000419881, 2.621784821874995952 ) ) ;
#33468 = CARTESIAN_POINT ( 'NONE',  ( 24.80625000122903145, -4.330127018922190985, -2.500000000000001332 ) ) ;
#33469 = CARTESIAN_POINT ( 'NONE',  ( 18.27187500061451431, -6.054752690667223547, -1.112240025338166033E-15 ) ) ;
#33470 = CARTESIAN_POINT ( 'NONE',  ( 26.57812500061451644, 4.541064518000418104, 2.621784821874999949 ) ) ;
#33471 = CARTESIAN_POINT ( 'NONE',  ( 11.24062500061451608, 6.054752690667223547, 3.707466751127219781E-16 ) ) ;
#33472 = CARTESIAN_POINT ( 'NONE',  ( 29.44687500061451502, -3.027376345333614438, 5.243569643749998122 ) ) ;
#33473 = CARTESIAN_POINT ( 'NONE',  ( 4.243569643749999898, 12.88437500061451857, -30.00000000000000000 ) ) ;
#33474 = CARTESIAN_POINT ( 'NONE',  ( 13.72500000122903074, 2.886751345948129099, -4.999999999999998224 ) ) ;
#33475 = CARTESIAN_POINT ( 'NONE',  ( 28.41562500061451502, 3.027376345333611329, 5.243569643749999010 ) ) ;
#33476 = CARTESIAN_POINT ( 'NONE',  ( -4.243569643749999898, 16.20312500061451644, -30.00000000000000000 ) ) ;
#33477 = CARTESIAN_POINT ( 'NONE',  ( 16.31250000122903288, -4.330127018922190985, -2.500000000000001332 ) ) ;
#33478 = CARTESIAN_POINT ( 'NONE',  ( 13.50000000000000178, -4.330127018922190985, -2.500000000000001332 ) ) ;
#33479 = CARTESIAN_POINT ( 'NONE',  ( 10.31250000122903288, 0.000000000000000000, 4.999999999999998224 ) ) ;
#33480 = CARTESIAN_POINT ( 'NONE',  ( 23.61562500061451431, -6.054752690667223547, -1.112240025338166033E-15 ) ) ;
#33481 = CARTESIAN_POINT ( 'NONE',  ( 8.071875000614518569, 3.027376345333612662, -5.243569643749998122 ) ) ;
#33482 = CARTESIAN_POINT ( 'NONE',  ( 9.525000001229033231, -5.773502691896255534, -1.060575238724906372E-15 ) ) ;
#33483 = CARTESIAN_POINT ( 'NONE',  ( 19.76250000122903216, 0.000000000000000000, 4.999999999999998224 ) ) ;
#33484 = CARTESIAN_POINT ( 'NONE',  ( 14.31562500061451537, 3.027376345333613106, -5.243569643749998122 ) ) ;
#33485 = SHAPE_REPRESENTATION ( 'MAS-181', ( #47401, #22614, #6134, #26153, #69825, #32064 ), #35583 ) ;
#33486 = CARTESIAN_POINT ( 'NONE',  ( 19.19062500061452070, -3.027376345333610441, -5.243569643749999898 ) ) ;
#33487 = CARTESIAN_POINT ( 'NONE',  ( 25.91250000122903074, 4.330127018922192761, -2.499999999999997780 ) ) ;
#33488 = EDGE_CURVE ( 'NONE', #885, #11117, #39598, .T. ) ;
#33489 = CARTESIAN_POINT ( 'NONE',  ( 29.17500000122903714, 2.886751345948126879, 4.999999999999999112 ) ) ;
#33490 = CARTESIAN_POINT ( 'NONE',  ( 22.76249999999999574, 2.886751345948126879, 4.999999999999999112 ) ) ;
#33491 = CARTESIAN_POINT ( 'NONE',  ( 25.09687500061451715, -3.027376345333610441, -5.243569643749999898 ) ) ;
#33492 = DIRECTION ( 'NONE',  ( -1.000000000000000000, -0.000000000000000000, -0.000000000000000000 ) ) ;
#33493 = CARTESIAN_POINT ( 'NONE',  ( 10.91250000122903252, -4.330127018922190985, -2.500000000000001332 ) ) ;
#33494 = CARTESIAN_POINT ( 'NONE',  ( 27.04687500061451644, 6.054752690667223547, 3.707466751127219781E-16 ) ) ;
#33495 = CARTESIAN_POINT ( 'NONE',  ( -3.999999999999999112, 13.21250000000000213, 27.69059892324149885 ) ) ;
#33496 = CARTESIAN_POINT ( 'NONE',  ( 3.871875000614519280, -6.054752690667223547, -1.112240025338166033E-15 ) ) ;
#33497 = CARTESIAN_POINT ( 'NONE',  ( 23.05312500061451431, 0.000000000000000000, 5.243569643749999010 ) ) ;
#33498 = CARTESIAN_POINT ( 'NONE',  ( -3.756430356250000990, 14.81562499938548427, 32.16877607737301048 ) ) ;
#33499 = LINE ( 'NONE', #39061, #66882 ) ;
#33500 = CARTESIAN_POINT ( 'NONE',  ( 9.196875000614518569, -3.027376345333614438, 5.243569643749998122 ) ) ;
#33501 = CARTESIAN_POINT ( 'NONE',  ( 4.924325218087134637, -0.8666147624583920850, 4.924325218087160394 ) ) ;
#33502 = CARTESIAN_POINT ( 'NONE',  ( 3.459375000614519635, -4.541064518000417216, -2.621784821875001281 ) ) ;
#33503 = CARTESIAN_POINT ( 'NONE',  ( 6.871875000614517504, 3.027376345333611329, 5.243569643749999010 ) ) ;
#33504 = CARTESIAN_POINT ( 'NONE',  ( 28.24687500061451573, -3.027376345333610441, -5.243569643749999898 ) ) ;
#33505 = CARTESIAN_POINT ( 'NONE',  ( -4.243569643749998122, 9.940625000614591755, 32.45002607614398471 ) ) ;
#33506 = CARTESIAN_POINT ( 'NONE',  ( 19.91250000000000142, 2.886751345948129099, -4.999999999999998224 ) ) ;
#33507 = VERTEX_POINT ( 'NONE', #23780 ) ;
#33508 = CARTESIAN_POINT ( 'NONE',  ( 26.25000000000000000, 4.330127018922192761, -2.499999999999997780 ) ) ;
#33509 = CARTESIAN_POINT ( 'NONE',  ( 28.50937500061451502, 0.000000000000000000, 5.243569643749999010 ) ) ;
#33510 = ORIENTED_EDGE ( 'NONE', *, *, #50852, .T. ) ;
#33511 = CARTESIAN_POINT ( 'NONE',  ( 16.97812500061451502, 6.421520780324663323E-16, -5.243569643749999010 ) ) ;
#33512 = CARTESIAN_POINT ( 'NONE',  ( 8.390625000614518214, -3.027376345333610441, -5.243569643749999898 ) ) ;
#33513 = CARTESIAN_POINT ( 'NONE',  ( 22.28437500061451360, -2.746126346562642428, -4.756430356249999214 ) ) ;
#33514 = CARTESIAN_POINT ( 'NONE',  ( 3.796875000614517326, -3.027376345333614438, 5.243569643749998122 ) ) ;
#33515 = CARTESIAN_POINT ( 'NONE',  ( 17.73750000122903359, 6.123233995736764310E-16, -4.999999999999998224 ) ) ;
#33516 = CARTESIAN_POINT ( 'NONE',  ( 25.42500000000000071, 4.330127018922191873, 2.499999999999999556 ) ) ;
#33517 = CARTESIAN_POINT ( 'NONE',  ( 15.59999999999999964, 0.000000000000000000, 4.999999999999998224 ) ) ;
#33518 = CARTESIAN_POINT ( 'NONE',  ( 6.496875000614517504, -3.027376345333614438, 5.243569643749998122 ) ) ;
#33519 = CARTESIAN_POINT ( 'NONE',  ( 11.37187500061451750, 3.027376345333611329, 5.243569643749999010 ) ) ;
#33520 = CARTESIAN_POINT ( 'NONE',  ( 22.95937500061451431, 4.541064518000418104, -2.621784821874998173 ) ) ;
#33521 = CARTESIAN_POINT ( 'NONE',  ( 7.724999999999999645, 6.123233995736764310E-16, -4.999999999999998224 ) ) ;
#33522 = ORIENTED_EDGE ( 'NONE', *, *, #10883, .F. ) ;
#33523 = CARTESIAN_POINT ( 'NONE',  ( 3.571875000614517237, 3.027376345333613106, -5.243569643749998122 ) ) ;
#33524 = CARTESIAN_POINT ( 'NONE',  ( 10.72500000000000142, -4.330127018922194537, 2.499999999999995559 ) ) ;
#33525 =( BOUNDED_CURVE ( )  B_SPLINE_CURVE ( 2, ( #54171, #37536, #48998, #2460, #48265, #60058, #71529 ),
 .UNSPECIFIED., .F., .F. ) 
 B_SPLINE_CURVE_WITH_KNOTS ( ( 3, 2, 2, 3 ),
 ( 0.7000000000000001776, 0.7033333333333335879, 0.7066666666666668872, 0.7100000000000001865 ),
 .UNSPECIFIED. ) 
 CURVE ( )  GEOMETRIC_REPRESENTATION_ITEM ( )  RATIONAL_B_SPLINE_CURVE ( ( 0.9999999999999911182, 0.8660254037844475894, 1.000000000000000000, 0.8660254037844387076, 1.000000000000000000, 0.8660254037844298258, 1.000000000000008882 ) ) 
 REPRESENTATION_ITEM ( '' )  );
#33526 = CARTESIAN_POINT ( 'NONE',  ( 7.134375000614516793, 6.421520780324663323E-16, -5.243569643749999010 ) ) ;
#33527 = CARTESIAN_POINT ( 'NONE',  ( -1.878215178125001827, 14.29062499938548392, 33.25316411605952283 ) ) ;
#33528 = CARTESIAN_POINT ( 'NONE',  ( 21.60000000000000142, -4.330127018922190985, -2.500000000000001332 ) ) ;
#33529 = CARTESIAN_POINT ( 'NONE',  ( 15.51562500061451644, -6.054752690667223547, -1.112240025338166033E-15 ) ) ;
#33530 = CARTESIAN_POINT ( 'NONE',  ( 4.000000000000000000, 17.89999999999999858, 30.00000000000000000 ) ) ;
#33531 = CYLINDRICAL_SURFACE ( 'NONE', #66977, 4.999999999999998224 ) ;
#33532 = CARTESIAN_POINT ( 'NONE',  ( 21.83437500061451786, -4.119189519843968306, 2.378215178124996054 ) ) ;
#33533 = CARTESIAN_POINT ( 'NONE',  ( 9.140625000614518214, -3.027376345333614438, 5.243569643749998122 ) ) ;
#33534 = CARTESIAN_POINT ( 'NONE',  ( 25.95937500061451431, -4.541064518000417216, -2.621784821875001281 ) ) ;
#33535 = CARTESIAN_POINT ( 'NONE',  ( 20.13750000000000639, -2.886751345948130876, 4.999999999999996447 ) ) ;
#33536 = CARTESIAN_POINT ( 'NONE',  ( 28.92187500061451644, 3.027376345333611329, 5.243569643749999010 ) ) ;
#33537 = CARTESIAN_POINT ( 'NONE',  ( 11.02500000000000036, 4.330127018922191873, 2.499999999999999556 ) ) ;
#33538 = CARTESIAN_POINT ( 'NONE',  ( 1.999999999999998668, 16.36250000122903359, 26.53589838486224650 ) ) ;
#33539 = CARTESIAN_POINT ( 'NONE',  ( 9.037500001229034297, -4.330127018922194537, 2.499999999999995559 ) ) ;
#33540 = CARTESIAN_POINT ( 'NONE',  ( 19.09687500061451360, -3.027376345333614438, 5.243569643749998122 ) ) ;
#33541 = CARTESIAN_POINT ( 'NONE',  ( 13.65937500061451715, 0.000000000000000000, 5.243569643749999010 ) ) ;
#33542 = CARTESIAN_POINT ( 'NONE',  ( 9.337500001229033231, 4.330127018922191873, 2.499999999999999556 ) ) ;
#33543 = ORIENTED_EDGE ( 'NONE', *, *, #13440, .T. ) ;
#33544 = VECTOR ( 'NONE', #57194, 1000.000000000000000 ) ;
#33545 = CARTESIAN_POINT ( 'NONE',  ( 14.24062500061451608, -3.027376345333610441, -5.243569643749999898 ) ) ;
#33546 = CARTESIAN_POINT ( 'NONE',  ( 25.23750000122903359, -4.330127018922194537, 2.499999999999995559 ) ) ;
#33547 = CARTESIAN_POINT ( 'NONE',  ( 15.23437500061451644, 6.421520780324663323E-16, -5.243569643749999010 ) ) ;
#33548 = CARTESIAN_POINT ( 'NONE',  ( 4.519730000842647755, 8.925305311771484895, -26.03535200691664642 ) ) ;
#33549 = CARTESIAN_POINT ( 'NONE',  ( 16.41562500061451857, -6.054752690667223547, -1.112240025338166033E-15 ) ) ;
#33550 = CARTESIAN_POINT ( 'NONE',  ( 4.000000000000000000, 20.13124999877096499, 27.69059892324149885 ) ) ;
#33551 = CARTESIAN_POINT ( 'NONE',  ( 27.27187500061451431, -6.054752690667223547, -1.112240025338166033E-15 ) ) ;
#33552 = CARTESIAN_POINT ( 'NONE',  ( 9.001249775931846008E-16, 10.46562500061451928, 34.90005215228797653 ) ) ;
#33553 = CARTESIAN_POINT ( 'NONE',  ( 14.78437500061451715, 6.421520780324663323E-16, -5.243569643749999010 ) ) ;
#33554 = CARTESIAN_POINT ( 'NONE',  ( 14.66250000122903252, 4.330127018922192761, -2.499999999999997780 ) ) ;
#33555 = DIRECTION ( 'NONE',  ( -0.000000000000000000, -1.000000000000000000, -0.000000000000000000 ) ) ;
#33556 = CARTESIAN_POINT ( 'NONE',  ( 3.360320061989407137, -3.702473467127644469, 3.713053667660598745 ) ) ;
#33557 = CARTESIAN_POINT ( 'NONE',  ( 19.99687500061451573, -3.027376345333614438, 5.243569643749998122 ) ) ;
#33558 = CARTESIAN_POINT ( 'NONE',  ( 21.11250000122903359, 0.000000000000000000, 4.999999999999998224 ) ) ;
#33559 =( BOUNDED_CURVE ( )  B_SPLINE_CURVE ( 2, ( #16485, #5421, #10597, #10958, #71928, #27227, #26866 ),
 .UNSPECIFIED., .F., .F. ) 
 B_SPLINE_CURVE_WITH_KNOTS ( ( 3, 2, 2, 3 ),
 ( 0.2499999999999999722, 0.2533333333333333548, 0.2566666666666667096, 0.2600000000000000644 ),
 .UNSPECIFIED. ) 
 CURVE ( )  GEOMETRIC_REPRESENTATION_ITEM ( )  RATIONAL_B_SPLINE_CURVE ( ( 1.000000000000001110, 0.8660254037844374864, 1.000000000000000000, 0.8660254037844387076, 1.000000000000000000, 0.8660254037844364872, 1.000000000000002220 ) ) 
 REPRESENTATION_ITEM ( '' )  );
#33560 = VECTOR ( 'NONE', #13501, 1000.000000000000000 ) ;
#33561 = CARTESIAN_POINT ( 'NONE',  ( 17.55937500061451573, 4.541064518000418104, -2.621784821874998173 ) ) ;
#33562 = CARTESIAN_POINT ( 'NONE',  ( 4.243569643749999898, 13.29687500061451644, 32.45002607614398471 ) ) ;
#33563 = CARTESIAN_POINT ( 'NONE',  ( 16.45312500061451289, -4.541064518000417216, -2.621784821875001281 ) ) ;
#33564 = ORIENTED_EDGE ( 'NONE', *, *, #51473, .F. ) ;
#33565 = VERTEX_POINT ( 'NONE', #72959 ) ;
#33566 = AXIS2_PLACEMENT_3D ( 'NONE', #51044, #18121, #51405 ) ;
#33567 = CARTESIAN_POINT ( 'NONE',  ( 19.79999999999999716, -4.330127018922190985, -2.500000000000001332 ) ) ;
#33568 = CARTESIAN_POINT ( 'NONE',  ( 17.43750000000000000, -2.886751345948096681, 5.000000000000054179 ) ) ;
#33569 = CARTESIAN_POINT ( 'NONE',  ( 25.52812500061451573, 6.421520780324663323E-16, -5.243569643749999010 ) ) ;
#33570 = CARTESIAN_POINT ( 'NONE',  ( 2.803125000614518747, 0.000000000000000000, 5.243569643749999010 ) ) ;
#33571 = CARTESIAN_POINT ( 'NONE',  ( 17.02500000122903145, 2.886751345948126879, 4.999999999999999112 ) ) ;
#33572 = CARTESIAN_POINT ( 'NONE',  ( 21.66562500061451502, 3.027376345333611329, 5.243569643749999010 ) ) ;
#33573 = CARTESIAN_POINT ( 'NONE',  ( 26.05312500061451431, 4.541064518000418104, -2.621784821874998173 ) ) ;
#33574 = CARTESIAN_POINT ( 'NONE',  ( 6.065625000614516260, -6.054752690667223547, -1.112240025338166033E-15 ) ) ;
#33575 = ORIENTED_EDGE ( 'NONE', *, *, #35397, .T. ) ;
#33576 = EDGE_CURVE ( 'NONE', #42322, #62008, #915, .T. ) ;
#33577 = CARTESIAN_POINT ( 'NONE',  ( -1.626862140677534273E-15, 20.43124999877096570, 34.00000000000000000 ) ) ;
#33578 = CARTESIAN_POINT ( 'NONE',  ( 17.21249999999999858, 2.886751345948073588, -5.000000000000094147 ) ) ;
#33579 =( BOUNDED_CURVE ( )  B_SPLINE_CURVE ( 2, ( #425, #17396, #4523, #40304, #69113, #12582, #29933, #19193, #47293 ),
 .UNSPECIFIED., .F., .F. ) 
 B_SPLINE_CURVE_WITH_KNOTS ( ( 3, 2, 2, 2, 3 ),
 ( 0.3804347826086956763, 0.3840579710144927383, 0.3913043478260869734, 0.3985507246376811530, 0.4021739130434782705 ),
 .UNSPECIFIED. ) 
 CURVE ( )  GEOMETRIC_REPRESENTATION_ITEM ( )  RATIONAL_B_SPLINE_CURVE ( ( 0.9330127018922194093, 0.9330127018922198534, 1.000000000000000000, 0.8660254037844387076, 1.000000000000000000, 0.8660254037844387076, 1.000000000000000000, 0.9330127018922194093, 0.9330127018922194093 ) ) 
 REPRESENTATION_ITEM ( '' )  );
#33580 = CARTESIAN_POINT ( 'NONE',  ( 11.40937500061451892, 0.000000000000000000, 4.756430356249998326 ) ) ;
#33581 = CARTESIAN_POINT ( 'NONE',  ( 34.99999999999999289, 9.426999614876460059E-14, 9.000000000000000000 ) ) ;
#33582 = CARTESIAN_POINT ( 'NONE',  ( -3.999999999999999112, 11.56250000122903465, -30.00000000000000000 ) ) ;
#33583 = CARTESIAN_POINT ( 'NONE',  ( 4.243569643749999010, 18.32187500061451502, -32.45002607614398471 ) ) ;
#33584 = CARTESIAN_POINT ( 'NONE',  ( 7.687500000000000000, -2.886751345948125991, -5.000000000000000000 ) ) ;
#33585 = CARTESIAN_POINT ( 'NONE',  ( 3.525000001229034119, 2.886751345948126879, 4.999999999999999112 ) ) ;
#33586 = CARTESIAN_POINT ( 'NONE',  ( 12.68437500061451573, 4.541064518000418104, 2.621784821874999949 ) ) ;
#33587 = CARTESIAN_POINT ( 'NONE',  ( 1.999999999999998668, 16.81250000122903643, -33.46410161513775705 ) ) ;
#33588 = CARTESIAN_POINT ( 'NONE',  ( 2.859375000614519546, 0.000000000000000000, 5.243569643749999010 ) ) ;
#33589 = CARTESIAN_POINT ( 'NONE',  ( 12.11250000000000249, -5.773502691896255534, -1.060575238724906372E-15 ) ) ;
#33590 = CIRCLE ( 'NONE', #43037, 1.500000000000000888 ) ;
#33591 = CARTESIAN_POINT ( 'NONE',  ( -3.999999999999997335, 10.70000000122903394, 32.30940107675850470 ) ) ;
#33592 = CARTESIAN_POINT ( 'NONE',  ( 8.971875000614515372, 3.027376345333613106, -5.243569643749998122 ) ) ;
#33593 = DIRECTION ( 'NONE',  ( -1.000000000000000000, -0.000000000000000000, -0.000000000000000000 ) ) ;
#33594 = CARTESIAN_POINT ( 'NONE',  ( 20.42812500061451431, -4.541064518000419881, 2.621784821874995952 ) ) ;
#33595 = CARTESIAN_POINT ( 'NONE',  ( 16.68750000000000000, -2.886751345948126435, -5.000000000000000000 ) ) ;
#33596 = CARTESIAN_POINT ( 'NONE',  ( -2.121784821874999949, 17.92812500061459602, 26.32496088578401938 ) ) ;
#33597 = CARTESIAN_POINT ( 'NONE',  ( 22.58437500061451431, 4.541064518000418104, 2.621784821874999949 ) ) ;
#33598 = CYLINDRICAL_SURFACE ( 'NONE', #24915, 3.999999999999996447 ) ;
#33599 = CARTESIAN_POINT ( 'NONE',  ( 29.02500000122903145, 2.886751345948129099, -4.999999999999998224 ) ) ;
#33600 = AXIS2_PLACEMENT_3D ( 'NONE', #29083, #51618, #1019 ) ;
#33601 = CARTESIAN_POINT ( 'NONE',  ( 19.69687500061451502, 4.119189519843966529, -2.378215178124998275 ) ) ;
#33602 = CARTESIAN_POINT ( 'NONE',  ( 26.20312500061451644, 0.000000000000000000, 5.243569643749999010 ) ) ;
#33603 = CARTESIAN_POINT ( 'NONE',  ( 15.70312500061451644, 4.541064518000418104, -2.621784821874998173 ) ) ;
#33604 = CARTESIAN_POINT ( 'NONE',  ( 15.39375000122903181, -2.886751345948125991, -5.000000000000000000 ) ) ;
#33605 = CARTESIAN_POINT ( 'NONE',  ( 10.95937500061451964, 0.000000000000000000, 5.243569643749999010 ) ) ;
#33606 = CARTESIAN_POINT ( 'NONE',  ( 28.27499999999999858, -4.330127018922194537, 2.499999999999995559 ) ) ;
#33607 = CARTESIAN_POINT ( 'NONE',  ( 25.46250000122903501, 4.330127018922192761, -2.499999999999997780 ) ) ;
#33608 = CARTESIAN_POINT ( 'NONE',  ( 27.00000000000000000, -4.330127018922190985, -2.500000000000001332 ) ) ;
#33609 = CARTESIAN_POINT ( 'NONE',  ( 15.12187500061451750, -6.054752690667223547, -1.112240025338166033E-15 ) ) ;
#33610 = CARTESIAN_POINT ( 'NONE',  ( 29.07187500061451502, -6.054752690667223547, -1.112240025338166033E-15 ) ) ;
#33611 = LINE ( 'NONE', #15889, #11213 ) ;
#33612 = CARTESIAN_POINT ( 'NONE',  ( 16.72500000122903430, -5.773502691896255534, -1.060575238724906372E-15 ) ) ;
#33613 = CARTESIAN_POINT ( 'NONE',  ( 23.85937500061451644, 4.541064518000418104, -2.621784821874998173 ) ) ;
#33614 = CARTESIAN_POINT ( 'NONE',  ( 15.34687500061451537, 6.054752690667223547, 3.707466751127219781E-16 ) ) ;
#33615 = CARTESIAN_POINT ( 'NONE',  ( -3.756430356250000102, 16.12812499938548427, 30.00000000000000000 ) ) ;
#33616 = CARTESIAN_POINT ( 'NONE',  ( 29.09999999999999787, 0.000000000000000000, 4.999999999999998224 ) ) ;
#33617 = CARTESIAN_POINT ( 'NONE',  ( 4.312500001229034652, 4.330127018922192761, -2.499999999999997780 ) ) ;
#33618 = CARTESIAN_POINT ( 'NONE',  ( 5.100000000000000533, 4.330127018922192761, -2.499999999999997780 ) ) ;
#33619 = CARTESIAN_POINT ( 'NONE',  ( 7.659375000614514484, 2.746126346562643317, 4.756430356249998326 ) ) ;
#33620 = CARTESIAN_POINT ( 'NONE',  ( 19.52812500061451573, -4.541064518000419881, 2.621784821874995952 ) ) ;
#33621 = CARTESIAN_POINT ( 'NONE',  ( 9.562500000000001776, 2.886751345948129099, -4.999999999999998224 ) ) ;
#33622 = FACE_OUTER_BOUND ( 'NONE', #63314, .T. ) ;
#33623 = CARTESIAN_POINT ( 'NONE',  ( 17.25000000000000000, 4.330127018922192761, -2.499999999999997780 ) ) ;
#33624 = CARTESIAN_POINT ( 'NONE',  ( -4.243569643749997233, 12.64062500061451999, 32.45002607614398471 ) ) ;
#33625 = DIRECTION ( 'NONE',  ( -1.000000000000000000, -0.000000000000000000, -0.000000000000000000 ) ) ;
#33626 = CARTESIAN_POINT ( 'NONE',  ( 21.97500000122903074, 2.886751345948126879, 4.999999999999999112 ) ) ;
#33627 = CARTESIAN_POINT ( 'NONE',  ( 15.07499999999999929, 4.330127018922191873, 2.499999999999999556 ) ) ;
#33628 = CARTESIAN_POINT ( 'NONE',  ( 27.68437500061451573, -4.541064518000419881, 2.621784821874995952 ) ) ;
#33629 = VERTEX_POINT ( 'NONE', #11985 ) ;
#33630 = CARTESIAN_POINT ( 'NONE',  ( 16.97812500061451502, 6.421520780324663323E-16, -5.243569643749999010 ) ) ;
#33631 = CARTESIAN_POINT ( 'NONE',  ( 22.82812500061451644, 6.421520780324663323E-16, -5.243569643749999010 ) ) ;
#33632 = B_SPLINE_CURVE_WITH_KNOTS ( 'NONE', 3,
 ( #24090, #46637, #494, #41104, #7471, #62533, #29997, #52538, #1947, #24453, #23003, #45563, #47002, #69537, #34455, #18896, #23368, #63976, #40371, #13359, #56983, #45916, #62889, #17810, #68448, #6387, #28920, #12284, #34817, #57347, #13735, #31833, #48097, #14466, #14830, #43291, #64711, #14095, #31465, #8565, #36635, #65075, #8201, #36999, #42548, #25556 ),
 .UNSPECIFIED., .F., .F.,
 ( 4, 2, 2, 2, 2, 2, 2, 2, 2, 2, 2, 2, 2, 2, 2, 2, 2, 2, 2, 2, 2, 2, 4 ),
 ( 0.000000000000000000, 0.001203096460345648173, 0.002406192920691296346, 0.003609289381036944518, 0.004812385841382592691, 0.005413934071555414826, 0.006015482301728236093, 0.007218578762073870822, 0.008421675222419504683, 0.009023223452592316410, 0.009624771682765129871, 0.01082786814311074639, 0.01142941637328355291, 0.01203096460345635769, 0.01323406106380197247, 0.01443715752414758725, 0.01503870575432038684, 0.01564025398449318469, 0.01684335044483878038, 0.01744489867501157823, 0.01804644690518437608, 0.01864799513535717046, 0.01924954336552996831 ),
 .UNSPECIFIED. ) ;
#33633 = CARTESIAN_POINT ( 'NONE',  ( 22.73437500061451644, -4.541064518000419881, 2.621784821874995952 ) ) ;
#33634 = CARTESIAN_POINT ( 'NONE',  ( 5.962500000000002132, 2.886751345948129099, -4.999999999999998224 ) ) ;
#33635 = CARTESIAN_POINT ( 'NONE',  ( 10.19062500061451892, -3.027376345333610441, -5.243569643749999898 ) ) ;
#33636 = CARTESIAN_POINT ( 'NONE',  ( 24.44062500061451715, -3.027376345333614438, 5.243569643749998122 ) ) ;
#33637 = CARTESIAN_POINT ( 'NONE',  ( 15.60937500061451644, -4.541064518000417216, -2.621784821875001281 ) ) ;
#33638 = CARTESIAN_POINT ( 'NONE',  ( 19.99687500061451573, -3.027376345333614438, 5.243569643749998122 ) ) ;
#33639 = DIRECTION ( 'NONE',  ( -1.000000000000000000, 0.000000000000000000, 0.000000000000000000 ) ) ;
#33640 = CARTESIAN_POINT ( 'NONE',  ( -2.121784821874999949, 17.02812500061451573, 26.32496088578401938 ) ) ;
#33641 = CARTESIAN_POINT ( 'NONE',  ( 20.40000000122903145, -2.886751345948125991, -5.000000000000000000 ) ) ;
#33642 = CARTESIAN_POINT ( 'NONE',  ( 13.92187500061451289, 2.746126346562645981, -4.756430356249997438 ) ) ;
#33643 = CARTESIAN_POINT ( 'NONE',  ( 12.25312500061451537, 0.000000000000000000, 5.243569643749999010 ) ) ;
#33644 = CARTESIAN_POINT ( 'NONE',  ( 6.084375000614518747, -4.541064518000419881, 2.621784821874995952 ) ) ;
#33645 = CARTESIAN_POINT ( 'NONE',  ( 4.209375000614516971, 0.000000000000000000, 5.243569643749999010 ) ) ;
#33646 = ORIENTED_EDGE ( 'NONE', *, *, #40344, .F. ) ;
#33647 = CARTESIAN_POINT ( 'NONE',  ( 28.92187500061451644, 3.027376345333611329, 5.243569643749999010 ) ) ;
#33648 = CARTESIAN_POINT ( 'NONE',  ( 19.90312500061451573, 0.000000000000000000, 5.243569643749999010 ) ) ;
#33649 = CARTESIAN_POINT ( 'NONE',  ( 27.75000000122903288, 5.773502691896255534, 3.535250795749688894E-16 ) ) ;
#33650 = CARTESIAN_POINT ( 'NONE',  ( 26.72812500061451502, -4.541064518000419881, 2.621784821874995952 ) ) ;
#33651 = CARTESIAN_POINT ( 'NONE',  ( 25.17187500061451644, 3.027376345333613106, -5.243569643749998122 ) ) ;
#33652 = CARTESIAN_POINT ( 'NONE',  ( 16.34062500061451573, -3.027376345333614438, 5.243569643749998122 ) ) ;
#33653 = CARTESIAN_POINT ( 'NONE',  ( 3.999999999999999112, 10.32500000000000107, 30.00000000000000000 ) ) ;
#33654 = CARTESIAN_POINT ( 'NONE',  ( 25.26562500061451289, 3.027376345333611329, 5.243569643749999010 ) ) ;
#33655 = CARTESIAN_POINT ( 'NONE',  ( 4.237500001229036251, 6.123233995736764310E-16, -4.999999999999998224 ) ) ;
#33656 = VERTEX_POINT ( 'NONE', #17513 ) ;
#33657 = CARTESIAN_POINT ( 'NONE',  ( 27.29999999999999716, 0.000000000000000000, 4.999999999999998224 ) ) ;
#33658 = CARTESIAN_POINT ( 'NONE',  ( -3.999999999999999112, 14.60000000000000142, -30.00000000000000000 ) ) ;
#33659 = CARTESIAN_POINT ( 'NONE',  ( -3.756430356250000102, 16.57812499938548356, 30.00000000000000000 ) ) ;
#33660 = EDGE_CURVE ( 'NONE', #1565, #40669, #49515, .T. ) ;
#33661 = CARTESIAN_POINT ( 'NONE',  ( 4.959375000614516971, 4.541064518000418104, -2.621784821874998173 ) ) ;
#33662 = CARTESIAN_POINT ( 'NONE',  ( 13.30312500061451786, -4.541064518000417216, -2.621784821875001281 ) ) ;
#33663 = CARTESIAN_POINT ( 'NONE',  ( 7.171875000614517326, 3.027376345333613106, -5.243569643749998122 ) ) ;
#33664 = CARTESIAN_POINT ( 'NONE',  ( 25.57500000122903216, 2.886751345948126879, 4.999999999999999112 ) ) ;
#33665 = VECTOR ( 'NONE', #54515, 1000.000000000000000 ) ;
#33666 = CARTESIAN_POINT ( 'NONE',  ( 14.07187500061451679, 3.027376345333611329, 5.243569643749999010 ) ) ;
#33667 = CARTESIAN_POINT ( 'NONE',  ( 3.084375000614519191, 6.421520780324663323E-16, -5.243569643749999010 ) ) ;
#33668 = CARTESIAN_POINT ( 'NONE',  ( 27.86249999999999716, -5.773502691896255534, -1.060575238724906372E-15 ) ) ;
#33669 = CARTESIAN_POINT ( 'NONE',  ( 27.34687500061451360, -3.027376345333610441, -5.243569643749999898 ) ) ;
#33670 = CARTESIAN_POINT ( 'NONE',  ( 14.24999999999999822, 0.000000000000000000, 4.999999999999998224 ) ) ;
#33671 = CARTESIAN_POINT ( 'NONE',  ( 13.86562500061451431, 3.027376345333613106, -5.243569643749998122 ) ) ;
#33672 = ORIENTED_EDGE ( 'NONE', *, *, #69921, .T. ) ;
#33673 = VECTOR ( 'NONE', #47141, 1000.000000000000000 ) ;
#33674 = CARTESIAN_POINT ( 'NONE',  ( 10.34062500061451750, 6.054752690667223547, 3.707466751127219781E-16 ) ) ;
#33675 = AXIS2_PLACEMENT_3D ( 'NONE', #65580, #20876, #65951 ) ;
#33676 = CARTESIAN_POINT ( 'NONE',  ( 6.590625000614518392, -3.027376345333610441, -5.243569643749999898 ) ) ;
#33677 = CARTESIAN_POINT ( 'NONE',  ( 18.04687500061451999, 5.492252693125287522, 3.363034840372157021E-16 ) ) ;
#33678 = CARTESIAN_POINT ( 'NONE',  ( 16.08749999999999503, -2.886751345948129988, 4.999999999999997335 ) ) ;
#33679 = CARTESIAN_POINT ( 'NONE',  ( 17.22187500061451715, 3.027376345333611329, 5.243569643749999010 ) ) ;
#33680 = CARTESIAN_POINT ( 'NONE',  ( 13.87500000122903465, 2.886751345948126879, 4.999999999999999112 ) ) ;
#33681 = CARTESIAN_POINT ( 'NONE',  ( 19.57500000000000284, 4.330127018922191873, 2.499999999999999556 ) ) ;
#33682 = CARTESIAN_POINT ( 'NONE',  ( 21.23437500061451644, 4.541064518000418104, 2.621784821874999949 ) ) ;
#33683 = CARTESIAN_POINT ( 'NONE',  ( -2.121784821874999949, 12.97812500061451679, -33.67503911421598417 ) ) ;
#33684 = CARTESIAN_POINT ( 'NONE',  ( 25.69687500061451502, 0.000000000000000000, 4.756430356249998326 ) ) ;
#33685 = CARTESIAN_POINT ( 'NONE',  ( 4.162457142321725811, 2.770219694541247168, 4.452085545162252522 ) ) ;
#33686 = CARTESIAN_POINT ( 'NONE',  ( 27.74062500061451431, -3.027376345333610441, -5.243569643749999898 ) ) ;
#33687 = CARTESIAN_POINT ( 'NONE',  ( 5.137500001229033941, 6.123233995736764310E-16, -4.999999999999998224 ) ) ;
#33688 = CARTESIAN_POINT ( 'NONE',  ( 24.82499999999999929, 6.123233995736764310E-16, -4.999999999999998224 ) ) ;
#33689 = CARTESIAN_POINT ( 'NONE',  ( 27.52500000000000213, 6.123233995736764310E-16, -4.999999999999998224 ) ) ;
#33690 = CARTESIAN_POINT ( 'NONE',  ( 8.428125000614517859, 6.421520780324663323E-16, -5.243569643749999010 ) ) ;
#33691 = CARTESIAN_POINT ( 'NONE',  ( 26.14687500061451431, 0.000000000000000000, 4.756430356249998326 ) ) ;
#33692 = CARTESIAN_POINT ( 'NONE',  ( 18.12187500061451573, 3.027376345333611329, 5.243569643749999010 ) ) ;
#33693 = CARTESIAN_POINT ( 'NONE',  ( 13.32187500061451502, 5.824947211148865298E-16, -4.756430356249998326 ) ) ;
#33694 = CARTESIAN_POINT ( 'NONE',  ( 5.578125000614518214, -4.541064518000419881, 2.621784821874995952 ) ) ;
#33695 = CARTESIAN_POINT ( 'NONE',  ( 10.73437500061451644, 6.421520780324663323E-16, -5.243569643749999010 ) ) ;
#33696 = ORIENTED_EDGE ( 'NONE', *, *, #50010, .F. ) ;
#33697 = CARTESIAN_POINT ( 'NONE',  ( 22.39687500061451075, -3.027376345333610441, -5.243569643749999898 ) ) ;
#33698 = CARTESIAN_POINT ( 'NONE',  ( 3.992467690304758232, 3.010110221998377078, -30.28122918867793700 ) ) ;
#33699 = CARTESIAN_POINT ( 'NONE',  ( 29.92500000000000071, 4.330127018922191873, 2.499999999999999556 ) ) ;
#33700 = CARTESIAN_POINT ( 'NONE',  ( 5.587500000000003020, 5.773502691896255534, 3.535250795749688894E-16 ) ) ;
#33701 = CARTESIAN_POINT ( 'NONE',  ( 15.22500000122903252, 2.886751345948126879, 4.999999999999999112 ) ) ;
#33702 = CARTESIAN_POINT ( 'NONE',  ( 20.64375000122903359, -2.886751345948102898, 5.000000000000044409 ) ) ;
#33703 = CARTESIAN_POINT ( 'NONE',  ( 18.97499999999999787, 6.123233995736764310E-16, -4.999999999999998224 ) ) ;
#33704 = ORIENTED_EDGE ( 'NONE', *, *, #12479, .F. ) ;
#33705 = CARTESIAN_POINT ( 'NONE',  ( 13.01249999999999929, -5.773502691896255534, -1.060575238724906372E-15 ) ) ;
#33706 = CARTESIAN_POINT ( 'NONE',  ( 28.00312500061451715, 0.000000000000000000, 5.243569643749999010 ) ) ;
#33707 = CARTESIAN_POINT ( 'NONE',  ( 16.64999999999999858, -4.330127018922190985, -2.500000000000001332 ) ) ;
#33708 =( BOUNDED_CURVE ( )  B_SPLINE_CURVE ( 1, ( #53031, #57115 ),
 .UNSPECIFIED., .F., .F. ) 
 B_SPLINE_CURVE_WITH_KNOTS ( ( 2, 2 ),
 ( 0.000000000000000000, 1.000000000000000000 ),
 .UNSPECIFIED. ) 
 CURVE ( )  GEOMETRIC_REPRESENTATION_ITEM ( )  RATIONAL_B_SPLINE_CURVE ( ( 0.9401542295229587953, 0.9401542295229587953 ) ) 
 REPRESENTATION_ITEM ( '' )  );
#33709 = CARTESIAN_POINT ( 'NONE',  ( 11.51250000122903216, 4.330127018922192761, -2.499999999999997780 ) ) ;
#33710 = CARTESIAN_POINT ( 'NONE',  ( 9.440625000614517148, 6.054752690667223547, 3.707466751127219781E-16 ) ) ;
#33711 = EDGE_CURVE ( 'NONE', #60995, #37430, #57045, .T. ) ;
#33712 = AXIS2_PLACEMENT_3D ( 'NONE', #47055, #7523, #7890 ) ;
#33713 = CARTESIAN_POINT ( 'NONE',  ( 7.837499999999999467, 5.773502691896255534, 3.535250795749688894E-16 ) ) ;
#33714 = CARTESIAN_POINT ( 'NONE',  ( -5.810221930991193690E-16, 18.98750000000000071, 26.00000000000000355 ) ) ;
#33715 = CARTESIAN_POINT ( 'NONE',  ( -4.243569643749999898, 15.32187500061451679, -32.45002607614398471 ) ) ;
#33716 = CARTESIAN_POINT ( 'NONE',  ( 27.86250000122903359, 0.000000000000000000, 4.999999999999998224 ) ) ;
#33717 = CARTESIAN_POINT ( 'NONE',  ( 1.878215178124997609, 14.81562499938548427, 33.25316411605952993 ) ) ;
#33718 = CARTESIAN_POINT ( 'NONE',  ( 8.025000000000000355, -4.330127018922194537, 2.499999999999995559 ) ) ;
#33719 = CARTESIAN_POINT ( 'NONE',  ( 45.00000000000000000, 0.000000000000000000, 4.999999999999998224 ) ) ;
#33720 = ORIENTED_EDGE ( 'NONE', *, *, #45399, .F. ) ;
#33721 = CARTESIAN_POINT ( 'NONE',  ( 23.99062500061451786, -3.027376345333614438, 5.243569643749998122 ) ) ;
#33722 = CARTESIAN_POINT ( 'NONE',  ( 28.86562500061451786, 3.027376345333611329, 5.243569643749999010 ) ) ;
#33723 = VECTOR ( 'NONE', #35433, 1000.000000000000000 ) ;
#33724 = CARTESIAN_POINT ( 'NONE',  ( 18.86250000122903359, 0.000000000000000000, 4.999999999999998224 ) ) ;
#33725 = CARTESIAN_POINT ( 'NONE',  ( 19.32187500061451857, 3.027376345333613106, -5.243569643749998122 ) ) ;
#33726 = CARTESIAN_POINT ( 'NONE',  ( 17.09062500061451573, 6.054752690667223547, 3.707466751127219781E-16 ) ) ;
#33727 = CARTESIAN_POINT ( 'NONE',  ( 2.121784821875001281, 10.50312500061459531, -26.32496088578401938 ) ) ;
#33728 = CARTESIAN_POINT ( 'NONE',  ( 6.740625000614516082, 6.054752690667223547, 3.707466751127219781E-16 ) ) ;
#33729 = CARTESIAN_POINT ( 'NONE',  ( 29.25000000122903288, -2.886751345948129988, 4.999999999999997335 ) ) ;
#33730 = CARTESIAN_POINT ( 'NONE',  ( 24.94687500061451502, -2.746126346562646425, 4.756430356249996549 ) ) ;
#33731 = CARTESIAN_POINT ( 'NONE',  ( 19.22812500061451502, 6.421520780324663323E-16, -5.243569643749999010 ) ) ;
#33732 = FACE_OUTER_BOUND ( 'NONE', #3906, .T. ) ;
#33733 = CARTESIAN_POINT ( 'NONE',  ( 1.878215178125000495, 18.11562499938548498, 26.74683588394047007 ) ) ;
#33734 = CARTESIAN_POINT ( 'NONE',  ( 13.73437500061451821, -4.541064518000419881, 2.621784821874995952 ) ) ;
#33735 = CARTESIAN_POINT ( 'NONE',  ( 11.82187500061451679, 3.027376345333611329, 5.243569643749999010 ) ) ;
#33736 = CARTESIAN_POINT ( 'NONE',  ( 21.42187500061451644, -6.054752690667223547, -1.112240025338166033E-15 ) ) ;
#33737 = EDGE_LOOP ( 'NONE', ( #51378, #56344, #62599, #7979 ) ) ;
#33738 = CARTESIAN_POINT ( 'NONE',  ( 2.803125000614518747, 0.000000000000000000, 5.243569643749999010 ) ) ;
#33739 = CARTESIAN_POINT ( 'NONE',  ( 25.60312500061451502, 4.541064518000418104, -2.621784821874998173 ) ) ;
#33740 = CARTESIAN_POINT ( 'NONE',  ( 27.06562500061451004, 3.027376345333611329, 5.243569643749999010 ) ) ;
#33741 = CARTESIAN_POINT ( 'NONE',  ( 3.999999999999999112, 12.12500000000000000, -30.00000000000000000 ) ) ;
#33742 = CARTESIAN_POINT ( 'NONE',  ( -2.828200636599751609E-16, 17.63749999999999929, 25.38119784648299770 ) ) ;
#33743 = CARTESIAN_POINT ( 'NONE',  ( 5.709375000614517859, -4.541064518000417216, -2.621784821875001281 ) ) ;
#33744 = CARTESIAN_POINT ( 'NONE',  ( 12.07500000122903216, 2.886751345948126879, 4.999999999999999112 ) ) ;
#33745 = CARTESIAN_POINT ( 'NONE',  ( 6.225000001229036073, 2.886751345948126879, 4.999999999999999112 ) ) ;
#33746 = CARTESIAN_POINT ( 'NONE',  ( 3.815625000614518036, -6.054752690667223547, -1.112240025338166033E-15 ) ) ;
#33747 = CARTESIAN_POINT ( 'NONE',  ( -4.000000000000000888, 18.55624999877096570, 32.30940107675850470 ) ) ;
#33748 = CARTESIAN_POINT ( 'NONE',  ( 17.00625000122903074, 0.000000000000000000, 4.999999999999998224 ) ) ;
#33749 = CARTESIAN_POINT ( 'NONE',  ( 12.08437500061451608, 6.421520780324663323E-16, -5.243569643749999010 ) ) ;
#33750 = CARTESIAN_POINT ( 'NONE',  ( 45.00000000000000000, 0.000000000000000000, 0.000000000000000000 ) ) ;
#33751 = CARTESIAN_POINT ( 'NONE',  ( 18.96562500061451573, 3.027376345333611329, 5.243569643749999010 ) ) ;
#33752 = CARTESIAN_POINT ( 'NONE',  ( 13.54687500061451999, 6.054752690667223547, 3.707466751127219781E-16 ) ) ;
#33753 = CARTESIAN_POINT ( 'NONE',  ( 3.928125000614516527, 6.421520780324663323E-16, -5.243569643749999010 ) ) ;
#33754 = CARTESIAN_POINT ( 'NONE',  ( 22.32187500061451857, -6.054752690667223547, -1.112240025338166033E-15 ) ) ;
#33755 = CARTESIAN_POINT ( 'NONE',  ( 10.05937500061451750, 0.000000000000000000, 5.243569643749999010 ) ) ;
#33756 = CARTESIAN_POINT ( 'NONE',  ( 4.078125000614517326, 4.541064518000418104, 2.621784821874999949 ) ) ;
#33757 = CARTESIAN_POINT ( 'NONE',  ( 1.138803498474273873E-14, 15.98750000000000249, 34.00000000000000000 ) ) ;
#33758 = CARTESIAN_POINT ( 'NONE',  ( 4.875000001229034652, 2.886751345948126879, 4.999999999999999112 ) ) ;
#33759 = CARTESIAN_POINT ( 'NONE',  ( 20.57812500061451644, 6.421520780324663323E-16, -5.243569643749999010 ) ) ;
#33760 = CARTESIAN_POINT ( 'NONE',  ( 8.437500001229034652, 4.330127018922191873, 2.499999999999999556 ) ) ;
#33761 = CARTESIAN_POINT ( 'NONE',  ( 16.49062500061451786, -3.027376345333610441, -5.243569643749999898 ) ) ;
#33762 = VECTOR ( 'NONE', #47375, 1000.000000000000000 ) ;
#33763 = CARTESIAN_POINT ( 'NONE',  ( 15.81562500061451537, 3.027376345333611329, 5.243569643749999010 ) ) ;
#33764 = CARTESIAN_POINT ( 'NONE',  ( 25.73437500061451644, 4.119189519843966529, 2.378215178124999607 ) ) ;
#33765 = CARTESIAN_POINT ( 'NONE',  ( 16.08749999999999503, -2.886751345948129988, 4.999999999999997335 ) ) ;
#33766 = CARTESIAN_POINT ( 'NONE',  ( 9.225000001229034297, 2.886751345948129099, -4.999999999999998224 ) ) ;
#33767 = ADVANCED_FACE ( 'NONE', ( #2001 ), #42239, .F. ) ;
#33768 = CARTESIAN_POINT ( 'NONE',  ( 4.940625000614515372, 6.054752690667223547, 3.707466751127219781E-16 ) ) ;
#33769 =( BOUNDED_CURVE ( )  B_SPLINE_CURVE ( 2, ( #66403, #37956, #8787, #70847, #60476, #54956, #32056, #20220, #42775 ),
 .UNSPECIFIED., .F., .F. ) 
 B_SPLINE_CURVE_WITH_KNOTS ( ( 3, 2, 2, 2, 3 ),
 ( 0.5416666666666667407, 0.5462962962962962798, 0.5555555555555555802, 0.5648148148148147696, 0.5694444444444444198 ),
 .UNSPECIFIED. ) 
 CURVE ( )  GEOMETRIC_REPRESENTATION_ITEM ( )  RATIONAL_B_SPLINE_CURVE ( ( 0.9330127018922192983, 0.9330127018922200755, 1.000000000000000000, 0.8660254037844387076, 1.000000000000000000, 0.8660254037844387076, 1.000000000000000000, 0.9330127018922194093, 0.9330127018922194093 ) ) 
 REPRESENTATION_ITEM ( '' )  );
#33770 = CARTESIAN_POINT ( 'NONE',  ( 20.17500000122903359, 2.886751345948126879, 4.999999999999999112 ) ) ;
#33771 = CARTESIAN_POINT ( 'NONE',  ( 28.12499999999999645, 4.330127018922191873, 2.499999999999999556 ) ) ;
#33772 = CARTESIAN_POINT ( 'NONE',  ( -4.243569643749997233, 12.24687500061451928, -27.54997392385601174 ) ) ;
#33773 = CARTESIAN_POINT ( 'NONE',  ( 9.862499999999997158, -5.773502691896255534, -1.060575238724906372E-15 ) ) ;
#33774 = CARTESIAN_POINT ( 'NONE',  ( 0.000000000000000000, 20.00000000000000000, -30.00000000000000000 ) ) ;
#33775 = FACE_OUTER_BOUND ( 'NONE', #37795, .T. ) ;
#33776 = CARTESIAN_POINT ( 'NONE',  ( 21.75937500061451502, 0.000000000000000000, 5.243569643749999010 ) ) ;
#33777 = CARTESIAN_POINT ( 'NONE',  ( 12.44999999999999929, 0.000000000000000000, 4.999999999999998224 ) ) ;
#33778 = CARTESIAN_POINT ( 'NONE',  ( 17.65312500061451573, 0.000000000000000000, 5.243569643749999010 ) ) ;
#33779 = CARTESIAN_POINT ( 'NONE',  ( 11.71875000122903465, -5.773502691896255534, -1.060575238724906372E-15 ) ) ;
#33780 = CARTESIAN_POINT ( 'NONE',  ( 11.10000000000000142, 0.000000000000000000, 4.999999999999998224 ) ) ;
#33781 = CARTESIAN_POINT ( 'NONE',  ( 13.85625000122903216, 0.000000000000000000, 4.999999999999998224 ) ) ;
#33782 = CARTESIAN_POINT ( 'NONE',  ( 27.90937500061451715, 4.541064518000418104, -2.621784821874998173 ) ) ;
#33783 = CARTESIAN_POINT ( 'NONE',  ( 21.72187500061451715, -4.119189519843968306, 2.378215178124996054 ) ) ;
#33784 = CARTESIAN_POINT ( 'NONE',  ( 12.51562500061451821, 3.027376345333613106, -5.243569643749998122 ) ) ;
#33785 = CARTESIAN_POINT ( 'NONE',  ( 10.88437500061451679, 4.541064518000418104, 2.621784821874999949 ) ) ;
#33786 = ORIENTED_EDGE ( 'NONE', *, *, #40515, .F. ) ;
#33787 = CARTESIAN_POINT ( 'NONE',  ( -3.999999999999999112, 14.11250000000000071, -32.30940107675850470 ) ) ;
#33788 = CARTESIAN_POINT ( 'NONE',  ( 23.42812500061451786, 4.541064518000418104, 2.621784821874999949 ) ) ;
#33789 = CARTESIAN_POINT ( 'NONE',  ( 27.75000000000000000, 0.000000000000000000, 4.999999999999998224 ) ) ;
#33790 = CARTESIAN_POINT ( 'NONE',  ( 10.93125000122903501, 6.123233995736764310E-16, -4.999999999999998224 ) ) ;
#33791 = CARTESIAN_POINT ( 'NONE',  ( 13.08750000000000036, -2.886751345948125991, -5.000000000000000000 ) ) ;
#33792 = CARTESIAN_POINT ( 'NONE',  ( 21.07500000122903572, 2.886751345948126879, 4.999999999999999112 ) ) ;
#33793 = CARTESIAN_POINT ( 'NONE',  ( 15.85312500061451857, 0.000000000000000000, 5.243569643749999010 ) ) ;
#33794 = CARTESIAN_POINT ( 'NONE',  ( 12.57187500061451502, 4.119189519843966529, 2.378215178124999607 ) ) ;
#33795 = VERTEX_POINT ( 'NONE', #35237 ) ;
#33796 = CARTESIAN_POINT ( 'NONE',  ( 20.92500000000000071, 4.330127018922191873, 2.499999999999999556 ) ) ;
#33797 = CARTESIAN_POINT ( 'NONE',  ( 24.33749999999999858, -2.886751345948125991, -5.000000000000000000 ) ) ;
#33798 = CARTESIAN_POINT ( 'NONE',  ( 21.83437500061451786, -4.541064518000419881, 2.621784821874995952 ) ) ;
#33799 = CARTESIAN_POINT ( 'NONE',  ( 24.10312500061451502, -4.541064518000417216, -2.621784821875001281 ) ) ;
#33800 = ORIENTED_EDGE ( 'NONE', *, *, #24709, .F. ) ;
#33801 = CARTESIAN_POINT ( 'NONE',  ( 21.16875000122903216, -5.773502691896255534, -1.060575238724906372E-15 ) ) ;
#33802 = CARTESIAN_POINT ( 'NONE',  ( 7.903125000614515727, -4.541064518000417216, -2.621784821875001281 ) ) ;
#33803 = LINE ( 'NONE', #56347, #39480 ) ;
#33804 = VECTOR ( 'NONE', #51388, 1000.000000000000000 ) ;
#33805 = CARTESIAN_POINT ( 'NONE',  ( 14.96250000000000036, 2.886751345948129099, -4.999999999999998224 ) ) ;
#33806 = CARTESIAN_POINT ( 'NONE',  ( 3.578157825243565515, -3.492515161539162527, -3.678572976455726895 ) ) ;
#33807 = CARTESIAN_POINT ( 'NONE',  ( 5.034375000614519813, 4.541064518000418104, 2.621784821874999949 ) ) ;
#33808 = CARTESIAN_POINT ( 'NONE',  ( 28.35937500061451289, 4.541064518000418104, -2.621784821874998173 ) ) ;
#33809 = ORIENTED_EDGE ( 'NONE', *, *, #36205, .F. ) ;
#33810 = CARTESIAN_POINT ( 'NONE',  ( 24.81562500061451715, 3.027376345333611329, 5.243569643749999010 ) ) ;
#33811 = CARTESIAN_POINT ( 'NONE',  ( 25.88437500061451502, -4.541064518000419881, 2.621784821874995952 ) ) ;
#33812 = CARTESIAN_POINT ( 'NONE',  ( -2.121784821874999949, 17.92812500061459602, -33.67503911421598417 ) ) ;
#33813 = CARTESIAN_POINT ( 'NONE',  ( 11.10000000000000142, 0.000000000000000000, 4.999999999999998224 ) ) ;
#33814 = CARTESIAN_POINT ( 'NONE',  ( 8.540625000614518569, 6.054752690667223547, 3.707466751127219781E-16 ) ) ;
#33815 = CARTESIAN_POINT ( 'NONE',  ( 7.162500000000001421, -5.773502691896255534, -1.060575238724906372E-15 ) ) ;
#33816 = CARTESIAN_POINT ( 'NONE',  ( 26.05312500061451431, 4.541064518000418104, -2.621784821874998173 ) ) ;
#33817 = CARTESIAN_POINT ( 'NONE',  ( 7.320879633048903241E-15, 18.20000000122903216, -34.00000000000000000 ) ) ;
#33818 = CARTESIAN_POINT ( 'NONE',  ( 13.92187500061451644, 2.746126346562645981, -4.756430356249997438 ) ) ;
#33819 = CARTESIAN_POINT ( 'NONE',  ( 3.065625000614517592, 3.027376345333613106, -5.243569643749998122 ) ) ;
#33820 = CARTESIAN_POINT ( 'NONE',  ( 19.09687500061451360, -3.027376345333614438, 5.243569643749998122 ) ) ;
#33821 = CARTESIAN_POINT ( 'NONE',  ( 4.243569643749999010, 15.17187500061451644, 27.54997392385601174 ) ) ;
#33822 = EDGE_CURVE ( 'NONE', #29028, #17531, #5416, .T. ) ;
#33823 = CARTESIAN_POINT ( 'NONE',  ( 20.85937500061451644, 0.000000000000000000, 5.243569643749999010 ) ) ;
#33824 = CARTESIAN_POINT ( 'NONE',  ( 3.337499999999999911, 5.773502691896255534, 3.535250795749688894E-16 ) ) ;
#33825 = CARTESIAN_POINT ( 'NONE',  ( -2.121784821874996840, 19.48437500061451644, 33.67503911421598417 ) ) ;
#33826 = CARTESIAN_POINT ( 'NONE',  ( 9.628125000614517148, -4.541064518000419881, 2.621784821874995952 ) ) ;
#33827 = DIRECTION ( 'NONE',  ( -1.000000000000000000, 0.000000000000000000, 0.000000000000000000 ) ) ;
#33828 = CARTESIAN_POINT ( 'NONE',  ( 5.896875000614518747, 6.054752690667223547, 3.707466751127219781E-16 ) ) ;
#33829 = DIRECTION ( 'NONE',  ( -0.000000000000000000, -1.000000000000000000, -0.000000000000000000 ) ) ;
#33830 = CARTESIAN_POINT ( 'NONE',  ( 6.553125000614518747, -4.541064518000417216, -2.621784821875001281 ) ) ;
#33831 = CARTESIAN_POINT ( 'NONE',  ( 12.94687500061451857, -3.027376345333610441, -5.243569643749999898 ) ) ;
#33832 =( LENGTH_UNIT ( ) NAMED_UNIT ( * ) SI_UNIT ( .MILLI., .METRE. ) );
#33833 = CARTESIAN_POINT ( 'NONE',  ( 18.22500000122903430, 2.886751345948129099, -4.999999999999998224 ) ) ;
#33834 = CARTESIAN_POINT ( 'NONE',  ( 6.984375000614516438, -4.541064518000419881, 2.621784821874995952 ) ) ;
#33835 = CARTESIAN_POINT ( 'NONE',  ( 8.953125000614518214, 4.541064518000418104, -2.621784821874998173 ) ) ;
#33836 = CARTESIAN_POINT ( 'NONE',  ( 4.178128910459903089, -3.728570022149966690, -3.541927282058038973 ) ) ;
#33837 = CARTESIAN_POINT ( 'NONE',  ( 26.26875000122903359, 2.886751345948129099, -4.999999999999998224 ) ) ;
#33838 = CARTESIAN_POINT ( 'NONE',  ( 20.14687500061451786, -3.027376345333610441, -5.243569643749999898 ) ) ;
#33839 = CARTESIAN_POINT ( 'NONE',  ( 9.037500001229034297, -4.330127018922194537, 2.499999999999995559 ) ) ;
#33840 = CARTESIAN_POINT ( 'NONE',  ( 27.14062500061451644, -3.027376345333614438, 5.243569643749998122 ) ) ;
#33841 = CARTESIAN_POINT ( 'NONE',  ( 11.54062500061451857, -3.027376345333610441, -5.243569643749999898 ) ) ;
#33842 = CARTESIAN_POINT ( 'NONE',  ( 29.70937500061451431, 4.541064518000418104, -2.621784821874998173 ) ) ;
#33843 = CARTESIAN_POINT ( 'NONE',  ( 4.243569643749999898, 10.14687500061451786, -27.54997392385601529 ) ) ;
#33844 = CARTESIAN_POINT ( 'NONE',  ( 13.50000000122903288, -2.886751345948129988, 4.999999999999997335 ) ) ;
#33845 = CARTESIAN_POINT ( 'NONE',  ( 27.85312500061451502, 4.541064518000418104, -2.621784821874998173 ) ) ;
#33846 = CARTESIAN_POINT ( 'NONE',  ( -2.121784821874999949, 16.12812500061451715, -33.67503911421598417 ) ) ;
#33847 = CARTESIAN_POINT ( 'NONE',  ( 14.51250000122903394, -4.330127018922190985, -2.500000000000001332 ) ) ;
#33848 = CARTESIAN_POINT ( 'NONE',  ( 12.26249999999999929, 2.886751345948129099, -4.999999999999998224 ) ) ;
#33849 = CARTESIAN_POINT ( 'NONE',  ( 23.09062500061451573, -3.027376345333614438, 5.243569643749998122 ) ) ;
#33850 = CARTESIAN_POINT ( 'NONE',  ( 8.334375000614516082, -4.541064518000419881, 2.621784821874995952 ) ) ;
#33851 = CARTESIAN_POINT ( 'NONE',  ( 8.737500001229033586, 6.123233995736764310E-16, -4.999999999999998224 ) ) ;
#33852 = CARTESIAN_POINT ( 'NONE',  ( 16.08750000122903501, 4.330127018922191873, 2.499999999999999556 ) ) ;
#33853 = CARTESIAN_POINT ( 'NONE',  ( 13.41562500061451502, 3.027376345333613106, -5.243569643749998122 ) ) ;
#33854 = CARTESIAN_POINT ( 'NONE',  ( 16.11562500061451786, 3.027376345333613106, -5.243569643749998122 ) ) ;
#33855 = CARTESIAN_POINT ( 'NONE',  ( 27.90000000122903145, -2.886751345948129988, 4.999999999999997335 ) ) ;
#33856 = CARTESIAN_POINT ( 'NONE',  ( 22.19999999999999574, 4.330127018922192761, -2.499999999999997780 ) ) ;
#33857 = CARTESIAN_POINT ( 'NONE',  ( 23.10937500061451644, 0.000000000000000000, 5.243569643749999010 ) ) ;
#33858 = CARTESIAN_POINT ( 'NONE',  ( 18.26250000122903216, 4.330127018922192761, -2.499999999999997780 ) ) ;
#33859 = EDGE_CURVE ( 'NONE', #55447, #16877, #52580, .T. ) ;
#33860 = CARTESIAN_POINT ( 'NONE',  ( 10.98750000122903536, 6.123233995736764310E-16, -4.999999999999998224 ) ) ;
#33861 = CARTESIAN_POINT ( 'NONE',  ( 28.02187500061451431, 3.027376345333611329, 5.243569643749999010 ) ) ;
#33862 = CARTESIAN_POINT ( 'NONE',  ( 4.771875000614516971, -6.054752690667223547, -1.112240025338166033E-15 ) ) ;
#33863 = CARTESIAN_POINT ( 'NONE',  ( 22.49062500061451431, 6.054752690667223547, 3.707466751127219781E-16 ) ) ;
#33864 = CARTESIAN_POINT ( 'NONE',  ( -3.756430356249999214, 15.64062499938548356, 27.83122392262697176 ) ) ;
#33865 = CARTESIAN_POINT ( 'NONE',  ( -1.243387493232115393E-14, 15.25624999877096677, 26.00000000000000000 ) ) ;
#33866 = CARTESIAN_POINT ( 'NONE',  ( 9.271875000614516082, -6.054752690667223547, -1.112240025338166033E-15 ) ) ;
#33867 = LINE ( 'NONE', #16510, #1785 ) ;
#33868 = CARTESIAN_POINT ( 'NONE',  ( 29.31562500061451715, 3.027376345333611329, 5.243569643749999010 ) ) ;
#33869 = CARTESIAN_POINT ( 'NONE',  ( 6.009375000614519458, 0.000000000000000000, 5.243569643749999010 ) ) ;
#33870 = CARTESIAN_POINT ( 'NONE',  ( 25.91249999999999787, 2.886751345948093572, 5.000000000000056843 ) ) ;
#33871 = CARTESIAN_POINT ( 'NONE',  ( 28.73437500061451644, 6.421520780324663323E-16, -5.243569643749999010 ) ) ;
#33872 = CARTESIAN_POINT ( 'NONE',  ( -4.243569643749999898, 10.80312500061459602, 30.00000000000000000 ) ) ;
#33873 = CARTESIAN_POINT ( 'NONE',  ( 19.65000000000000213, 0.000000000000000000, 4.999999999999998224 ) ) ;
#33874 = ORIENTED_EDGE ( 'NONE', *, *, #64752, .T. ) ;
#33875 = CARTESIAN_POINT ( 'NONE',  ( 27.11249999999999716, 2.886751345948129099, -4.999999999999998224 ) ) ;
#33876 = CARTESIAN_POINT ( 'NONE',  ( 28.02187500061451431, 3.027376345333611329, 5.243569643749999010 ) ) ;
#33877 = EDGE_LOOP ( 'NONE', ( #50649, #17523, #33061, #197 ) ) ;
#33878 = CARTESIAN_POINT ( 'NONE',  ( 15.36562500061451608, 3.027376345333611329, 5.243569643749999010 ) ) ;
#33879 = CARTESIAN_POINT ( 'NONE',  ( 9.403125000614517504, 4.541064518000418104, -2.621784821874998173 ) ) ;
#33880 = CARTESIAN_POINT ( 'NONE',  ( 18.98437500061451289, -2.746126346562646425, 4.756430356249996549 ) ) ;
#33881 = CARTESIAN_POINT ( 'NONE',  ( 3.684375000614518836, 4.541064518000418104, 2.621784821874999949 ) ) ;
#33882 = CARTESIAN_POINT ( 'NONE',  ( 17.81250000122903288, 4.330127018922192761, -2.499999999999997780 ) ) ;
#33883 = CARTESIAN_POINT ( 'NONE',  ( 22.76249999999999574, 2.886751345948126879, 4.999999999999999112 ) ) ;
#33884 = LINE ( 'NONE', #60868, #23231 ) ;
#33885 = CARTESIAN_POINT ( 'NONE',  ( 6.759375000614516793, 4.541064518000418104, -2.621784821874998173 ) ) ;
#33886 = CARTESIAN_POINT ( 'NONE',  ( 10.65937500061451715, -4.541064518000417216, -2.621784821875001281 ) ) ;
#33887 = CARTESIAN_POINT ( 'NONE',  ( 22.54687500061451999, 6.054752690667223547, 3.707466751127219781E-16 ) ) ;
#33888 = CARTESIAN_POINT ( 'NONE',  ( -1.071796769724504328, 14.69240381056766687, -26.00000000000001066 ) ) ;
#33889 = VERTEX_POINT ( 'NONE', #46695 ) ;
#33890 = CARTESIAN_POINT ( 'NONE',  ( 3.496875000614518836, -3.027376345333610441, -5.243569643749999898 ) ) ;
#33891 = CARTESIAN_POINT ( 'NONE',  ( 5.971875000614516260, 3.027376345333611329, 5.243569643749999010 ) ) ;
#33892 = CARTESIAN_POINT ( 'NONE',  ( 18.86249999999999716, -5.773502691896255534, -1.060575238724906372E-15 ) ) ;
#33893 = CARTESIAN_POINT ( 'NONE',  ( 16.26562500061451289, 3.027376345333611329, 5.243569643749999010 ) ) ;
#33894 = CARTESIAN_POINT ( 'NONE',  ( -1.999999999999999112, 18.50000000000000000, 26.53589838486224650 ) ) ;
#33895 = ADVANCED_FACE ( 'NONE', ( #19315 ), #69589, .F. ) ;
#33896 = CARTESIAN_POINT ( 'NONE',  ( 21.38437500061451502, -4.119189519843968306, 2.378215178124996054 ) ) ;
#33897 = CARTESIAN_POINT ( 'NONE',  ( 9.590625000614517504, -3.027376345333614438, 5.243569643749998122 ) ) ;
#33898 = CARTESIAN_POINT ( 'NONE',  ( 26.82187500061451857, -6.054752690667223547, -1.112240025338166033E-15 ) ) ;
#33899 = CARTESIAN_POINT ( 'NONE',  ( 12.75000000000000178, 4.330127018922192761, -2.499999999999997780 ) ) ;
#33900 = CARTESIAN_POINT ( 'NONE',  ( 28.80937500061451573, 4.541064518000418104, -2.621784821874998173 ) ) ;
#33901 = CARTESIAN_POINT ( 'NONE',  ( 8.887499999999999289, -2.886751345948129988, 4.999999999999997335 ) ) ;
#33902 = CARTESIAN_POINT ( 'NONE',  ( -3.999999999999999556, 16.02500000122903501, 27.69059892324149530 ) ) ;
#33903 = CARTESIAN_POINT ( 'NONE',  ( 9.637500001229033941, 6.123233995736764310E-16, -4.999999999999998224 ) ) ;
#33904 = CARTESIAN_POINT ( 'NONE',  ( 18.87187500061451573, 3.027376345333613106, -5.243569643749998122 ) ) ;
#33905 = CARTESIAN_POINT ( 'NONE',  ( 13.39687500061451608, -3.027376345333610441, -5.243569643749999898 ) ) ;
#33906 = CARTESIAN_POINT ( 'NONE',  ( -3.578127771932956058, 3.495591672637165637, -28.19363475146253251 ) ) ;
#33907 = VERTEX_POINT ( 'NONE', #25231 ) ;
#33908 = CARTESIAN_POINT ( 'NONE',  ( 13.67812500061451786, -4.541064518000419881, 2.621784821874995952 ) ) ;
#33909 = CARTESIAN_POINT ( 'NONE',  ( 26.40000000122902790, 5.773502691896255534, 3.535250795749688894E-16 ) ) ;
#33910 = CARTESIAN_POINT ( 'NONE',  ( 15.57187500061451679, -6.054752690667223547, -1.112240025338166033E-15 ) ) ;
#33911 = B_SPLINE_CURVE_WITH_KNOTS ( 'NONE', 3,
 ( #14505, #19301, #25216, #3809, #41854, #30770, #47763, #8604, #20033, #71029 ),
 .UNSPECIFIED., .F., .F.,
 ( 4, 3, 3, 4 ),
 ( 0.000000000000000000, 2.812508172722986163E-05, 5.625016478268387503E-05, 0.0001066165372333795924 ),
 .UNSPECIFIED. ) ;
#33912 = CARTESIAN_POINT ( 'NONE',  ( 4.763386231524737724, 8.796087519298451340, -33.66842538561026288 ) ) ;
#33913 = CARTESIAN_POINT ( 'NONE',  ( 17.72812500061451502, -4.541064518000419881, 2.621784821874995952 ) ) ;
#33914 = FACE_BOUND ( 'NONE', #12788, .T. ) ;
#33915 = CARTESIAN_POINT ( 'NONE',  ( 26.22187500061451715, 3.027376345333611329, 5.243569643749999010 ) ) ;
#33916 = CARTESIAN_POINT ( 'NONE',  ( -3.000416591977282496E-16, 10.69062500061451715, 25.09994784771203058 ) ) ;
#33917 = CARTESIAN_POINT ( 'NONE',  ( 15.57187500061451679, -6.054752690667223547, -1.112240025338166033E-15 ) ) ;
#33918 = CARTESIAN_POINT ( 'NONE',  ( 13.95000000122903572, -2.886751345948129988, 4.999999999999997335 ) ) ;
#33919 = CARTESIAN_POINT ( 'NONE',  ( 8.146875000614516082, 5.492252693125287522, 3.363034840372157021E-16 ) ) ;
#33920 = CARTESIAN_POINT ( 'NONE',  ( 4.243569643749999898, 18.69687500061451857, -27.54997392385601529 ) ) ;
#33921 =( BOUNDED_CURVE ( )  B_SPLINE_CURVE ( 2, ( #2036, #36724, #13826, #41909, #69982, #47092, #14556 ),
 .UNSPECIFIED., .F., .F. ) 
 B_SPLINE_CURVE_WITH_KNOTS ( ( 3, 2, 2, 3 ),
 ( 0.9514076071890844588, 0.9527777777777777235, 0.9555555555555556024, 0.9567839273083657003 ),
 .UNSPECIFIED. ) 
 CURVE ( )  GEOMETRIC_REPRESENTATION_ITEM ( )  RATIONAL_B_SPLINE_CURVE ( ( 0.9330248690816613788, 0.9339155015080172761, 1.000000000000000000, 0.8660254037844387076, 1.000000000000000000, 0.9407545805492795177, 0.9339074489089478348 ) ) 
 REPRESENTATION_ITEM ( '' )  );
#33922 = CARTESIAN_POINT ( 'NONE',  ( 18.68437500061451928, -4.541064518000419881, 2.621784821874995952 ) ) ;
#33923 = CARTESIAN_POINT ( 'NONE',  ( 20.32500000122903572, -5.773502691896255534, -1.060575238724906372E-15 ) ) ;
#33924 = CARTESIAN_POINT ( 'NONE',  ( 15.12187500061451750, -6.054752690667223547, -1.112240025338166033E-15 ) ) ;
#33925 = CARTESIAN_POINT ( 'NONE',  ( 2.121784821875001281, 11.90937500061451892, 33.67503911421598417 ) ) ;
#33926 = CARTESIAN_POINT ( 'NONE',  ( 22.38750000122903216, 4.330127018922191873, 2.499999999999999556 ) ) ;
#33927 = CARTESIAN_POINT ( 'NONE',  ( 14.84062500061451750, 6.054752690667223547, 3.707466751127219781E-16 ) ) ;
#33928 = VERTEX_POINT ( 'NONE', #14153 ) ;
#33929 = ORIENTED_EDGE ( 'NONE', *, *, #41045, .T. ) ;
#33930 = CARTESIAN_POINT ( 'NONE',  ( 21.75000000000000000, 4.330127018922192761, -2.499999999999997780 ) ) ;
#33931 = DIRECTION ( 'NONE',  ( 1.000000000000000000, 0.000000000000000000, 0.000000000000000000 ) ) ;
#33932 = CARTESIAN_POINT ( 'NONE',  ( 3.140625000614516882, 6.054752690667223547, 3.707466751127219781E-16 ) ) ;
#33933 = CARTESIAN_POINT ( 'NONE',  ( 16.20000000122903216, -2.886751345948129988, 4.999999999999997335 ) ) ;
#33934 = CARTESIAN_POINT ( 'NONE',  ( 21.02812500061451573, 6.421520780324663323E-16, -5.243569643749999010 ) ) ;
#33935 = CARTESIAN_POINT ( 'NONE',  ( 25.26562500061451289, 3.027376345333611329, 5.243569643749999010 ) ) ;
#33936 = CARTESIAN_POINT ( 'NONE',  ( 4.715625000614516615, -6.054752690667223547, -1.112240025338166033E-15 ) ) ;
#33937 = CARTESIAN_POINT ( 'NONE',  ( 29.21249999999999858, -5.773502691896255534, -1.060575238724906372E-15 ) ) ;
#33938 = CARTESIAN_POINT ( 'NONE',  ( -4.000000000000000888, 13.15624999877096535, 32.30940107675850470 ) ) ;
#33939 = CARTESIAN_POINT ( 'NONE',  ( 9.384375000614518569, 5.824947211148865298E-16, -4.756430356249998326 ) ) ;
#33940 = DIRECTION ( 'NONE',  ( -1.000000000000000000, -0.000000000000000000, -0.000000000000000000 ) ) ;
#33941 = CARTESIAN_POINT ( 'NONE',  ( 2.000000000000001332, 10.81250000122903465, -26.53589838486224650 ) ) ;
#33942 = CARTESIAN_POINT ( 'NONE',  ( -2.121784821874996840, 17.68437500061451928, -26.32496088578401583 ) ) ;
#33943 = CARTESIAN_POINT ( 'NONE',  ( 5.287500001229035185, 4.330127018922191873, 2.499999999999999556 ) ) ;
#33944 = AXIS2_PLACEMENT_3D ( 'NONE', #73003, #6851, #61910 ) ;
#33945 = CARTESIAN_POINT ( 'NONE',  ( 7.162500000000001421, -5.773502691896255534, -1.060575238724906372E-15 ) ) ;
#33946 = EDGE_CURVE ( 'NONE', #24236, #60873, #36761, .T. ) ;
#33947 = CARTESIAN_POINT ( 'NONE',  ( 3.862500001229035362, 4.330127018922192761, -2.499999999999997780 ) ) ;
#33948 = CARTESIAN_POINT ( 'NONE',  ( 11.33437500061451608, 4.541064518000418104, 2.621784821874999949 ) ) ;
#33949 = LINE ( 'NONE', #50237, #63071 ) ;
#33950 = CARTESIAN_POINT ( 'NONE',  ( 3.628125000614518036, 4.541064518000418104, 2.621784821874999949 ) ) ;
#33951 = CARTESIAN_POINT ( 'NONE',  ( 29.85937500061451644, 0.000000000000000000, 4.756430356249998326 ) ) ;
#33952 = CARTESIAN_POINT ( 'NONE',  ( -5.810221930991193690E-16, 10.88750000000000107, -34.00000000000000000 ) ) ;
#33953 = CARTESIAN_POINT ( 'NONE',  ( 10.13437500061451679, -4.541064518000419881, 2.621784821874995952 ) ) ;
#33954 = CARTESIAN_POINT ( 'NONE',  ( -1.071796769724487453, 18.55759618943233491, -34.00000000000000000 ) ) ;
#33955 = CARTESIAN_POINT ( 'NONE',  ( 4.000000000000000000, 14.33750000000000213, 32.30940107675849760 ) ) ;
#33956 =( BOUNDED_CURVE ( )  B_SPLINE_CURVE ( 2, ( #44203, #72996, #33102, #39753, #56716, #28648, #71907, #72634, #22018 ),
 .UNSPECIFIED., .F., .F. ) 
 B_SPLINE_CURVE_WITH_KNOTS ( ( 3, 2, 2, 2, 3 ),
 ( 0.2282608695652174058, 0.2318840579710144956, 0.2391304347826087029, 0.2463768115942029102, 0.2500000000000000000 ),
 .UNSPECIFIED. ) 
 CURVE ( )  GEOMETRIC_REPRESENTATION_ITEM ( )  RATIONAL_B_SPLINE_CURVE ( ( 0.9330127018922194093, 0.9330127018922196314, 1.000000000000000000, 0.8660254037844387076, 1.000000000000000000, 0.8660254037844387076, 1.000000000000000000, 0.9330127018922196314, 0.9330127018922194093 ) ) 
 REPRESENTATION_ITEM ( '' )  );
#33957 = CARTESIAN_POINT ( 'NONE',  ( -4.243569643749999898, 16.61562500061459247, 27.54997392385601529 ) ) ;
#33958 = CARTESIAN_POINT ( 'NONE',  ( 21.60937500061451644, 4.541064518000418104, -2.621784821874998173 ) ) ;
#33959 = CARTESIAN_POINT ( 'NONE',  ( 2.771473848796851769, -4.161669585790501280, 2.894079486085709529 ) ) ;
#33960 =( BOUNDED_CURVE ( )  B_SPLINE_CURVE ( 2, ( #72051, #17342, #62414, #72413, #16613, #32891, #39901 ),
 .UNSPECIFIED., .F., .F. ) 
 B_SPLINE_CURVE_WITH_KNOTS ( ( 3, 2, 2, 3 ),
 ( 0.3599999999999999867, 0.3633333333333333415, 0.3666666666666666408, 0.3699999999999999956 ),
 .UNSPECIFIED. ) 
 CURVE ( )  GEOMETRIC_REPRESENTATION_ITEM ( )  RATIONAL_B_SPLINE_CURVE ( ( 1.000000000000000000, 0.8660254037844387076, 1.000000000000000000, 0.8660254037844387076, 1.000000000000000000, 0.8660254037844387076, 1.000000000000000000 ) ) 
 REPRESENTATION_ITEM ( '' )  );
#33961 = CARTESIAN_POINT ( 'NONE',  ( 27.82500000122903572, 2.886751345948126879, 4.999999999999999112 ) ) ;
#33962 = CARTESIAN_POINT ( 'NONE',  ( 17.44687500061451502, 4.119189519843966529, -2.378215178124998275 ) ) ;
#33963 = CARTESIAN_POINT ( 'NONE',  ( 23.42812500061451786, 4.541064518000418104, 2.621784821874999949 ) ) ;
#33964 = CARTESIAN_POINT ( 'NONE',  ( 15.44062500061451537, -3.027376345333614438, 5.243569643749998122 ) ) ;
#33965 = CARTESIAN_POINT ( 'NONE',  ( 13.03125000122903110, -4.330127018922194537, 2.499999999999995559 ) ) ;
#33966 = CARTESIAN_POINT ( 'NONE',  ( 12.42187500061451821, -6.054752690667223547, -1.112240025338166033E-15 ) ) ;
#33967 = CARTESIAN_POINT ( 'NONE',  ( 28.38749999999999929, -2.886751345948125991, -5.000000000000000000 ) ) ;
#33968 = CARTESIAN_POINT ( 'NONE',  ( 25.65000000122903145, -2.886751345948129988, 4.999999999999997335 ) ) ;
#33969 = CARTESIAN_POINT ( 'NONE',  ( 3.271875000614519635, 3.027376345333611329, 5.243569643749999010 ) ) ;
#33970 = CARTESIAN_POINT ( 'NONE',  ( 13.92187500061451644, 3.027376345333613106, -5.243569643749998122 ) ) ;
#33971 = FACE_OUTER_BOUND ( 'NONE', #70757, .T. ) ;
#33972 = CARTESIAN_POINT ( 'NONE',  ( 8.287500001229034297, 6.123233995736764310E-16, -4.999999999999998224 ) ) ;
#33973 = CARTESIAN_POINT ( 'NONE',  ( -3.999999999999997335, 12.05000000122903359, 32.30940107675850470 ) ) ;
#33974 = CARTESIAN_POINT ( 'NONE',  ( 22.32187500061451502, -6.054752690667223547, -1.112240025338166033E-15 ) ) ;
#33975 = CARTESIAN_POINT ( 'NONE',  ( 15.19687500061451857, -3.027376345333610441, -5.243569643749999898 ) ) ;
#33976 = CARTESIAN_POINT ( 'NONE',  ( 1.878215178124997609, 17.17812499938548498, 33.25316411605952993 ) ) ;
#33977 = CARTESIAN_POINT ( 'NONE',  ( 27.18750000000000000, 5.773502691896255534, 3.535250795749688894E-16 ) ) ;
#33978 = CARTESIAN_POINT ( 'NONE',  ( 3.525000001229034119, 2.886751345948126879, 4.999999999999999112 ) ) ;
#33979 = CARTESIAN_POINT ( 'NONE',  ( 29.10937500061451644, -4.119189519843965641, -2.378215178125001383 ) ) ;
#33980 = CARTESIAN_POINT ( 'NONE',  ( 16.52812500061451573, 6.421520780324663323E-16, -5.243569643749999010 ) ) ;
#33981 = CARTESIAN_POINT ( 'NONE',  ( 6.487499999999999822, 5.773502691896255534, 3.535250795749688894E-16 ) ) ;
#33982 = DIRECTION ( 'NONE',  ( 0.000000000000000000, 0.000000000000000000, -1.000000000000000000 ) ) ;
#33983 = CARTESIAN_POINT ( 'NONE',  ( 17.96250000000000213, -5.773502691896255534, -1.060575238724906372E-15 ) ) ;
#33984 = EDGE_CURVE ( 'NONE', #20497, #16648, #47125, .T. ) ;
#33985 = CARTESIAN_POINT ( 'NONE',  ( -2.121784821874996840, 12.22812500061451857, 33.67503911421598417 ) ) ;
#33986 =( BOUNDED_CURVE ( )  B_SPLINE_CURVE ( 2, ( #27702, #67954, #11796, #39513, #34313, #56846, #28779, #33954, #62760 ),
 .UNSPECIFIED., .F., .T. ) 
 B_SPLINE_CURVE_WITH_KNOTS ( ( 3, 2, 2, 2, 3 ),
 ( 0.1195652173913043514, 0.1231884057971014551, 0.1304347826086956486, 0.1376811594202898559, 0.1413043478260869734 ),
 .UNSPECIFIED. ) 
 CURVE ( )  GEOMETRIC_REPRESENTATION_ITEM ( )  RATIONAL_B_SPLINE_CURVE ( ( 0.9330127018922194093, 0.9330127018922194093, 1.000000000000000000, 0.8660254037844387076, 1.000000000000000000, 0.8660254037844387076, 1.000000000000000000, 0.9330127018922190762, 0.9330127018922194093 ) ) 
 REPRESENTATION_ITEM ( '' )  );
#33987 = FACE_OUTER_BOUND ( 'NONE', #70326, .T. ) ;
#33988 = CARTESIAN_POINT ( 'NONE',  ( 20.66250000122903074, 0.000000000000000000, 4.999999999999998224 ) ) ;
#33989 = CARTESIAN_POINT ( 'NONE',  ( 3.756430356250000102, 12.75312499938548427, 30.00000000000000000 ) ) ;
#33990 = CARTESIAN_POINT ( 'NONE',  ( 28.24687500061451573, -3.027376345333610441, -5.243569643749999898 ) ) ;
#33991 = VERTEX_POINT ( 'NONE', #47415 ) ;
#33992 = CARTESIAN_POINT ( 'NONE',  ( 21.59062500061451928, 6.054752690667223547, 3.707466751127219781E-16 ) ) ;
#33993 = CARTESIAN_POINT ( 'NONE',  ( 22.84687500061451715, -3.027376345333610441, -5.243569643749999898 ) ) ;
#33994 = CARTESIAN_POINT ( 'NONE',  ( 7.762500000000001954, 2.886751345948129099, -4.999999999999998224 ) ) ;
#33995 = CARTESIAN_POINT ( 'NONE',  ( 9.740625000614516082, -3.027376345333610441, -5.243569643749999898 ) ) ;
#33996 = CARTESIAN_POINT ( 'NONE',  ( 24.96562500061451573, -6.054752690667223547, -1.112240025338166033E-15 ) ) ;
#33997 = CARTESIAN_POINT ( 'NONE',  ( 11.82187500061451679, 3.027376345333611329, 5.243569643749999010 ) ) ;
#33998 = CARTESIAN_POINT ( 'NONE',  ( 17.37187500061451573, -6.054752690667223547, -1.112240025338166033E-15 ) ) ;
#33999 = CARTESIAN_POINT ( 'NONE',  ( 30.00000000000000000, 0.000000000000000000, 0.000000000000000000 ) ) ;
#34000 = CARTESIAN_POINT ( 'NONE',  ( -3.000416591977282496E-16, 16.54062500061451857, 25.09994784771203058 ) ) ;
#34001 = CARTESIAN_POINT ( 'NONE',  ( 20.28750000122903074, -4.330127018922194537, 2.499999999999995559 ) ) ;
#34002 = CARTESIAN_POINT ( 'NONE',  ( 13.73437500061451821, -4.119189519843968306, 2.378215178124996054 ) ) ;
#34003 = CARTESIAN_POINT ( 'NONE',  ( 11.80312500061451608, 0.000000000000000000, 5.243569643749999010 ) ) ;
#34004 = CARTESIAN_POINT ( 'NONE',  ( 5.146875000614517859, -3.027376345333614438, 5.243569643749998122 ) ) ;
#34005 = CARTESIAN_POINT ( 'NONE',  ( 5.596875000614516260, -3.027376345333614438, 5.243569643749998122 ) ) ;
#34006 = ORIENTED_EDGE ( 'NONE', *, *, #11564, .F. ) ;
#34007 = CARTESIAN_POINT ( 'NONE',  ( 26.03437500061451715, 6.421520780324663323E-16, -5.243569643749999010 ) ) ;
#34008 = CARTESIAN_POINT ( 'NONE',  ( 16.90312500061451573, -4.541064518000417216, -2.621784821875001281 ) ) ;
#34009 = CARTESIAN_POINT ( 'NONE',  ( 27.78750000122903074, 4.330127018922191873, 2.499999999999999556 ) ) ;
#34010 = CARTESIAN_POINT ( 'NONE',  ( 27.21562500061451928, -6.054752690667223547, -1.112240025338166033E-15 ) ) ;
#34011 = CARTESIAN_POINT ( 'NONE',  ( 20.82187500061451857, 3.027376345333611329, 5.243569643749999010 ) ) ;
#34012 = CARTESIAN_POINT ( 'NONE',  ( 17.57812500061451644, 4.541064518000418104, 2.621784821874999949 ) ) ;
#34013 = CARTESIAN_POINT ( 'NONE',  ( -3.000416591977282496E-16, 18.39687500061451786, 25.09994784771203058 ) ) ;
#34014 = CARTESIAN_POINT ( 'NONE',  ( 23.61562500061451431, -6.054752690667223547, -1.112240025338166033E-15 ) ) ;
#34015 = CARTESIAN_POINT ( 'NONE',  ( 5.137500001229033941, 6.123233995736764310E-16, -4.999999999999998224 ) ) ;
#34016 = ORIENTED_EDGE ( 'NONE', *, *, #48422, .T. ) ;
#34017 = CARTESIAN_POINT ( 'NONE',  ( 28.38749999999999929, -2.886751345948125991, -5.000000000000000000 ) ) ;
#34018 = CARTESIAN_POINT ( 'NONE',  ( 8.484601909799253346E-16, 13.36250000000000071, -25.38119784648299770 ) ) ;
#34019 = CARTESIAN_POINT ( 'NONE',  ( -3.756430356249999214, 17.44062499938548427, 27.83122392262697531 ) ) ;
#34020 = CARTESIAN_POINT ( 'NONE',  ( 29.72812500061451502, 4.541064518000418104, 2.621784821874999949 ) ) ;
#34021 = CARTESIAN_POINT ( 'NONE',  ( 9.478125000614515017, 4.541064518000418104, 2.621784821874999949 ) ) ;
#34022 = CARTESIAN_POINT ( 'NONE',  ( 21.86250000122903003, 4.330127018922192761, -2.499999999999997780 ) ) ;
#34023 = CARTESIAN_POINT ( 'NONE',  ( 13.32187500061451502, -6.054752690667223547, -1.112240025338166033E-15 ) ) ;
#34024 = CARTESIAN_POINT ( 'NONE',  ( 2.934375000614518392, -4.541064518000419881, 2.621784821874995952 ) ) ;
#34025 = CARTESIAN_POINT ( 'NONE',  ( 26.77499999999999858, 4.330127018922191873, 2.499999999999999556 ) ) ;
#34026 = CARTESIAN_POINT ( 'NONE',  ( 14.73750000122903359, 4.330127018922191873, 2.499999999999999556 ) ) ;
#34027 = CARTESIAN_POINT ( 'NONE',  ( 14.09062500061451750, -3.027376345333614438, 5.243569643749998122 ) ) ;
#34028 = EDGE_LOOP ( 'NONE', ( #8358, #41983, #30572, #57847 ) ) ;
#34029 = CARTESIAN_POINT ( 'NONE',  ( 9.665625000614515017, -6.054752690667223547, -1.112240025338166033E-15 ) ) ;
#34030 = CARTESIAN_POINT ( 'NONE',  ( 5.503125000614516260, 0.000000000000000000, 5.243569643749999010 ) ) ;
#34031 = CARTESIAN_POINT ( 'NONE',  ( 17.82187500061451502, -5.492252693125287522, -1.008910452111647106E-15 ) ) ;
#34032 = CYLINDRICAL_SURFACE ( 'NONE', #20829, 4.999999999999998224 ) ;
#34033 = CARTESIAN_POINT ( 'NONE',  ( 15.29999999999999893, -4.330127018922190985, -2.500000000000001332 ) ) ;
#34034 = CARTESIAN_POINT ( 'NONE',  ( 16.13437500061451502, 6.421520780324663323E-16, -5.243569643749999010 ) ) ;
#34035 = CARTESIAN_POINT ( 'NONE',  ( 11.73750000122903181, -4.330127018922194537, 2.499999999999995559 ) ) ;
#34036 = CARTESIAN_POINT ( 'NONE',  ( 18.72187500061451360, -6.054752690667223547, -1.112240025338166033E-15 ) ) ;
#34037 = CARTESIAN_POINT ( 'NONE',  ( 20.47500000000000142, 4.330127018922191873, 2.499999999999999556 ) ) ;
#34038 = CARTESIAN_POINT ( 'NONE',  ( 20.85937500061451644, 0.000000000000000000, 5.243569643749999010 ) ) ;
#34039 = CARTESIAN_POINT ( 'NONE',  ( -4.243569643749999898, 13.50312500061451715, -30.00000000000000000 ) ) ;
#34040 = CARTESIAN_POINT ( 'NONE',  ( 21.00000000122903288, 5.773502691896255534, 3.535250795749688401E-16 ) ) ;
#34041 = CARTESIAN_POINT ( 'NONE',  ( 24.83437500061451431, -2.746126346562646425, 4.756430356249996549 ) ) ;
#34042 = CARTESIAN_POINT ( 'NONE',  ( 12.67499999999999893, 6.123233995736764310E-16, -4.999999999999998224 ) ) ;
#34043 = CARTESIAN_POINT ( 'NONE',  ( 26.42812500061451431, 6.421520780324663323E-16, -5.243569643749999010 ) ) ;
#34044 = CARTESIAN_POINT ( 'NONE',  ( 5.250000001229035540, 5.773502691896255534, 3.535250795749688401E-16 ) ) ;
#34045 = CARTESIAN_POINT ( 'NONE',  ( 29.03437500061451715, -4.541064518000419881, 2.621784821874995952 ) ) ;
#34046 = CARTESIAN_POINT ( 'NONE',  ( 24.56250000000000000, 2.886751345948126879, 4.999999999999999112 ) ) ;
#34047 = CARTESIAN_POINT ( 'NONE',  ( 9.178125000614517859, -4.541064518000419881, 2.621784821874995952 ) ) ;
#34048 = CARTESIAN_POINT ( 'NONE',  ( 24.27187500061451431, 4.119189519843966529, 2.378215178124999607 ) ) ;
#34049 = CARTESIAN_POINT ( 'NONE',  ( 18.98437500061451644, 4.541064518000418104, 2.621784821874999949 ) ) ;
#34050 = CARTESIAN_POINT ( 'NONE',  ( 11.82187500061451502, -4.119189519843968306, 2.378215178124996054 ) ) ;
#34051 = CARTESIAN_POINT ( 'NONE',  ( 5.390625000614518214, 6.054752690667223547, 3.707466751127219781E-16 ) ) ;
#34052 = CARTESIAN_POINT ( 'NONE',  ( 11.74687500061451573, 6.054752690667223547, 3.707466751127219781E-16 ) ) ;
#34053 = EDGE_LOOP ( 'NONE', ( #61234, #45254, #52697, #61245 ) ) ;
#34054 = CARTESIAN_POINT ( 'NONE',  ( 22.62187500061451573, 3.027376345333611329, 5.243569643749999010 ) ) ;
#34055 = CARTESIAN_POINT ( 'NONE',  ( 25.94999999999999929, 0.000000000000000000, 4.999999999999998224 ) ) ;
#34056 = CARTESIAN_POINT ( 'NONE',  ( 28.80000000000000071, -4.330127018922190985, -2.500000000000001332 ) ) ;
#34057 = CARTESIAN_POINT ( 'NONE',  ( 28.65937500061451715, -4.541064518000417216, -2.621784821875001281 ) ) ;
#34058 = CARTESIAN_POINT ( 'NONE',  ( 13.98750000122903359, -4.330127018922194537, 2.499999999999995559 ) ) ;
#34059 = CARTESIAN_POINT ( 'NONE',  ( 3.776121927792477351, -3.277331717486649421, 4.093179622544351304 ) ) ;
#34060 = EDGE_LOOP ( 'NONE', ( #6493, #6678, #26060, #22912 ) ) ;
#34061 = CARTESIAN_POINT ( 'NONE',  ( 13.38750000000000107, -2.886751345948129988, 4.999999999999997335 ) ) ;
#34062 = CARTESIAN_POINT ( 'NONE',  ( 23.80312500061451786, 4.541064518000418104, -2.621784821874998173 ) ) ;
#34063 = CARTESIAN_POINT ( 'NONE',  ( 14.24999999999999822, 0.000000000000000000, 4.999999999999998224 ) ) ;
#34064 = CARTESIAN_POINT ( 'NONE',  ( 9.487500001229033586, -4.330127018922194537, 2.499999999999995559 ) ) ;
#34065 = CARTESIAN_POINT ( 'NONE',  ( 7.940625000614518036, -3.027376345333610441, -5.243569643749999898 ) ) ;
#34066 = EDGE_CURVE ( 'NONE', #17484, #71135, #58115, .T. ) ;
#34067 = CARTESIAN_POINT ( 'NONE',  ( 8.175000000000002487, 6.123233995736764310E-16, -4.999999999999998224 ) ) ;
#34068 = CARTESIAN_POINT ( 'NONE',  ( 27.29999999999999716, 0.000000000000000000, 4.999999999999998224 ) ) ;
#34069 = CARTESIAN_POINT ( 'NONE',  ( 2.121784821875001281, 13.70937500061451786, -26.32496088578401938 ) ) ;
#34070 = CARTESIAN_POINT ( 'NONE',  ( 28.05000000122903359, -2.886751345948125991, -5.000000000000000000 ) ) ;
#34071 = CARTESIAN_POINT ( 'NONE',  ( 3.756430356250000546, 18.07812499938548711, 27.83122392262697886 ) ) ;
#34072 = CARTESIAN_POINT ( 'NONE',  ( 7.312500000000000000, 2.886751345948129099, -4.999999999999998224 ) ) ;
#34073 = DIRECTION ( 'NONE',  ( 0.000000000000000000, 0.000000000000000000, -1.000000000000000000 ) ) ;
#34074 = EDGE_LOOP ( 'NONE', ( #65587, #37518, #37507, #52639 ) ) ;
#34075 = CARTESIAN_POINT ( 'NONE',  ( 20.95312500061451999, -4.541064518000417216, -2.621784821875001281 ) ) ;
#34076 = CARTESIAN_POINT ( 'NONE',  ( 14.43750000122903288, -4.330127018922194537, 2.499999999999995559 ) ) ;
#34077 = CARTESIAN_POINT ( 'NONE',  ( 0.000000000000000000, 0.000000000000000000, 50.00000000000000000 ) ) ;
#34078 = DIRECTION ( 'NONE',  ( -0.000000000000000000, -1.000000000000000000, -0.000000000000000000 ) ) ;
#34079 = CARTESIAN_POINT ( 'NONE',  ( 20.10937500061451289, -4.541064518000417216, -2.621784821875001281 ) ) ;
#34080 = CARTESIAN_POINT ( 'NONE',  ( 17.54062500061451502, 6.054752690667223547, 3.707466751127219781E-16 ) ) ;
#34081 = CARTESIAN_POINT ( 'NONE',  ( 9.001249775931846008E-16, 12.71562500061459211, -25.09994784771203058 ) ) ;
#34082 = CARTESIAN_POINT ( 'NONE',  ( 6.478125000614516793, -4.541064518000419881, 2.621784821874995952 ) ) ;
#34083 = CARTESIAN_POINT ( 'NONE',  ( 27.97500000122903074, -5.773502691896255534, -1.060575238724906372E-15 ) ) ;
#34084 = CARTESIAN_POINT ( 'NONE',  ( 20.85937500061451644, 0.000000000000000000, 4.756430356249998326 ) ) ;
#34085 = CARTESIAN_POINT ( 'NONE',  ( 20.27812500061451573, 4.541064518000418104, 2.621784821874999949 ) ) ;
#34086 = CARTESIAN_POINT ( 'NONE',  ( 2.000000000000001332, 11.26250000122903394, -26.53589838486224650 ) ) ;
#34087 = CARTESIAN_POINT ( 'NONE',  ( 4.275000001229035895, 2.886751345948129099, -4.999999999999998224 ) ) ;
#34088 = CARTESIAN_POINT ( 'NONE',  ( 12.75937500061451857, 0.000000000000000000, 5.243569643749999010 ) ) ;
#34089 = CARTESIAN_POINT ( 'NONE',  ( 11.25937500061451679, 4.541064518000418104, -2.621784821874998173 ) ) ;
#34090 = CARTESIAN_POINT ( 'NONE',  ( 20.85937500061451644, 0.000000000000000000, 5.243569643749999010 ) ) ;
#34091 = EDGE_LOOP ( 'NONE', ( #66246, #62147, #7756, #53 ) ) ;
#34092 = CARTESIAN_POINT ( 'NONE',  ( 3.815625000614518036, -6.054752690667223547, -1.112240025338166033E-15 ) ) ;
#34093 = CARTESIAN_POINT ( 'NONE',  ( 24.85312500061451502, 0.000000000000000000, 5.243569643749999010 ) ) ;
#34094 = CARTESIAN_POINT ( 'NONE',  ( 19.99687500061451573, -3.027376345333614438, 5.243569643749998122 ) ) ;
#34095 = CARTESIAN_POINT ( 'NONE',  ( 23.87812500061451715, 4.541064518000418104, 2.621784821874999949 ) ) ;
#34096 = CARTESIAN_POINT ( 'NONE',  ( 19.76250000122903216, 0.000000000000000000, 4.999999999999998224 ) ) ;
#34097 = CARTESIAN_POINT ( 'NONE',  ( 1.999999999999998668, 16.69999999999999929, 26.53589838486224650 ) ) ;
#34098 = CARTESIAN_POINT ( 'NONE',  ( 3.759375000614517681, 0.000000000000000000, 5.243569643749999010 ) ) ;
#34099 = CONTEXT_DEPENDENT_SHAPE_REPRESENTATION ( #20035, #3073 ) ;
#34100 = CARTESIAN_POINT ( 'NONE',  ( 12.93750000122903465, 4.330127018922191873, 2.499999999999999556 ) ) ;
#34101 = CARTESIAN_POINT ( 'NONE',  ( 6.337500001229033231, -4.330127018922194537, 2.499999999999995559 ) ) ;
#34102 = CARTESIAN_POINT ( 'NONE',  ( 3.999999999999999112, 19.32500000000000284, -30.00000000000000000 ) ) ;
#34103 = CARTESIAN_POINT ( 'NONE',  ( 26.77500000122903145, 2.886751345948129099, -4.999999999999998224 ) ) ;
#34104 = CARTESIAN_POINT ( 'NONE',  ( -1.999999999999999112, 17.54374999877096641, 26.53589838486224650 ) ) ;
#34105 = CARTESIAN_POINT ( 'NONE',  ( 15.80625000122903145, -4.330127018922190985, -2.500000000000001332 ) ) ;
#34106 = CARTESIAN_POINT ( 'NONE',  ( 10.73437500061451644, 6.421520780324663323E-16, -5.243569643749999010 ) ) ;
#34107 = DIRECTION ( 'NONE',  ( 0.000000000000000000, 0.000000000000000000, 1.000000000000000000 ) ) ;
#34108 = CARTESIAN_POINT ( 'NONE',  ( 17.05312500061451786, 4.541064518000418104, -2.621784821874998173 ) ) ;
#34109 = CARTESIAN_POINT ( 'NONE',  ( 13.80937500061451750, -4.541064518000417216, -2.621784821875001281 ) ) ;
#34110 = CARTESIAN_POINT ( 'NONE',  ( 4.078125000614517326, 4.541064518000418104, 2.621784821874999949 ) ) ;
#34111 = CARTESIAN_POINT ( 'NONE',  ( 22.73437500061451644, -4.541064518000419881, 2.621784821874995952 ) ) ;
#34112 = CARTESIAN_POINT ( 'NONE',  ( 8.896875000614517859, -3.027376345333610441, -5.243569643749999898 ) ) ;
#34113 = CARTESIAN_POINT ( 'NONE',  ( 5.878125000614517148, 4.541064518000418104, 2.621784821874999949 ) ) ;
#34114 = DIRECTION ( 'NONE',  ( -1.000000000000000000, -0.000000000000000000, -0.000000000000000000 ) ) ;
#34115 = CARTESIAN_POINT ( 'NONE',  ( 6.112500001229034474, 4.330127018922192761, -2.499999999999997780 ) ) ;
#34116 = CARTESIAN_POINT ( 'NONE',  ( 19.71562500061451928, 3.027376345333613106, -5.243569643749998122 ) ) ;
#34117 = CARTESIAN_POINT ( 'NONE',  ( 6.900000001229035007, -2.886751345948125991, -5.000000000000000000 ) ) ;
#34118 = CARTESIAN_POINT ( 'NONE',  ( 17.50312500061451715, 4.541064518000418104, -2.621784821874998173 ) ) ;
#34119 = CARTESIAN_POINT ( 'NONE',  ( 13.11562500061451786, 3.027376345333611329, 5.243569643749999010 ) ) ;
#34120 = CARTESIAN_POINT ( 'NONE',  ( 26.03437500061451715, 5.824947211148865298E-16, -4.756430356249998326 ) ) ;
#34121 = CARTESIAN_POINT ( 'NONE',  ( 13.68750000000000178, 5.773502691896255534, 3.535250795749688894E-16 ) ) ;
#34122 = CARTESIAN_POINT ( 'NONE',  ( 8.587500001229035007, -4.330127018922194537, 2.499999999999995559 ) ) ;
#34123 = CARTESIAN_POINT ( 'NONE',  ( 5.053125000614517859, 0.000000000000000000, 5.243569643749999010 ) ) ;
#34124 = EDGE_CURVE ( 'NONE', #48852, #53469, #5884, .T. ) ;
#34125 = CARTESIAN_POINT ( 'NONE',  ( 19.05000000122903359, -2.886751345948125991, -5.000000000000000000 ) ) ;
#34126 = CARTESIAN_POINT ( 'NONE',  ( 26.47499999999999787, -4.330127018922194537, 2.499999999999995559 ) ) ;
#34127 = CARTESIAN_POINT ( 'NONE',  ( -4.243569643749999898, 11.30937500061451928, -30.00000000000000000 ) ) ;
#34128 = CARTESIAN_POINT ( 'NONE',  ( 9.937500000000001776, -2.886751345948126435, -5.000000000000000000 ) ) ;
#34129 = CARTESIAN_POINT ( 'NONE',  ( 3.450000001229036162, 5.773502691896255534, 3.535250795749688894E-16 ) ) ;
#34130 = CARTESIAN_POINT ( 'NONE',  ( 28.53750000122903074, 6.123233995736764310E-16, -4.999999999999998224 ) ) ;
#34131 = CARTESIAN_POINT ( 'NONE',  ( 20.03437500061451715, -4.541064518000419881, 2.621784821874995952 ) ) ;
#34132 = CARTESIAN_POINT ( 'NONE',  ( 23.08125000122903359, 6.123233995736764310E-16, -4.999999999999998224 ) ) ;
#34133 = CARTESIAN_POINT ( 'NONE',  ( 15.81562500061451537, 3.027376345333611329, 5.243569643749999010 ) ) ;
#34134 = CARTESIAN_POINT ( 'NONE',  ( 11.83125000122903181, 6.123233995736764310E-16, -4.999999999999998224 ) ) ;
#34135 = CARTESIAN_POINT ( 'NONE',  ( 10.91250000000000142, 2.886751345948062486, -5.000000000000113687 ) ) ;
#34136 = CARTESIAN_POINT ( 'NONE',  ( 25.17187500061451644, 3.027376345333613106, -5.243569643749998122 ) ) ;
#34137 = CARTESIAN_POINT ( 'NONE',  ( 18.27187500061451431, 5.824947211148865298E-16, -4.756430356249998326 ) ) ;
#34138 = CARTESIAN_POINT ( 'NONE',  ( 12.40312500061451573, -4.541064518000417216, -2.621784821875001281 ) ) ;
#34139 = CARTESIAN_POINT ( 'NONE',  ( 9.609375000614518214, 0.000000000000000000, 5.243569643749999010 ) ) ;
#34140 = ORIENTED_EDGE ( 'NONE', *, *, #11487, .T. ) ;
#34141 = CARTESIAN_POINT ( 'NONE',  ( 29.57812500061451644, 6.421520780324663323E-16, -5.243569643749999010 ) ) ;
#34142 = CARTESIAN_POINT ( 'NONE',  ( 20.46562500061451928, -6.054752690667223547, -1.112240025338166033E-15 ) ) ;
#34143 = CARTESIAN_POINT ( 'NONE',  ( 27.97500000000000142, 6.123233995736764310E-16, -4.999999999999998224 ) ) ;
#34144 = EDGE_CURVE ( 'NONE', #69611, #30395, #2715, .T. ) ;
#34145 = CARTESIAN_POINT ( 'NONE',  ( 10.70625000122903536, 0.000000000000000000, 4.999999999999998224 ) ) ;
#34146 = CARTESIAN_POINT ( 'NONE',  ( 11.10000000000000142, 0.000000000000000000, 4.999999999999998224 ) ) ;
#34147 = CARTESIAN_POINT ( 'NONE',  ( 21.56250000122903288, 0.000000000000000000, 4.999999999999998224 ) ) ;
#34148 = CARTESIAN_POINT ( 'NONE',  ( 15.51562500061451644, -6.054752690667223547, -1.112240025338166033E-15 ) ) ;
#34149 = CARTESIAN_POINT ( 'NONE',  ( 13.99687500061451395, 0.000000000000000000, 4.756430356249998326 ) ) ;
#34150 = ORIENTED_EDGE ( 'NONE', *, *, #66954, .F. ) ;
#34151 = CARTESIAN_POINT ( 'NONE',  ( 20.28750000000000142, -2.886751345948125991, -5.000000000000000000 ) ) ;
#34152 = CARTESIAN_POINT ( 'NONE',  ( 23.58749999999999858, 5.773502691896255534, 3.535250795749688894E-16 ) ) ;
#34153 = CARTESIAN_POINT ( 'NONE',  ( 21.08437500061451786, 6.421520780324663323E-16, -5.243569643749999010 ) ) ;
#34154 = CARTESIAN_POINT ( 'NONE',  ( 26.31562500061451715, -6.054752690667223547, -1.112240025338166033E-15 ) ) ;
#34155 = VERTEX_POINT ( 'NONE', #31145 ) ;
#34156 = DIRECTION ( 'NONE',  ( -1.000000000000000000, -0.000000000000000000, -0.000000000000000000 ) ) ;
#34157 = CARTESIAN_POINT ( 'NONE',  ( 7.603125000614517681, 4.541064518000418104, -2.621784821874998173 ) ) ;
#34158 = CARTESIAN_POINT ( 'NONE',  ( 3.275654489317120444, 3.777613493092820462, 3.573368934894253002 ) ) ;
#34159 = CARTESIAN_POINT ( 'NONE',  ( 14.32500000000000107, -4.330127018922194537, 2.499999999999995559 ) ) ;
#34160 = CARTESIAN_POINT ( 'NONE',  ( 4.243569643749999010, 18.26562500061451644, 27.54997392385601174 ) ) ;
#34161 = CARTESIAN_POINT ( 'NONE',  ( 3.946875000614517681, -3.027376345333610441, -5.243569643749999898 ) ) ;
#34162 = CARTESIAN_POINT ( 'NONE',  ( 26.40937500061451715, -4.541064518000417216, -2.621784821875001281 ) ) ;
#34163 = ORIENTED_EDGE ( 'NONE', *, *, #36053, .F. ) ;
#34164 = CARTESIAN_POINT ( 'NONE',  ( 24.10312500061451502, -4.541064518000417216, -2.621784821875001281 ) ) ;
#34165 = CARTESIAN_POINT ( 'NONE',  ( 24.23437500061451644, 6.421520780324663323E-16, -5.243569643749999010 ) ) ;
#34166 = CARTESIAN_POINT ( 'NONE',  ( 2.121784821875001281, 18.60312500061459673, -26.32496088578401938 ) ) ;
#34167 = CARTESIAN_POINT ( 'NONE',  ( 12.07499999999999929, -4.330127018922194537, 2.499999999999995559 ) ) ;
#34168 = CARTESIAN_POINT ( 'NONE',  ( 8.128125000614515372, 4.541064518000418104, 2.621784821874999949 ) ) ;
#34169 = CARTESIAN_POINT ( 'NONE',  ( 28.65937500061451715, -4.119189519843965641, -2.378215178125001383 ) ) ;
#34170 = CARTESIAN_POINT ( 'NONE',  ( 29.09062500061451573, -3.027376345333610441, -5.243569643749999898 ) ) ;
#34171 = CARTESIAN_POINT ( 'NONE',  ( 26.42812500061451431, 6.421520780324663323E-16, -5.243569643749999010 ) ) ;
#34172 = DIRECTION ( 'NONE',  ( 0.000000000000000000, 0.000000000000000000, -1.000000000000000000 ) ) ;
#34173 = CARTESIAN_POINT ( 'NONE',  ( 13.99687500061451928, 5.492252693125287522, 3.363034840372157021E-16 ) ) ;
#34174 = CARTESIAN_POINT ( 'NONE',  ( 20.59687500061451360, -3.027376345333610441, -5.243569643749999898 ) ) ;
#34175 = CARTESIAN_POINT ( 'NONE',  ( 4.243569643749999898, 15.13437500061451679, 30.00000000000000000 ) ) ;
#34176 = CARTESIAN_POINT ( 'NONE',  ( 19.77187500061451786, 3.027376345333613106, -5.243569643749998122 ) ) ;
#34178 = EDGE_CURVE ( 'NONE', #54204, #38333, #53686, .T. ) ;
#34177 = CARTESIAN_POINT ( 'NONE',  ( 26.52187500061451431, 3.027376345333613106, -5.243569643749998122 ) ) ;
#34179 = CARTESIAN_POINT ( 'NONE',  ( -3.000416591977282496E-16, 16.59687500061452070, 25.09994784771203058 ) ) ;
#34180 = CARTESIAN_POINT ( 'NONE',  ( 10.60312500061451679, -4.541064518000417216, -2.621784821875001281 ) ) ;
#34181 = CARTESIAN_POINT ( 'NONE',  ( 8.137500000000002842, -2.886751345948126435, -5.000000000000000000 ) ) ;
#34182 = CARTESIAN_POINT ( 'NONE',  ( 4.584375000614516971, 4.541064518000418104, 2.621784821874999949 ) ) ;
#34183 = LINE ( 'NONE', #955, #56065 ) ;
#34184 = CARTESIAN_POINT ( 'NONE',  ( 8.765625000614518214, -6.054752690667223547, -1.112240025338166033E-15 ) ) ;
#34185 = CARTESIAN_POINT ( 'NONE',  ( 11.03437500061451715, -4.541064518000419881, 2.621784821874995952 ) ) ;
#34186 = SURFACE_SIDE_STYLE ('',( #68549 ) ) ;
#34187 = CARTESIAN_POINT ( 'NONE',  ( 19.65000000122902790, 5.773502691896255534, 3.535250795749688894E-16 ) ) ;
#34188 = CARTESIAN_POINT ( 'NONE',  ( 6.609375000614519102, -4.541064518000417216, -2.621784821875001281 ) ) ;
#34189 = CARTESIAN_POINT ( 'NONE',  ( 10.22812500061451679, 6.421520780324663323E-16, -5.243569643749999010 ) ) ;
#34190 = CARTESIAN_POINT ( 'NONE',  ( 5.015625000614518214, 3.027376345333611329, 5.243569643749999010 ) ) ;
#34191 = CARTESIAN_POINT ( 'NONE',  ( 24.43125000122903145, 6.123233995736764310E-16, -4.999999999999998224 ) ) ;
#34192 = CARTESIAN_POINT ( 'NONE',  ( 19.84687500061451360, 6.054752690667223547, 3.707466751127219781E-16 ) ) ;
#34193 = CARTESIAN_POINT ( 'NONE',  ( 9.000000001229032875, -2.886751345948063374, 5.000000000000112799 ) ) ;
#34194 = ORIENTED_EDGE ( 'NONE', *, *, #12308, .F. ) ;
#34195 = CARTESIAN_POINT ( 'NONE',  ( 25.37812500061451715, -4.541064518000419881, 2.621784821874995952 ) ) ;
#34196 = CARTESIAN_POINT ( 'NONE',  ( 13.07812500061451821, 4.541064518000418104, 2.621784821874999949 ) ) ;
#34197 = CARTESIAN_POINT ( 'NONE',  ( 29.55937500061451573, -4.541064518000417216, -2.621784821875001281 ) ) ;
#34198 = CARTESIAN_POINT ( 'NONE',  ( 12.36562500061451608, -6.054752690667223547, -1.112240025338166033E-15 ) ) ;
#34199 = CARTESIAN_POINT ( 'NONE',  ( 4.243569643749999010, 10.22187500061451892, -32.45002607614398471 ) ) ;
#34200 = CARTESIAN_POINT ( 'NONE',  ( 13.53750000122903430, -4.330127018922194537, 2.499999999999995559 ) ) ;
#34201 =( BOUNDED_CURVE ( )  B_SPLINE_CURVE ( 2, ( #39442, #49434, #15799, #44986, #61963, #21707, #61240 ),
 .UNSPECIFIED., .F., .F. ) 
 B_SPLINE_CURVE_WITH_KNOTS ( ( 3, 2, 2, 3 ),
 ( 0.2083333333333332871, 0.2111111111111110827, 0.2138888888888889062, 0.2166666666666667296 ),
 .UNSPECIFIED. ) 
 CURVE ( )  GEOMETRIC_REPRESENTATION_ITEM ( )  RATIONAL_B_SPLINE_CURVE ( ( 1.000000000000002665, 0.8660254037844360431, 1.000000000000000000, 0.8660254037844387076, 1.000000000000000000, 0.8660254037844360431, 1.000000000000002665 ) ) 
 REPRESENTATION_ITEM ( '' )  );
#34202 = CARTESIAN_POINT ( 'NONE',  ( 27.36562500061451786, 3.027376345333613106, -5.243569643749998122 ) ) ;
#34203 = CARTESIAN_POINT ( 'NONE',  ( 4.243569643749999010, 12.41562500061451857, -32.45002607614398471 ) ) ;
#34204 = CARTESIAN_POINT ( 'NONE',  ( 14.92500000122903181, -5.773502691896255534, -1.060575238724906372E-15 ) ) ;
#34205 = CARTESIAN_POINT ( 'NONE',  ( 14.28750000000000142, -2.886751345948129988, 4.999999999999997335 ) ) ;
#34206 = CARTESIAN_POINT ( 'NONE',  ( 20.16562500061451146, 3.027376345333613106, -5.243569643749998122 ) ) ;
#34207 = CARTESIAN_POINT ( 'NONE',  ( 7.209375000614519635, 4.541064518000418104, -2.621784821874998173 ) ) ;
#34208 = CARTESIAN_POINT ( 'NONE',  ( 7.950000001229033053, 5.773502691896255534, 3.535250795749688894E-16 ) ) ;
#34209 = CARTESIAN_POINT ( 'NONE',  ( 17.13750000122903216, -4.330127018922194537, 2.499999999999995559 ) ) ;
#34210 = CARTESIAN_POINT ( 'NONE',  ( 13.37812500061451715, 6.421520780324663323E-16, -5.243569643749999010 ) ) ;
#34211 = CARTESIAN_POINT ( 'NONE',  ( 14.87812500061451537, 4.541064518000418104, 2.621784821874999949 ) ) ;
#34212 = CARTESIAN_POINT ( 'NONE',  ( 26.92500000122903359, 2.886751345948126879, 4.999999999999999112 ) ) ;
#34213 = CARTESIAN_POINT ( 'NONE',  ( 22.61250000000000071, 2.886751345948129099, -4.999999999999998224 ) ) ;
#34214 = CARTESIAN_POINT ( 'NONE',  ( 24.23437500061451644, 6.421520780324663323E-16, -5.243569643749999010 ) ) ;
#34215 = CYLINDRICAL_SURFACE ( 'NONE', #6395, 4.999999999999998224 ) ;
#34216 = CARTESIAN_POINT ( 'NONE',  ( 10.76250000122903572, 0.000000000000000000, 4.999999999999998224 ) ) ;
#34217 = CARTESIAN_POINT ( 'NONE',  ( 28.58437500061451786, -4.541064518000419881, 2.621784821874995952 ) ) ;
#34218 = EDGE_CURVE ( 'NONE', #7983, #24010, #69777, .T. ) ;
#34219 = CARTESIAN_POINT ( 'NONE',  ( 4.096875000614518925, 6.054752690667223547, 3.707466751127219781E-16 ) ) ;
#34220 = CARTESIAN_POINT ( 'NONE',  ( 24.32812500061451289, 4.541064518000418104, 2.621784821874999949 ) ) ;
#34221 = CARTESIAN_POINT ( 'NONE',  ( 3.756430356250000102, 13.65312499938548285, 30.00000000000000000 ) ) ;
#34222 = FACE_OUTER_BOUND ( 'NONE', #56818, .T. ) ;
#34223 = CARTESIAN_POINT ( 'NONE',  ( 10.99687500061451750, -3.027376345333614438, 5.243569643749998122 ) ) ;
#34224 = CARTESIAN_POINT ( 'NONE',  ( 25.94999999999999929, 0.000000000000000000, 4.999999999999998224 ) ) ;
#34225 = CARTESIAN_POINT ( 'NONE',  ( 28.97812500061451502, -4.541064518000419881, 2.621784821874995952 ) ) ;
#34226 = CARTESIAN_POINT ( 'NONE',  ( 6.309375000614517504, 4.541064518000418104, -2.621784821874998173 ) ) ;
#34227 = FACE_OUTER_BOUND ( 'NONE', #274, .T. ) ;
#34228 = CARTESIAN_POINT ( 'NONE',  ( 26.40937500061451715, -4.541064518000417216, -2.621784821875001281 ) ) ;
#34229 = CARTESIAN_POINT ( 'NONE',  ( -3.000416591977282496E-16, 11.14062500061459637, 25.09994784771203058 ) ) ;
#34230 = CARTESIAN_POINT ( 'NONE',  ( 19.72499999999999787, -4.330127018922194537, 2.499999999999995559 ) ) ;
#34231 = ORIENTED_EDGE ( 'NONE', *, *, #51961, .T. ) ;
#34232 = CARTESIAN_POINT ( 'NONE',  ( 26.96249999999999858, -5.773502691896255534, -1.060575238724906372E-15 ) ) ;
#34233 = CARTESIAN_POINT ( 'NONE',  ( 28.35937500061451289, 4.541064518000418104, -2.621784821874998173 ) ) ;
#34234 = ORIENTED_EDGE ( 'NONE', *, *, #34124, .F. ) ;
#34235 = CARTESIAN_POINT ( 'NONE',  ( 16.49062500061451786, -3.027376345333610441, -5.243569643749999898 ) ) ;
#34236 = CARTESIAN_POINT ( 'NONE',  ( 8.315625000614515372, -6.054752690667223547, -1.112240025338166033E-15 ) ) ;
#34237 = CARTESIAN_POINT ( 'NONE',  ( 19.62187500061451573, 5.824947211148865298E-16, -4.756430356249998326 ) ) ;
#34238 = CARTESIAN_POINT ( 'NONE',  ( 5.446875000614518569, 6.054752690667223547, 3.707466751127219781E-16 ) ) ;
#34239 = CARTESIAN_POINT ( 'NONE',  ( 17.28750000122903430, 6.123233995736764310E-16, -4.999999999999998224 ) ) ;
#34240 = CARTESIAN_POINT ( 'NONE',  ( 22.05000000000000071, -4.330127018922190985, -2.500000000000001332 ) ) ;
#34241 = CARTESIAN_POINT ( 'NONE',  ( 1.510657702057710734E-15, 19.43750000000000000, -33.99999999999999289 ) ) ;
#34242 = CARTESIAN_POINT ( 'NONE',  ( 3.909375000614518481, -4.541064518000417216, -2.621784821875001281 ) ) ;
#34243 = CARTESIAN_POINT ( 'NONE',  ( 10.95937500061451964, 0.000000000000000000, 5.243569643749999010 ) ) ;
#34244 = CARTESIAN_POINT ( 'NONE',  ( 22.05937500061451573, 4.541064518000418104, -2.621784821874998173 ) ) ;
#34245 = CARTESIAN_POINT ( 'NONE',  ( 1.592000809091587073E-14, 17.18750000000000355, -34.00000000000000000 ) ) ;
#34246 = ORIENTED_EDGE ( 'NONE', *, *, #42591, .F. ) ;
#34247 = CARTESIAN_POINT ( 'NONE',  ( 4.771875000614516971, -6.054752690667223547, -1.112240025338166033E-15 ) ) ;
#34249 = ADVANCED_FACE ( 'NONE', ( #59947 ), #55517, .T. ) ;
#34248 = CARTESIAN_POINT ( 'NONE',  ( 8.146875000614516082, 6.054752690667223547, 3.707466751127219781E-16 ) ) ;
#34250 = CARTESIAN_POINT ( 'NONE',  ( 19.42499999999999716, 6.123233995736764310E-16, -4.999999999999998224 ) ) ;
#34251 = CARTESIAN_POINT ( 'NONE',  ( 16.30312500061451786, 0.000000000000000000, 5.243569643749999010 ) ) ;
#34252 = CARTESIAN_POINT ( 'NONE',  ( -2.000000000000001776, 16.40000000000000213, 33.46410161513775705 ) ) ;
#34253 = FACE_OUTER_BOUND ( 'NONE', #41128, .T. ) ;
#34254 = CARTESIAN_POINT ( 'NONE',  ( 19.02187500061451786, 2.746126346562643317, 4.756430356249998326 ) ) ;
#34255 = CARTESIAN_POINT ( 'NONE',  ( 10.60312500061451679, -4.541064518000417216, -2.621784821875001281 ) ) ;
#34256 = CARTESIAN_POINT ( 'NONE',  ( 27.12187500061451573, 3.027376345333611329, 5.243569643749999010 ) ) ;
#34257 = CARTESIAN_POINT ( 'NONE',  ( 20.21250000000000213, -5.773502691896255534, -1.060575238724906372E-15 ) ) ;
#34258 = CARTESIAN_POINT ( 'NONE',  ( 26.52187500061451431, 3.027376345333613106, -5.243569643749998122 ) ) ;
#34259 = CARTESIAN_POINT ( 'NONE',  ( 8.775000000000002132, 4.330127018922191873, 2.499999999999999556 ) ) ;
#34260 = CARTESIAN_POINT ( 'NONE',  ( -1.999999999999997113, 16.13750000122903216, 33.46410161513775705 ) ) ;
#34261 = CARTESIAN_POINT ( 'NONE',  ( 8.250000001229034652, -2.886751345948125991, -5.000000000000000000 ) ) ;
#34262 = CARTESIAN_POINT ( 'NONE',  ( 20.70937500061451786, 4.541064518000418104, -2.621784821874998173 ) ) ;
#34263 = CARTESIAN_POINT ( 'NONE',  ( 14.22187500061451537, -6.054752690667223547, -1.112240025338166033E-15 ) ) ;
#34264 = DIRECTION ( 'NONE',  ( -1.000000000000000000, -0.000000000000000000, -0.000000000000000000 ) ) ;
#34265 = ORIENTED_EDGE ( 'NONE', *, *, #61021, .F. ) ;
#34266 = CARTESIAN_POINT ( 'NONE',  ( 15.85312500061451857, 0.000000000000000000, 5.243569643749999010 ) ) ;
#34267 = CARTESIAN_POINT ( 'NONE',  ( 26.28750000122903430, 6.123233995736764310E-16, -4.999999999999998224 ) ) ;
#34268 = CARTESIAN_POINT ( 'NONE',  ( 14.14687500061451786, -3.027376345333614438, 5.243569643749998122 ) ) ;
#34269 = CARTESIAN_POINT ( 'NONE',  ( 4.096875000614518925, 6.054752690667223547, 3.707466751127219781E-16 ) ) ;
#34270 = CARTESIAN_POINT ( 'NONE',  ( 16.71562500061451573, 3.027376345333611329, 5.243569643749999010 ) ) ;
#34271 = LINE ( 'NONE', #18725, #25611 ) ;
#34272 = ADVANCED_FACE ( 'NONE', ( #21153 ), #20418, .T. ) ;
#34273 = CARTESIAN_POINT ( 'NONE',  ( 25.24687500061451573, 6.054752690667223547, 3.707466751127219781E-16 ) ) ;
#34274 = CARTESIAN_POINT ( 'NONE',  ( -0.7368881354385758975, 9.803648613939515144, 25.82089971438751519 ) ) ;
#34275 = CARTESIAN_POINT ( 'NONE',  ( 15.94687500061451502, -3.027376345333614438, 5.243569643749998122 ) ) ;
#34276 = CARTESIAN_POINT ( 'NONE',  ( 11.21250000122903501, 0.000000000000000000, 4.999999999999998224 ) ) ;
#34277 = CARTESIAN_POINT ( 'NONE',  ( 7.471875000614519813, -5.492252693125287522, -1.008910452111647106E-15 ) ) ;
#34278 = CARTESIAN_POINT ( 'NONE',  ( -4.243569643749999898, 15.77187500061451608, -32.45002607614398471 ) ) ;
#34279 = CARTESIAN_POINT ( 'NONE',  ( 17.78437500061451715, -4.541064518000419881, 2.621784821874995952 ) ) ;
#34280 = CARTESIAN_POINT ( 'NONE',  ( 21.15000000122903145, -2.886751345948129988, 4.999999999999997335 ) ) ;
#34281 = CARTESIAN_POINT ( 'NONE',  ( 14.07187500061451679, 3.027376345333611329, 5.243569643749999010 ) ) ;
#34282 = CARTESIAN_POINT ( 'NONE',  ( -2.121784821874999949, 11.23437500061451821, 26.32496088578401938 ) ) ;
#34283 = CARTESIAN_POINT ( 'NONE',  ( 22.83750000122903501, 4.330127018922191873, 2.499999999999999556 ) ) ;
#34284 = CARTESIAN_POINT ( 'NONE',  ( 15.06562500061451537, -6.054752690667223547, -1.112240025338166033E-15 ) ) ;
#34285 = CARTESIAN_POINT ( 'NONE',  ( 0.000000000000000000, 20.00000000000000000, -30.00000000000000000 ) ) ;
#34286 = ORIENTED_EDGE ( 'NONE', *, *, #10471, .T. ) ;
#34287 = ORIENTED_EDGE ( 'NONE', *, *, #41535, .F. ) ;
#34288 = CARTESIAN_POINT ( 'NONE',  ( 20.13749999999999929, -2.886751345948129988, 4.999999999999997335 ) ) ;
#34289 = CARTESIAN_POINT ( 'NONE',  ( -1.071796769724487453, 17.77009619066136636, 26.00000000000000000 ) ) ;
#34290 = CARTESIAN_POINT ( 'NONE',  ( 3.440625000614518036, -3.027376345333610441, -5.243569643749999898 ) ) ;
#34291 = CARTESIAN_POINT ( 'NONE',  ( 16.12500000122903288, 2.886751345948126879, 4.999999999999999112 ) ) ;
#34292 = CARTESIAN_POINT ( 'NONE',  ( 20.87812500061451715, -4.541064518000419881, 2.621784821874995952 ) ) ;
#34293 = ADVANCED_FACE ( 'NONE', ( #26343, #10447 ), #71043, .T. ) ;
#34294 = CARTESIAN_POINT ( 'NONE',  ( 22.52812500061451573, 4.541064518000418104, 2.621784821874999949 ) ) ;
#34295 = CARTESIAN_POINT ( 'NONE',  ( 4.078125000614517326, 4.541064518000418104, 2.621784821874999949 ) ) ;
#34296 = CARTESIAN_POINT ( 'NONE',  ( 28.87499999999999645, 6.123233995736764310E-16, -4.999999999999998224 ) ) ;
#34297 = DIRECTION ( 'NONE',  ( -0.000000000000000000, -1.000000000000000000, -0.000000000000000000 ) ) ;
#34298 = CARTESIAN_POINT ( 'NONE',  ( 9.009375000614518569, 4.119189519843966529, -2.378215178124998275 ) ) ;
#34299 = CARTESIAN_POINT ( 'NONE',  ( 6.487500001229034474, 6.123233995736764310E-16, -4.999999999999998224 ) ) ;
#34300 = CARTESIAN_POINT ( 'NONE',  ( -3.999999999999999112, 12.01250000122903394, -30.00000000000000000 ) ) ;
#34301 = CARTESIAN_POINT ( 'NONE',  ( -2.121784821874996840, 17.23437500061451999, -26.32496088578401583 ) ) ;
#34302 = EDGE_CURVE ( 'NONE', #54059, #19228, #20787, .T. ) ;
#34303 = CARTESIAN_POINT ( 'NONE',  ( 6.150000001229033231, 5.773502691896255534, 3.535250795749688894E-16 ) ) ;
#34304 = CARTESIAN_POINT ( 'NONE',  ( 8.099999999999999645, -4.330127018922190985, -2.500000000000001332 ) ) ;
#34305 = CARTESIAN_POINT ( 'NONE',  ( 4.275000001229035895, 2.886751345948129099, -4.999999999999998224 ) ) ;
#34306 = CARTESIAN_POINT ( 'NONE',  ( 11.22187500061451892, 3.027376345333613106, -5.243569643749998122 ) ) ;
#34307 = CARTESIAN_POINT ( 'NONE',  ( 2.000000000000001332, 16.66250000122903430, -26.53589838486224650 ) ) ;
#34308 = CARTESIAN_POINT ( 'NONE',  ( 3.346875000614518036, -3.027376345333614438, 5.243569643749998122 ) ) ;
#34309 = CARTESIAN_POINT ( 'NONE',  ( 1.510657702057710734E-15, 19.10000000122903430, 26.00000000000000000 ) ) ;
#34310 = CARTESIAN_POINT ( 'NONE',  ( 34.99999999999999289, 2.500000000000000000, -3.500000000000000000 ) ) ;
#34311 = CARTESIAN_POINT ( 'NONE',  ( 10.99687500061451750, -3.027376345333614438, 5.243569643749998122 ) ) ;
#34312 = CARTESIAN_POINT ( 'NONE',  ( 14.03437500061451715, 4.541064518000418104, 2.621784821874999949 ) ) ;
#34313 = CARTESIAN_POINT ( 'NONE',  ( -3.999999999999999112, 18.64999999999999858, -30.00000000000000000 ) ) ;
#34314 = CARTESIAN_POINT ( 'NONE',  ( 6.825000000000001066, 6.123233995736764310E-16, -4.999999999999998224 ) ) ;
#34315 = CARTESIAN_POINT ( 'NONE',  ( 9.001249775931846008E-16, 17.66562500061459318, 34.90005215228797653 ) ) ;
#34316 = CARTESIAN_POINT ( 'NONE',  ( 22.43437500061451573, 6.421520780324663323E-16, -5.243569643749999010 ) ) ;
#34317 = VECTOR ( 'NONE', #53507, 1000.000000000000000 ) ;
#34318 = CARTESIAN_POINT ( 'NONE',  ( 45.00000000000000000, 0.000000000000000000, 4.999999999999998224 ) ) ;
#34319 = CARTESIAN_POINT ( 'NONE',  ( 26.32500000122903216, 2.886751345948129099, -4.999999999999998224 ) ) ;
#34320 = CARTESIAN_POINT ( 'NONE',  ( 17.78437500061451360, -2.746126346562642428, -4.756430356249999214 ) ) ;
#34321 = CARTESIAN_POINT ( 'NONE',  ( 23.01562500061451644, 3.027376345333611329, 5.243569643749999010 ) ) ;
#34322 = CARTESIAN_POINT ( 'NONE',  ( 16.15312500061451573, 4.541064518000418104, -2.621784821874998173 ) ) ;
#34323 = CARTESIAN_POINT ( 'NONE',  ( 25.02187500061451431, 5.824947211148865298E-16, -4.756430356249998326 ) ) ;
#34324 = CARTESIAN_POINT ( 'NONE',  ( 12.04687500061451821, -3.027376345333610441, -5.243569643749999898 ) ) ;
#34325 = CARTESIAN_POINT ( 'NONE',  ( 27.44999999999999929, -4.330127018922190985, -2.500000000000001332 ) ) ;
#34326 = CARTESIAN_POINT ( 'NONE',  ( 25.61250000122903359, 0.000000000000000000, 4.999999999999998224 ) ) ;
#34327 = CARTESIAN_POINT ( 'NONE',  ( 4.434375000614519280, 6.421520780324663323E-16, -5.243569643749999010 ) ) ;
#34328 = CARTESIAN_POINT ( 'NONE',  ( 14.70937500061451786, -4.541064518000417216, -2.621784821875001281 ) ) ;
#34329 = CARTESIAN_POINT ( 'NONE',  ( 28.32187500061451502, 3.027376345333613106, -5.243569643749998122 ) ) ;
#34330 = DIRECTION ( 'NONE',  ( -1.000000000000000000, -0.000000000000000000, -0.000000000000000000 ) ) ;
#34331 = CYLINDRICAL_SURFACE ( 'NONE', #11255, 4.999999999999998224 ) ;
#34332 = CARTESIAN_POINT ( 'NONE',  ( 21.38437500061451502, -4.541064518000419881, 2.621784821874995952 ) ) ;
#34333 = CARTESIAN_POINT ( 'NONE',  ( 14.93437500061451750, 4.541064518000418104, 2.621784821874999949 ) ) ;
#34334 = CARTESIAN_POINT ( 'NONE',  ( 3.756430356250000546, 18.64062499938548001, 27.83122392262697886 ) ) ;
#34335 = CARTESIAN_POINT ( 'NONE',  ( 26.06250000000000000, -5.773502691896255534, -1.060575238724906372E-15 ) ) ;
#34336 = CARTESIAN_POINT ( 'NONE',  ( 2.850000001229036073, -2.886751345948125991, -5.000000000000000000 ) ) ;
#34337 = CARTESIAN_POINT ( 'NONE',  ( 26.82187500061451857, -5.492252693125287522, -1.008910452111647106E-15 ) ) ;
#34338 = CARTESIAN_POINT ( 'NONE',  ( 17.01562500061451644, 3.027376345333613106, -5.243569643749998122 ) ) ;
#34339 = CARTESIAN_POINT ( 'NONE',  ( 6.112499999999999822, 2.886751345948126879, 4.999999999999999112 ) ) ;
#34340 =( BOUNDED_CURVE ( )  B_SPLINE_CURVE ( 2, ( #16831, #61903, #592, #5763, #11667, #50829, #62627, #12022, #29017 ),
 .UNSPECIFIED., .F., .F. ) 
 B_SPLINE_CURVE_WITH_KNOTS ( ( 3, 2, 2, 2, 3 ),
 ( 0.3369565217391304324, 0.3405797101449275499, 0.3478260869565217295, 0.3550724637681159646, 0.3586956521739130821 ),
 .UNSPECIFIED. ) 
 CURVE ( )  GEOMETRIC_REPRESENTATION_ITEM ( )  RATIONAL_B_SPLINE_CURVE ( ( 0.9330127018922194093, 0.9330127018922194093, 1.000000000000000000, 0.8660254037844387076, 1.000000000000000000, 0.8660254037844387076, 1.000000000000000000, 0.9330127018922188542, 0.9330127018922194093 ) ) 
 REPRESENTATION_ITEM ( '' )  );
#34341 = CARTESIAN_POINT ( 'NONE',  ( 15.56249999999999822, 2.886751345948193936, 4.999999999999883649 ) ) ;
#34342 = CARTESIAN_POINT ( 'NONE',  ( 16.68750000000000000, -2.886751345948125991, -5.000000000000000000 ) ) ;
#34343 = CARTESIAN_POINT ( 'NONE',  ( -4.243569643749999898, 12.60312500061451679, 30.00000000000000000 ) ) ;
#34344 = CARTESIAN_POINT ( 'NONE',  ( -1.243387493232115393E-14, 16.21250000000000213, 26.00000000000000000 ) ) ;
#34345 = CARTESIAN_POINT ( 'NONE',  ( 21.00000000122903288, 5.773502691896255534, 3.535250795749688894E-16 ) ) ;
#34346 = CARTESIAN_POINT ( 'NONE',  ( 27.00937500061451857, 4.541064518000418104, -2.621784821874998173 ) ) ;
#34347 = VERTEX_POINT ( 'NONE', #15248 ) ;
#34348 = CARTESIAN_POINT ( 'NONE',  ( 20.91562500061451502, -6.054752690667223547, -1.112240025338166033E-15 ) ) ;
#34349 = CARTESIAN_POINT ( 'NONE',  ( 21.23437500061451644, 4.541064518000418104, 2.621784821874999949 ) ) ;
#34350 = CARTESIAN_POINT ( 'NONE',  ( 3.712499999999999911, 2.886751345948129099, -4.999999999999998224 ) ) ;
#34351 = CARTESIAN_POINT ( 'NONE',  ( 8.615625000614517859, 3.027376345333611329, 5.243569643749999010 ) ) ;
#34352 = CARTESIAN_POINT ( 'NONE',  ( 23.31562500061451715, 3.027376345333613106, -5.243569643749998122 ) ) ;
#34353 = CARTESIAN_POINT ( 'NONE',  ( 11.89687500061451608, -3.027376345333614438, 5.243569643749998122 ) ) ;
#34354 = CARTESIAN_POINT ( 'NONE',  ( 17.85937500061451999, -4.541064518000417216, -2.621784821875001281 ) ) ;
#34356 = CARTESIAN_POINT ( 'NONE',  ( 4.243569643749999898, 17.77812500061451928, 30.00000000000000000 ) ) ;
#34355 = PRODUCT_DEFINITION_SHAPE ( 'NONE', 'NONE',  #36353 ) ;
#34357 = CARTESIAN_POINT ( 'NONE',  ( 21.37500000122902932, 2.886751345948129099, -4.999999999999998224 ) ) ;
#34358 = CARTESIAN_POINT ( 'NONE',  ( 15.79687500061451644, 5.492252693125287522, 3.363034840372157021E-16 ) ) ;
#34359 = CARTESIAN_POINT ( 'NONE',  ( 12.62812500061451537, 4.541064518000418104, 2.621784821874999949 ) ) ;
#34360 = CARTESIAN_POINT ( 'NONE',  ( 4.584375000614516971, 4.541064518000418104, 2.621784821874999949 ) ) ;
#34361 = CARTESIAN_POINT ( 'NONE',  ( 4.921875000614518214, 3.027376345333613106, -5.243569643749998122 ) ) ;
#34362 = ORIENTED_EDGE ( 'NONE', *, *, #42665, .F. ) ;
#34363 = CARTESIAN_POINT ( 'NONE',  ( 24.27187500061452141, 3.027376345333613106, -5.243569643749998122 ) ) ;
#34364 = CARTESIAN_POINT ( 'NONE',  ( 15.96562500061451573, -6.054752690667223547, -1.112240025338166033E-15 ) ) ;
#34365 = CARTESIAN_POINT ( 'NONE',  ( 26.77500000122903145, 2.886751345948129099, -4.999999999999998224 ) ) ;
#34366 = CARTESIAN_POINT ( 'NONE',  ( 27.51562500061451644, 3.027376345333611329, 5.243569643749999010 ) ) ;
#34367 = CARTESIAN_POINT ( 'NONE',  ( 21.30937500061451573, 0.000000000000000000, 5.243569643749999010 ) ) ;
#34368 = CARTESIAN_POINT ( 'NONE',  ( 16.07812500061451289, 6.421520780324663323E-16, -5.243569643749999010 ) ) ;
#34369 = CARTESIAN_POINT ( 'NONE',  ( -2.121784821874999949, 19.78437500061451715, 26.32496088578401938 ) ) ;
#34370 = CARTESIAN_POINT ( 'NONE',  ( 22.52812500061451573, 4.541064518000418104, 2.621784821874999949 ) ) ;
#34371 = CARTESIAN_POINT ( 'NONE',  ( 29.38125000122903074, 6.123233995736764310E-16, -4.999999999999998224 ) ) ;
#34372 = ORIENTED_EDGE ( 'NONE', *, *, #62833, .T. ) ;
#34373 = CARTESIAN_POINT ( 'NONE',  ( 27.97500000000000142, 6.123233995736764310E-16, -4.999999999999998224 ) ) ;
#34374 = CARTESIAN_POINT ( 'NONE',  ( 2.000000000000001332, 12.95000000000000107, -26.53589838486224650 ) ) ;
#34375 = CARTESIAN_POINT ( 'NONE',  ( 2.655984681222220721E-16, 18.26562499938548356, 25.66244784525396483 ) ) ;
#34376 = CARTESIAN_POINT ( 'NONE',  ( 28.41562500061451502, 3.027376345333611329, 5.243569643749999010 ) ) ;
#34377 = EDGE_CURVE ( 'NONE', #12584, #3838, #54252, .T. ) ;
#34378 = CARTESIAN_POINT ( 'NONE',  ( 11.24062500061451608, 6.054752690667223547, 3.707466751127219781E-16 ) ) ;
#34379 = CARTESIAN_POINT ( 'NONE',  ( 22.76250000122903216, 4.330127018922192761, -2.499999999999997780 ) ) ;
#34380 = CARTESIAN_POINT ( 'NONE',  ( 12.34687500061451892, -3.027376345333614438, 5.243569643749998122 ) ) ;
#34381 = CARTESIAN_POINT ( 'NONE',  ( 28.15312500061451573, -4.541064518000417216, -2.621784821875001281 ) ) ;
#34383 = CARTESIAN_POINT ( 'NONE',  ( 28.19999999999999929, 0.000000000000000000, 4.999999999999998224 ) ) ;
#34382 = COLOUR_RGB ( '',0.8941176470588234615, 0.8941176470588234615, 0.8941176470588234615 ) ;
#34384 = CARTESIAN_POINT ( 'NONE',  ( 8.484601909799253346E-16, 17.97500000122903785, -25.38119784648299770 ) ) ;
#34385 = CYLINDRICAL_SURFACE ( 'NONE', #23200, 4.999999999999998224 ) ;
#34386 = CARTESIAN_POINT ( 'NONE',  ( 11.84062500061451750, -3.027376345333614438, 5.243569643749998122 ) ) ;
#34387 = VERTEX_POINT ( 'NONE', #4188 ) ;
#34388 = CARTESIAN_POINT ( 'NONE',  ( 8.840625000614515727, -3.027376345333610441, -5.243569643749999898 ) ) ;
#34389 = CARTESIAN_POINT ( 'NONE',  ( 5.653125000614517504, -4.541064518000417216, -2.621784821875001281 ) ) ;
#34390 = CARTESIAN_POINT ( 'NONE',  ( 17.33437500061451431, -4.119189519843968306, 2.378215178124996054 ) ) ;
#34391 = DIRECTION ( 'NONE',  ( 0.000000000000000000, 0.000000000000000000, -1.000000000000000000 ) ) ;
#34392 = EDGE_CURVE ( 'NONE', #29843, #24253, #14113, .T. ) ;
#34393 =( BOUNDED_CURVE ( )  B_SPLINE_CURVE ( 2, ( #9699, #32232, #27065, #49596, #21137, #44056, #72121 ),
 .UNSPECIFIED., .F., .F. ) 
 B_SPLINE_CURVE_WITH_KNOTS ( ( 3, 2, 2, 3 ),
 ( 0.4099999999999999201, 0.4133333333333333304, 0.4166666666666667407, 0.4200000000000000955 ),
 .UNSPECIFIED. ) 
 CURVE ( )  GEOMETRIC_REPRESENTATION_ITEM ( )  RATIONAL_B_SPLINE_CURVE ( ( 1.000000000000002220, 0.8660254037844364872, 1.000000000000000000, 0.8660254037844387076, 1.000000000000000000, 0.8660254037844342667, 1.000000000000004441 ) ) 
 REPRESENTATION_ITEM ( '' )  );
#34394 = CARTESIAN_POINT ( 'NONE',  ( 16.16250000000000142, -5.773502691896255534, -1.060575238724906372E-15 ) ) ;
#34395 =( BOUNDED_CURVE ( )  B_SPLINE_CURVE ( 2, ( #28258, #45248, #11267, #55965, #29340, #6081, #40426, #68504, #34872 ),
 .UNSPECIFIED., .F., .F. ) 
 B_SPLINE_CURVE_WITH_KNOTS ( ( 3, 2, 2, 2, 3 ),
 ( 0.4021739130434782705, 0.4057971014492753881, 0.4130434782608695676, 0.4202898550724637472, 0.4239130434782608647 ),
 .UNSPECIFIED. ) 
 CURVE ( )  GEOMETRIC_REPRESENTATION_ITEM ( )  RATIONAL_B_SPLINE_CURVE ( ( 0.9330127018922194093, 0.9330127018922194093, 1.000000000000000000, 0.8660254037844387076, 1.000000000000000000, 0.8660254037844387076, 1.000000000000000000, 0.9330127018922194093, 0.9330127018922194093 ) ) 
 REPRESENTATION_ITEM ( '' )  );
#34396 = ADVANCED_FACE ( 'NONE', ( #60672 ), #48516, .T. ) ;
#34397 = CARTESIAN_POINT ( 'NONE',  ( 15.45937500061451608, 0.000000000000000000, 5.243569643749999010 ) ) ;
#34398 = CARTESIAN_POINT ( 'NONE',  ( 11.32500000122903394, -5.773502691896255534, -1.060575238724906372E-15 ) ) ;
#34399 = CARTESIAN_POINT ( 'NONE',  ( 18.49687500061452283, 6.054752690667223547, 3.707466751127219781E-16 ) ) ;
#34400 = CARTESIAN_POINT ( 'NONE',  ( 17.55000000000000071, -4.330127018922190985, -2.500000000000001332 ) ) ;
#34401 = CARTESIAN_POINT ( 'NONE',  ( 21.79687500061451644, -3.027376345333614438, 5.243569643749998122 ) ) ;
#34402 = CARTESIAN_POINT ( 'NONE',  ( 4.243569643749999010, 14.21562500061451928, -32.45002607614398471 ) ) ;
#34403 = CARTESIAN_POINT ( 'NONE',  ( 26.84999999999999787, 0.000000000000000000, 4.999999999999998224 ) ) ;
#34404 = CARTESIAN_POINT ( 'NONE',  ( 26.63437500061451502, -2.746126346562646425, 4.756430356249996549 ) ) ;
#34405 = CARTESIAN_POINT ( 'NONE',  ( 4.000000000000000000, 13.34374999877096712, 30.00000000000000000 ) ) ;
#34406 = CARTESIAN_POINT ( 'NONE',  ( 27.51562500061451644, 3.027376345333611329, 5.243569643749999010 ) ) ;
#34407 = CARTESIAN_POINT ( 'NONE',  ( -3.999999999999997335, 19.58750000000000213, -27.69059892324149530 ) ) ;
#34408 = CARTESIAN_POINT ( 'NONE',  ( 29.59687500061451715, -3.027376345333610441, -5.243569643749999898 ) ) ;
#34409 = CARTESIAN_POINT ( 'NONE',  ( 24.71250000000000213, -5.773502691896255534, -1.060575238724906372E-15 ) ) ;
#34410 =( BOUNDED_CURVE ( )  B_SPLINE_CURVE ( 2, ( #47863, #19394, #9435, #70392, #3166, #36040, #20493 ),
 .UNSPECIFIED., .F., .T. ) 
 B_SPLINE_CURVE_WITH_KNOTS ( ( 3, 2, 2, 3 ),
 ( 0.8200000000000000622, 0.8233333333333334725, 0.8266666666666667718, 0.8300000000000000711 ),
 .UNSPECIFIED. ) 
 CURVE ( )  GEOMETRIC_REPRESENTATION_ITEM ( )  RATIONAL_B_SPLINE_CURVE ( ( 0.9999999999999955591, 0.8660254037844431485, 1.000000000000000000, 0.8660254037844387076, 1.000000000000000000, 0.8660254037844342667, 1.000000000000004441 ) ) 
 REPRESENTATION_ITEM ( '' )  );
#34411 = CARTESIAN_POINT ( 'NONE',  ( 7.903125000614515727, -4.541064518000417216, -2.621784821875001281 ) ) ;
#34412 = CARTESIAN_POINT ( 'NONE',  ( 24.79687500061451644, 0.000000000000000000, 4.756430356249998326 ) ) ;
#34413 = CARTESIAN_POINT ( 'NONE',  ( 19.62187500061451573, -6.054752690667223547, -1.112240025338166033E-15 ) ) ;
#34414 = CARTESIAN_POINT ( 'NONE',  ( 11.63437500061451502, 5.492252693125287522, 3.363034840372157021E-16 ) ) ;
#34415 = CARTESIAN_POINT ( 'NONE',  ( 5.428125000614517859, 4.541064518000418104, 2.621784821874999949 ) ) ;
#34416 = CARTESIAN_POINT ( 'NONE',  ( 11.10937500061451644, -4.541064518000417216, -2.621784821875001281 ) ) ;
#34417 = ORIENTED_EDGE ( 'NONE', *, *, #44436, .T. ) ;
#34418 = CARTESIAN_POINT ( 'NONE',  ( 20.29687500061451644, 6.054752690667223547, 3.707466751127219781E-16 ) ) ;
#34419 = DIRECTION ( 'NONE',  ( -0.000000000000000000, -1.000000000000000000, -0.000000000000000000 ) ) ;
#34420 = CARTESIAN_POINT ( 'NONE',  ( 28.01249999999999574, 2.886751345948129099, -4.999999999999998224 ) ) ;
#34421 = CARTESIAN_POINT ( 'NONE',  ( 29.70937500061451431, 4.541064518000418104, -2.621784821874998173 ) ) ;
#34422 = LINE ( 'NONE', #61052, #57286 ) ;
#34423 = DIRECTION ( 'NONE',  ( 0.000000000000000000, 0.000000000000000000, 1.000000000000000000 ) ) ;
#34424 = ORIENTED_EDGE ( 'NONE', *, *, #50947, .F. ) ;
#34425 = CARTESIAN_POINT ( 'NONE',  ( 9.375000000000001776, -4.330127018922194537, 2.499999999999995559 ) ) ;
#34426 = CARTESIAN_POINT ( 'NONE',  ( 13.28437500061451537, -2.746126346562642428, -4.756430356249999214 ) ) ;
#34427 = CARTESIAN_POINT ( 'NONE',  ( 24.25312500061451715, 4.541064518000418104, -2.621784821874998173 ) ) ;
#34428 = CARTESIAN_POINT ( 'NONE',  ( 14.81250000000000000, -5.773502691896255534, -1.060575238724906372E-15 ) ) ;
#34429 = CARTESIAN_POINT ( 'NONE',  ( 11.58750000122903501, 4.330127018922191873, 2.499999999999999556 ) ) ;
#34430 = CARTESIAN_POINT ( 'NONE',  ( 9.028125000614517504, 4.541064518000418104, 2.621784821874999949 ) ) ;
#34431 = CARTESIAN_POINT ( 'NONE',  ( 7.950000000000001954, 0.000000000000000000, 4.999999999999998224 ) ) ;
#34432 = CARTESIAN_POINT ( 'NONE',  ( 16.05000000122903359, 5.773502691896255534, 3.535250795749688401E-16 ) ) ;
#34433 = AXIS2_PLACEMENT_3D ( 'NONE', #9409, #61108, #4967 ) ;
#34434 = CARTESIAN_POINT ( 'NONE',  ( 28.20000000122903216, 5.773502691896255534, 3.535250795749688894E-16 ) ) ;
#34435 = CARTESIAN_POINT ( 'NONE',  ( -7.967954043666661671E-16, 16.12812499938548427, 34.33755215474603517 ) ) ;
#34436 = CARTESIAN_POINT ( 'NONE',  ( 7.987500000000000711, -2.886751345948129988, 4.999999999999997335 ) ) ;
#34437 = CYLINDRICAL_SURFACE ( 'NONE', #16129, 4.999999999999998224 ) ;
#34438 = ORIENTED_EDGE ( 'NONE', *, *, #26979, .T. ) ;
#34439 = CARTESIAN_POINT ( 'NONE',  ( 21.44062500061452070, -3.027376345333610441, -5.243569643749999898 ) ) ;
#34440 = CARTESIAN_POINT ( 'NONE',  ( 3.332049138959096268, -3.727976942097309010, -3.471129952855481093 ) ) ;
#34441 = CARTESIAN_POINT ( 'NONE',  ( 28.54687500061451644, -3.027376345333614438, 5.243569643749998122 ) ) ;
#34442 = CARTESIAN_POINT ( 'NONE',  ( 19.20937500061451786, -4.541064518000417216, -2.621784821875001281 ) ) ;
#34443 = CARTESIAN_POINT ( 'NONE',  ( 17.39062500061451644, -3.027376345333610441, -5.243569643749999898 ) ) ;
#34444 = CARTESIAN_POINT ( 'NONE',  ( 4.243569643749999898, 11.92812500061459424, -30.00000000000000000 ) ) ;
#34445 = CARTESIAN_POINT ( 'NONE',  ( 4.940625000614515372, 6.054752690667223547, 3.707466751127219781E-16 ) ) ;
#34446 = CARTESIAN_POINT ( 'NONE',  ( 2.840625000614518392, -3.027376345333614438, 5.243569643749998122 ) ) ;
#34447 = CARTESIAN_POINT ( 'NONE',  ( 22.13437500061451502, 4.119189519843966529, 2.378215178124999607 ) ) ;
#34448 = CARTESIAN_POINT ( 'NONE',  ( 18.40312500061451573, 4.541064518000418104, -2.621784821874998173 ) ) ;
#34449 = DIRECTION ( 'NONE',  ( -1.000000000000000000, -0.000000000000000000, -0.000000000000000000 ) ) ;
#34450 = CARTESIAN_POINT ( 'NONE',  ( 3.675000001229035362, -5.773502691896255534, -1.060575238724906372E-15 ) ) ;
#34451 = CARTESIAN_POINT ( 'NONE',  ( 12.12187500061451573, 3.027376345333613106, -5.243569643749998122 ) ) ;
#34452 = CARTESIAN_POINT ( 'NONE',  ( 13.02187500061451608, 3.027376345333613106, -5.243569643749998122 ) ) ;
#34453 = CARTESIAN_POINT ( 'NONE',  ( 19.84687500061451360, 6.054752690667223547, 3.707466751127219781E-16 ) ) ;
#34454 = ORIENTED_EDGE ( 'NONE', *, *, #9967, .F. ) ;
#34455 = CARTESIAN_POINT ( 'NONE',  ( -5.376511845580211890, 8.433624770265598869, 27.30849239394979122 ) ) ;
#34456 = CARTESIAN_POINT ( 'NONE',  ( 24.51562500061451289, -6.054752690667223547, -1.112240025338166033E-15 ) ) ;
#34457 = CARTESIAN_POINT ( 'NONE',  ( 18.49687500061452283, 6.054752690667223547, 3.707466751127219781E-16 ) ) ;
#34458 = CARTESIAN_POINT ( 'NONE',  ( 24.17812500061451786, 6.421520780324663323E-16, -5.243569643749999010 ) ) ;
#34459 = CARTESIAN_POINT ( 'NONE',  ( 27.18750000000000000, 5.773502691896255534, 3.535250795749688401E-16 ) ) ;
#34460 = CARTESIAN_POINT ( 'NONE',  ( 8.484601909799253346E-16, 16.06250000000000000, 34.61880215351700230 ) ) ;
#34461 = CARTESIAN_POINT ( 'NONE',  ( 29.61562500061451431, 3.027376345333613106, -5.243569643749998122 ) ) ;
#34462 = CARTESIAN_POINT ( 'NONE',  ( 10.83750000122903501, -4.330127018922194537, 2.499999999999995559 ) ) ;
#34463 = CARTESIAN_POINT ( 'NONE',  ( 7.312500001229033764, -4.330127018922190985, -2.500000000000001332 ) ) ;
#34464 = FACE_OUTER_BOUND ( 'NONE', #25236, .T. ) ;
#34465 = CARTESIAN_POINT ( 'NONE',  ( 28.31250000122903288, 0.000000000000000000, 4.999999999999998224 ) ) ;
#34466 = CARTESIAN_POINT ( 'NONE',  ( -2.000000000000001776, 19.04374999877096641, 33.46410161513775705 ) ) ;
#34467 = CARTESIAN_POINT ( 'NONE',  ( 16.96875000122903288, 2.886751345948126879, 4.999999999999999112 ) ) ;
#34468 = CARTESIAN_POINT ( 'NONE',  ( 10.47187500061451715, 3.027376345333611329, 5.243569643749999010 ) ) ;
#34469 = FACE_OUTER_BOUND ( 'NONE', #5485, .T. ) ;
#34470 = CARTESIAN_POINT ( 'NONE',  ( 18.29062500061451502, -3.027376345333610441, -5.243569643749999898 ) ) ;
#34471 = CARTESIAN_POINT ( 'NONE',  ( 12.08437500061451608, 6.421520780324663323E-16, -5.243569643749999010 ) ) ;
#34472 = CARTESIAN_POINT ( 'NONE',  ( 3.140625000614516882, 6.054752690667223547, 3.707466751127219781E-16 ) ) ;
#34473 = CARTESIAN_POINT ( 'NONE',  ( 20.33437500061451786, 4.541064518000418104, 2.621784821874999949 ) ) ;
#34474 = CARTESIAN_POINT ( 'NONE',  ( 7.096875000614517148, -3.027376345333610441, -5.243569643749999898 ) ) ;
#34475 = CARTESIAN_POINT ( 'NONE',  ( 2.953125000614516438, -4.541064518000417216, -2.621784821875001281 ) ) ;
#34476 = CARTESIAN_POINT ( 'NONE',  ( 4.000000000000000000, 16.13749999999999929, 27.69059892324149885 ) ) ;
#34477 = CARTESIAN_POINT ( 'NONE',  ( 10.07812500061451644, -4.541064518000419881, 2.621784821874995952 ) ) ;
#34478 = CARTESIAN_POINT ( 'NONE',  ( 20.54062500061451502, -3.027376345333610441, -5.243569643749999898 ) ) ;
#34479 = EDGE_LOOP ( 'NONE', ( #15253, #18674, #9300, #53415 ) ) ;
#34480 = CARTESIAN_POINT ( 'NONE',  ( 6.525000001229033231, 2.886751345948129099, -4.999999999999998224 ) ) ;
#34481 = CARTESIAN_POINT ( 'NONE',  ( 14.46562500061451750, 3.027376345333611329, 5.243569643749999010 ) ) ;
#34482 = CARTESIAN_POINT ( 'NONE',  ( 13.26562500061451644, -6.054752690667223547, -1.112240025338166033E-15 ) ) ;
#34483 = CARTESIAN_POINT ( 'NONE',  ( 24.75937500061451502, 4.119189519843966529, -2.378215178124998275 ) ) ;
#34484 = CARTESIAN_POINT ( 'NONE',  ( 12.41249999999999964, 2.886751345948126879, 4.999999999999999112 ) ) ;
#34485 = CARTESIAN_POINT ( 'NONE',  ( 9.187500001229034652, 6.123233995736764310E-16, -4.999999999999998224 ) ) ;
#34486 = CARTESIAN_POINT ( 'NONE',  ( 5.765625000614519102, 3.027376345333613106, -5.243569643749998122 ) ) ;
#34487 = ADVANCED_FACE ( 'NONE', ( #55154 ), #4552, .T. ) ;
#34488 = CARTESIAN_POINT ( 'NONE',  ( 18.33750000122903501, 4.330127018922191873, 2.499999999999999556 ) ) ;
#34489 = CARTESIAN_POINT ( 'NONE',  ( 26.69999999999999929, 4.330127018922192761, -2.499999999999997780 ) ) ;
#34490 = CARTESIAN_POINT ( 'NONE',  ( 2.121784821874999061, 10.25937500061451857, -33.67503911421598417 ) ) ;
#34491 = CARTESIAN_POINT ( 'NONE',  ( 0.000000000000000000, 20.00000000000000000, 30.00000000000000000 ) ) ;
#34492 = CARTESIAN_POINT ( 'NONE',  ( 2.887500001229035274, 6.123233995736764310E-16, -4.999999999999998224 ) ) ;
#34493 = CARTESIAN_POINT ( 'NONE',  ( 4.000000000000000000, 14.78749999999999964, 27.69059892324149885 ) ) ;
#34494 = CARTESIAN_POINT ( 'NONE',  ( 19.32187500061451857, 3.027376345333613106, -5.243569643749998122 ) ) ;
#34495 = CARTESIAN_POINT ( 'NONE',  ( 1.592000809091587073E-14, 16.40000000122903501, 26.00000000000000000 ) ) ;
#34496 = CARTESIAN_POINT ( 'NONE',  ( 16.75312500061451715, 0.000000000000000000, 5.243569643749999010 ) ) ;
#34497 = CARTESIAN_POINT ( 'NONE',  ( 9.581250001229033586, 6.123233995736764310E-16, -4.999999999999998224 ) ) ;
#34498 = CARTESIAN_POINT ( 'NONE',  ( 30.00000000000000000, 0.000000000000000000, 4.999999999999998224 ) ) ;
#34499 = CARTESIAN_POINT ( 'NONE',  ( 28.92187500061451644, 3.027376345333611329, 5.243569643749999010 ) ) ;
#34500 = CARTESIAN_POINT ( 'NONE',  ( 26.67187500061451644, 3.027376345333611329, 5.243569643749999010 ) ) ;
#34501 = CARTESIAN_POINT ( 'NONE',  ( 17.89687500061451431, 4.119189519843966529, -2.378215178124998275 ) ) ;
#34502 = CARTESIAN_POINT ( 'NONE',  ( 12.32812500061451821, -4.541064518000419881, 2.621784821874995952 ) ) ;
#34503 = CARTESIAN_POINT ( 'NONE',  ( 9.984375000614518214, 4.541064518000418104, 2.621784821874999949 ) ) ;
#34504 = ORIENTED_EDGE ( 'NONE', *, *, #38215, .T. ) ;
#34505 = CARTESIAN_POINT ( 'NONE',  ( 9.299999999999998934, 0.000000000000000000, 4.999999999999998224 ) ) ;
#34506 = CARTESIAN_POINT ( 'NONE',  ( 19.37812500061451715, 4.541064518000418104, 2.621784821874999949 ) ) ;
#34507 = CARTESIAN_POINT ( 'NONE',  ( 0.000000000000000000, 20.00000000000000000, -30.00000000000000000 ) ) ;
#34508 = CARTESIAN_POINT ( 'NONE',  ( 20.43749999999999645, 5.773502691896255534, 3.535250795749688401E-16 ) ) ;
#34509 = CARTESIAN_POINT ( 'NONE',  ( 9.787499999999999645, -2.886751345948129988, 4.999999999999997335 ) ) ;
#34510 = CARTESIAN_POINT ( 'NONE',  ( 21.11250000122903359, 0.000000000000000000, 4.999999999999998224 ) ) ;
#34511 = CARTESIAN_POINT ( 'NONE',  ( 16.07812500061451289, 6.421520780324663323E-16, -5.243569643749999010 ) ) ;
#34512 = CARTESIAN_POINT ( 'NONE',  ( 10.65937500061451892, 2.746126346562645981, -4.756430356249997438 ) ) ;
#34513 = ORIENTED_EDGE ( 'NONE', *, *, #72602, .T. ) ;
#34514 = CARTESIAN_POINT ( 'NONE',  ( 19.50000000000000000, 4.330127018922192761, -2.499999999999997780 ) ) ;
#34515 = CARTESIAN_POINT ( 'NONE',  ( 22.01249999999999574, -5.773502691896255534, -1.060575238724906372E-15 ) ) ;
#34516 = CARTESIAN_POINT ( 'NONE',  ( 21.60937500061451644, 4.541064518000418104, -2.621784821874998173 ) ) ;
#34517 = CARTESIAN_POINT ( 'NONE',  ( 25.37812500061451715, -4.541064518000419881, 2.621784821874995952 ) ) ;
#34518 = ORIENTED_EDGE ( 'NONE', *, *, #48920, .T. ) ;
#34519 = CARTESIAN_POINT ( 'NONE',  ( 19.65000000000000213, 0.000000000000000000, 4.999999999999998224 ) ) ;
#34520 = CARTESIAN_POINT ( 'NONE',  ( 7.265625000614516438, 3.027376345333611329, 5.243569643749999010 ) ) ;
#34521 = CARTESIAN_POINT ( 'NONE',  ( 9.093750001229031099, -2.886751345948126435, -5.000000000000000000 ) ) ;
#34522 = CARTESIAN_POINT ( 'NONE',  ( 13.83749999999999858, -2.886751345948129988, 4.999999999999997335 ) ) ;
#34523 = CARTESIAN_POINT ( 'NONE',  ( 9.001249775931846008E-16, 16.76562500061451999, 34.90005215228797653 ) ) ;
#34524 = CARTESIAN_POINT ( 'NONE',  ( 28.97812500061451502, -4.541064518000419881, 2.621784821874995952 ) ) ;
#34525 = CARTESIAN_POINT ( 'NONE',  ( 25.77187500061451075, 3.027376345333611329, 5.243569643749999010 ) ) ;
#34526 = EDGE_LOOP ( 'NONE', ( #57629, #21626, #22615, #55173 ) ) ;
#34527 = CARTESIAN_POINT ( 'NONE',  ( 22.97812500061451857, 4.541064518000418104, 2.621784821874999949 ) ) ;
#34528 = CARTESIAN_POINT ( 'NONE',  ( 25.62187500061451573, 3.027376345333613106, -5.243569643749998122 ) ) ;
#34529 = CARTESIAN_POINT ( 'NONE',  ( 4.243569643749999010, 18.71562500061458678, -32.45002607614398471 ) ) ;
#34530 = CARTESIAN_POINT ( 'NONE',  ( 11.36250000000000071, 2.886751345948129099, -4.999999999999998224 ) ) ;
#34531 = CARTESIAN_POINT ( 'NONE',  ( 9.103125000614515017, 0.000000000000000000, 5.243569643749999010 ) ) ;
#34532 = CARTESIAN_POINT ( 'NONE',  ( 29.25937500061451502, 4.119189519843966529, -2.378215178124998275 ) ) ;
#34533 = CARTESIAN_POINT ( 'NONE',  ( 28.75312500061451715, 4.541064518000418104, -2.621784821874998173 ) ) ;
#34534 = CARTESIAN_POINT ( 'NONE',  ( 25.97812500061451502, 6.421520780324663323E-16, -5.243569643749999010 ) ) ;
#34535 = CARTESIAN_POINT ( 'NONE',  ( 28.39687500061451431, 0.000000000000000000, 4.756430356249998326 ) ) ;
#34536 = CARTESIAN_POINT ( 'NONE',  ( 13.28437500061451715, -4.119189519843968306, 2.378215178124996054 ) ) ;
#34537 = CARTESIAN_POINT ( 'NONE',  ( 18.64687500061451786, -3.027376345333614438, 5.243569643749998122 ) ) ;
#34538 = CARTESIAN_POINT ( 'NONE',  ( -2.121784821874996840, 11.38437500061451679, 33.67503911421598417 ) ) ;
#34539 = CARTESIAN_POINT ( 'NONE',  ( 19.47187500061451360, 3.027376345333611329, 5.243569643749999010 ) ) ;
#34540 = CARTESIAN_POINT ( 'NONE',  ( 28.35937500061451289, 4.541064518000418104, -2.621784821874998173 ) ) ;
#34541 = CARTESIAN_POINT ( 'NONE',  ( 4.243569643749999010, 17.42187500061451999, 27.54997392385601174 ) ) ;
#34542 = CARTESIAN_POINT ( 'NONE',  ( 6.815625000614517148, 3.027376345333611329, 5.243569643749999010 ) ) ;
#34543 = CARTESIAN_POINT ( 'NONE',  ( -3.999999999999999112, 18.16250000000000142, -32.30940107675850470 ) ) ;
#34544 = EDGE_CURVE ( 'NONE', #21883, #38944, #54682, .T. ) ;
#34545 = CARTESIAN_POINT ( 'NONE',  ( 4.546875000614517326, 6.054752690667223547, 3.707466751127219781E-16 ) ) ;
#34546 = CARTESIAN_POINT ( 'NONE',  ( 1.071796769724491893, 15.63259618943233598, -26.00000000000000355 ) ) ;
#34547 = CARTESIAN_POINT ( 'NONE',  ( 6.890625000614516438, -3.027376345333614438, 5.243569643749998122 ) ) ;
#34548 = CARTESIAN_POINT ( 'NONE',  ( 12.30937500061451573, 0.000000000000000000, 5.243569643749999010 ) ) ;
#34549 = FILL_AREA_STYLE ('',( #11311 ) ) ;
#34550 = CARTESIAN_POINT ( 'NONE',  ( 18.41250000122903430, 0.000000000000000000, 4.999999999999998224 ) ) ;
#34551 = CARTESIAN_POINT ( 'NONE',  ( 6.684375000614518392, 6.421520780324663323E-16, -5.243569643749999010 ) ) ;
#34552 = CARTESIAN_POINT ( 'NONE',  ( 8.428125000614517859, 6.421520780324663323E-16, -5.243569643749999010 ) ) ;
#34553 = CARTESIAN_POINT ( 'NONE',  ( 4.087500001229035007, -4.330127018922194537, 2.499999999999995559 ) ) ;
#34554 = CARTESIAN_POINT ( 'NONE',  ( 22.25625000122903074, 4.330127018922192761, -2.499999999999997780 ) ) ;
#34555 = CARTESIAN_POINT ( 'NONE',  ( 15.57187500061451679, -6.054752690667223547, -1.112240025338166033E-15 ) ) ;
#34556 = DIRECTION ( 'NONE',  ( 1.000000000000000000, 0.000000000000000000, 0.000000000000000000 ) ) ;
#34557 = ORIENTED_EDGE ( 'NONE', *, *, #37950, .T. ) ;
#34558 = CARTESIAN_POINT ( 'NONE',  ( 25.60312500061451502, 4.541064518000418104, -2.621784821874998173 ) ) ;
#34559 = CARTESIAN_POINT ( 'NONE',  ( 10.64062500061451644, -3.027376345333610441, -5.243569643749999898 ) ) ;
#34560 = CARTESIAN_POINT ( 'NONE',  ( 27.87187500061451573, 3.027376345333612662, -5.243569643749998122 ) ) ;
#34561 = CARTESIAN_POINT ( 'NONE',  ( 10.52812500061451750, -4.541064518000419881, 2.621784821874995952 ) ) ;
#34562 = CARTESIAN_POINT ( 'NONE',  ( 30.00000000000000000, 0.000000000000000000, 4.999999999999998224 ) ) ;
#34563 = CARTESIAN_POINT ( 'NONE',  ( 13.61250000122903359, -4.330127018922190985, -2.500000000000001332 ) ) ;
#34564 = CARTESIAN_POINT ( 'NONE',  ( 26.95312500061451644, 4.541064518000418104, -2.621784821874998173 ) ) ;
#34565 = CARTESIAN_POINT ( 'NONE',  ( -3.000416591977282496E-16, 12.04062500061451857, -34.90005215228797653 ) ) ;
#34566 = CARTESIAN_POINT ( 'NONE',  ( 12.71250000122903145, -4.330127018922190985, -2.500000000000001332 ) ) ;
#34567 = CARTESIAN_POINT ( 'NONE',  ( 10.98750000000000071, 5.773502691896255534, 3.535250795749688894E-16 ) ) ;
#34568 = CARTESIAN_POINT ( 'NONE',  ( 20.61562500061451431, 3.027376345333613106, -5.243569643749998122 ) ) ;
#34569 = CARTESIAN_POINT ( 'NONE',  ( 7.171875000614516438, 3.027376345333612662, -5.243569643749998122 ) ) ;
#34570 = EDGE_CURVE ( 'NONE', #47360, #29982, #39624, .T. ) ;
#34571 = CARTESIAN_POINT ( 'NONE',  ( 19.65000000000000213, 0.000000000000000000, 4.999999999999998224 ) ) ;
#34572 = CARTESIAN_POINT ( 'NONE',  ( 6.862500001229034474, -4.330127018922190985, -2.500000000000001332 ) ) ;
#34573 = CARTESIAN_POINT ( 'NONE',  ( 15.48750000122903359, 6.123233995736764310E-16, -4.999999999999998224 ) ) ;
#34574 = CARTESIAN_POINT ( 'NONE',  ( 13.11562500061451786, 3.027376345333611329, 5.243569643749999010 ) ) ;
#34575 = CARTESIAN_POINT ( 'NONE',  ( 16.56562500061451715, 3.027376345333613106, -5.243569643749998122 ) ) ;
#34576 = CARTESIAN_POINT ( 'NONE',  ( 26.28750000122903430, 6.123233995736764310E-16, -4.999999999999998224 ) ) ;
#34577 = CARTESIAN_POINT ( 'NONE',  ( 20.73750000000000071, -2.886751345948125991, -5.000000000000000000 ) ) ;
#34578 = CARTESIAN_POINT ( 'NONE',  ( 23.44687500061451502, 6.054752690667223547, 3.707466751127219781E-16 ) ) ;
#34579 = CYLINDRICAL_SURFACE ( 'NONE', #67732, 4.999999999999998224 ) ;
#34580 = CARTESIAN_POINT ( 'NONE',  ( 9.112500001229033586, -4.330127018922190985, -2.500000000000001332 ) ) ;
#34581 = CARTESIAN_POINT ( 'NONE',  ( 9.946875000614516793, 6.054752690667223547, 3.707466751127219781E-16 ) ) ;
#34582 = CARTESIAN_POINT ( 'NONE',  ( 25.13437500061451502, 6.421520780324663323E-16, -5.243569643749999010 ) ) ;
#34583 = CARTESIAN_POINT ( 'NONE',  ( 23.69999999999999929, 0.000000000000000000, 4.999999999999998224 ) ) ;
#34584 = CARTESIAN_POINT ( 'NONE',  ( 23.76562500061451644, 3.027376345333613106, -5.243569643749998122 ) ) ;
#34585 = CARTESIAN_POINT ( 'NONE',  ( 27.30937500061451573, -4.541064518000417216, -2.621784821875001281 ) ) ;
#34586 = CARTESIAN_POINT ( 'NONE',  ( -1.878215178124999163, 16.05312499938548143, 26.74683588394047007 ) ) ;
#34587 = CARTESIAN_POINT ( 'NONE',  ( 17.96249999999999858, -5.773502691896255534, -1.060575238724906372E-15 ) ) ;
#34588 = CARTESIAN_POINT ( 'NONE',  ( 8.896875000614517859, -3.027376345333610441, -5.243569643749999898 ) ) ;
#34589 = DIRECTION ( 'NONE',  ( 0.000000000000000000, 1.000000000000000000, -8.673617379884036705E-17 ) ) ;
#34590 = CARTESIAN_POINT ( 'NONE',  ( 26.99062500061451431, 6.054752690667223547, 3.707466751127219781E-16 ) ) ;
#34591 = CARTESIAN_POINT ( 'NONE',  ( 5.709375000614517859, -4.541064518000417216, -2.621784821875001281 ) ) ;
#34592 = CARTESIAN_POINT ( 'NONE',  ( 1.592000809091587073E-14, 16.40000000122903501, -34.00000000000000000 ) ) ;
#34593 = CARTESIAN_POINT ( 'NONE',  ( 25.13437500061451502, 6.421520780324663323E-16, -5.243569643749999010 ) ) ;
#34594 = CARTESIAN_POINT ( 'NONE',  ( 2.121784821875001281, 10.05312500061459424, 33.67503911421598417 ) ) ;
#34595 = CARTESIAN_POINT ( 'NONE',  ( 16.42500000000000071, 4.330127018922191873, 2.499999999999999556 ) ) ;
#34596 = VERTEX_POINT ( 'NONE', #17064 ) ;
#34597 = CARTESIAN_POINT ( 'NONE',  ( 27.63749999999999929, 5.773502691896255534, 3.535250795749688894E-16 ) ) ;
#34598 = CARTESIAN_POINT ( 'NONE',  ( 27.45937500061451786, 4.541064518000418104, -2.621784821874998173 ) ) ;
#34599 = ORIENTED_EDGE ( 'NONE', *, *, #49494, .T. ) ;
#34600 = CARTESIAN_POINT ( 'NONE',  ( 16.30312500061451786, 0.000000000000000000, 5.243569643749999010 ) ) ;
#34601 = CARTESIAN_POINT ( 'NONE',  ( 6.890625000614516438, -3.027376345333614438, 5.243569643749998122 ) ) ;
#34602 = CARTESIAN_POINT ( 'NONE',  ( 20.07187500061451502, 5.824947211148865298E-16, -4.756430356249998326 ) ) ;
#34603 = CARTESIAN_POINT ( 'NONE',  ( 3.759375000614517681, 0.000000000000000000, 5.243569643749999010 ) ) ;
#34604 = CARTESIAN_POINT ( 'NONE',  ( 14.66250000122903252, 4.330127018922192761, -2.499999999999997780 ) ) ;
#34605 = CARTESIAN_POINT ( 'NONE',  ( 21.48750000000000071, -2.886751345948129988, 4.999999999999997335 ) ) ;
#34606 = CARTESIAN_POINT ( 'NONE',  ( 29.88749999999999929, 5.773502691896255534, 3.535250795749688894E-16 ) ) ;
#34607 = CARTESIAN_POINT ( 'NONE',  ( 5.371875000614516615, 3.027376345333613106, -5.243569643749998122 ) ) ;
#34608 = CARTESIAN_POINT ( 'NONE',  ( 10.09687500061451715, -3.027376345333614438, 5.243569643749998122 ) ) ;
#34609 = CARTESIAN_POINT ( 'NONE',  ( 22.77187500061451786, -6.054752690667223547, -1.112240025338166033E-15 ) ) ;
#34610 = CARTESIAN_POINT ( 'NONE',  ( 11.56875000122903430, 2.886751345948126879, 4.999999999999998224 ) ) ;
#34611 = EDGE_LOOP ( 'NONE', ( #10499, #6890, #58589, #21385 ) ) ;
#34612 = CARTESIAN_POINT ( 'NONE',  ( 4.921875000614518214, 3.027376345333613106, -5.243569643749998122 ) ) ;
#34613 = CARTESIAN_POINT ( 'NONE',  ( 7.546875000614517326, -3.027376345333610441, -5.243569643749999898 ) ) ;
#34614 = CARTESIAN_POINT ( 'NONE',  ( 17.51249999999999929, -5.773502691896255534, -1.060575238724906372E-15 ) ) ;
#34615 = CARTESIAN_POINT ( 'NONE',  ( 15.70312500061451644, 4.541064518000418104, -2.621784821874998173 ) ) ;
#34616 = CARTESIAN_POINT ( 'NONE',  ( 3.999999999999998668, 19.66249999999999787, 32.30940107675850470 ) ) ;
#34617 = CARTESIAN_POINT ( 'NONE',  ( 22.16250000000000142, 2.886751345948073588, -5.000000000000094147 ) ) ;
#34618 = CARTESIAN_POINT ( 'NONE',  ( 20.44687500061451857, -2.746126346562646425, 4.756430356249996549 ) ) ;
#34619 = CARTESIAN_POINT ( 'NONE',  ( 9.403125000614517504, 4.541064518000418104, -2.621784821874998173 ) ) ;
#34620 = CARTESIAN_POINT ( 'NONE',  ( 26.25937500061451857, 0.000000000000000000, 5.243569643749999010 ) ) ;
#34621 = DIRECTION ( 'NONE',  ( 0.000000000000000000, 1.000000000000000000, -8.673617379884036705E-17 ) ) ;
#34622 = CARTESIAN_POINT ( 'NONE',  ( 25.28437500061451715, 4.541064518000418104, 2.621784821874999949 ) ) ;
#34623 = CARTESIAN_POINT ( 'NONE',  ( 7.837499999999999467, 5.773502691896255534, 3.535250795749688894E-16 ) ) ;
#34624 = CARTESIAN_POINT ( 'NONE',  ( -3.999999999999999556, 12.87500000122903465, 27.69059892324149530 ) ) ;
#34626 =( BOUNDED_CURVE ( )  B_SPLINE_CURVE ( 2, ( #45603, #24131, #12324, #57023, #46681, #7509, #62931 ),
 .UNSPECIFIED., .F., .F. ) 
 B_SPLINE_CURVE_WITH_KNOTS ( ( 3, 2, 2, 3 ),
 ( 0.2999999999999999889, 0.3027777777777777568, 0.3055555555555555802, 0.3083333333333333481 ),
 .UNSPECIFIED. ) 
 CURVE ( )  GEOMETRIC_REPRESENTATION_ITEM ( )  RATIONAL_B_SPLINE_CURVE ( ( 1.000000000000000000, 0.8660254037844387076, 1.000000000000000000, 0.8660254037844387076, 1.000000000000000000, 0.8660254037844387076, 1.000000000000000000 ) ) 
 REPRESENTATION_ITEM ( '' )  );
#34625 = CARTESIAN_POINT ( 'NONE',  ( 7.162500001229032520, 0.000000000000000000, 4.999999999999998224 ) ) ;
#34627 = ADVANCED_FACE ( 'NONE', ( #5267 ), #61798, .T. ) ;
#34628 = CARTESIAN_POINT ( 'NONE',  ( 16.62187500061451573, 3.027376345333613106, -5.243569643749998122 ) ) ;
#34629 = CARTESIAN_POINT ( 'NONE',  ( 11.29687500061451644, 6.054752690667223547, 3.707466751127219781E-16 ) ) ;
#34630 = CARTESIAN_POINT ( 'NONE',  ( -2.672702088255949472E-15, 13.90624999877096890, 26.00000000000000000 ) ) ;
#34631 = VERTEX_POINT ( 'NONE', #29912 ) ;
#34632 = CARTESIAN_POINT ( 'NONE',  ( 15.70312500061451644, 4.541064518000418104, -2.621784821874998173 ) ) ;
#34633 = CARTESIAN_POINT ( 'NONE',  ( 25.76250000122903216, -4.330127018922190985, -2.500000000000001332 ) ) ;
#34634 = CARTESIAN_POINT ( 'NONE',  ( 12.90937500061451537, -4.541064518000417216, -2.621784821875001281 ) ) ;
#34635 = CARTESIAN_POINT ( 'NONE',  ( -3.137519842735245283E-14, 12.57500000122903572, 34.00000000000000000 ) ) ;
#34636 = CARTESIAN_POINT ( 'NONE',  ( 13.75312500061451715, -4.541064518000417216, -2.621784821875001281 ) ) ;
#34637 = EDGE_CURVE ( 'NONE', #59354, #30864, #31146, .T. ) ;
#34638 = LINE ( 'NONE', #35007, #31523 ) ;
#34639 = CARTESIAN_POINT ( 'NONE',  ( 25.47187500061451715, -6.054752690667223547, -1.112240025338166033E-15 ) ) ;
#34640 = CARTESIAN_POINT ( 'NONE',  ( 2.892512340070121812, -4.078410086807788382, 3.295700467049730520 ) ) ;
#34641 = CARTESIAN_POINT ( 'NONE',  ( 11.92500000122903181, 2.886751345948129099, -4.999999999999998224 ) ) ;
#34642 = CARTESIAN_POINT ( 'NONE',  ( 8.446875000614518569, -2.746126346562641984, -4.756430356249999214 ) ) ;
#34643 = DIRECTION ( 'NONE',  ( 0.000000000000000000, 0.000000000000000000, -1.000000000000000000 ) ) ;
#34644 = CARTESIAN_POINT ( 'NONE',  ( -2.121784821874996840, 16.78437500061452070, -26.32496088578401583 ) ) ;
#34645 = EDGE_CURVE ( 'NONE', #14992, #44258, #47632, .T. ) ;
#34646 = CARTESIAN_POINT ( 'NONE',  ( 19.13437500061451857, -4.541064518000419881, 2.621784821874995952 ) ) ;
#34647 = CARTESIAN_POINT ( 'NONE',  ( 20.17500000122903359, 2.886751345948126879, 4.999999999999999112 ) ) ;
#34648 = CARTESIAN_POINT ( 'NONE',  ( 14.55937500061451573, 0.000000000000000000, 5.243569643749999010 ) ) ;
#34649 = CARTESIAN_POINT ( 'NONE',  ( -3.000416591977282496E-16, 10.29687500061451644, 25.09994784771203058 ) ) ;
#34650 = CARTESIAN_POINT ( 'NONE',  ( 22.91250000122903430, 0.000000000000000000, 4.999999999999998224 ) ) ;
#34651 = CARTESIAN_POINT ( 'NONE',  ( 15.70312500061451644, 4.541064518000418104, -2.621784821874998173 ) ) ;
#34652 = CARTESIAN_POINT ( 'NONE',  ( 29.09062500061451573, -3.027376345333610441, -5.243569643749999898 ) ) ;
#34653 = VERTEX_POINT ( 'NONE', #64622 ) ;
#34654 = EDGE_LOOP ( 'NONE', ( #44898, #210, #1919, #8018 ) ) ;
#34655 = CARTESIAN_POINT ( 'NONE',  ( 19.27500000000000213, -4.330127018922194537, 2.499999999999995559 ) ) ;
#34656 = FACE_OUTER_BOUND ( 'NONE', #54791, .T. ) ;
#34657 = CARTESIAN_POINT ( 'NONE',  ( 2.953125000614516438, -4.541064518000417216, -2.621784821875001281 ) ) ;
#34658 = CARTESIAN_POINT ( 'NONE',  ( 15.71250000122903501, 0.000000000000000000, 4.999999999999998224 ) ) ;
#34659 = CARTESIAN_POINT ( 'NONE',  ( 20.65312500061451573, 4.541064518000418104, -2.621784821874998173 ) ) ;
#34660 = CARTESIAN_POINT ( 'NONE',  ( 22.07812500061451644, 4.541064518000418104, 2.621784821874999949 ) ) ;
#34661 = CARTESIAN_POINT ( 'NONE',  ( 2.878125000614517592, -4.541064518000419881, 2.621784821874995952 ) ) ;
#34662 = CARTESIAN_POINT ( 'NONE',  ( 27.26249999999999929, 2.886751345948126879, 4.999999999999999112 ) ) ;
#34663 = CARTESIAN_POINT ( 'NONE',  ( 2.000000000000001332, 11.71250000122903501, 33.46410161513774995 ) ) ;
#34664 = CARTESIAN_POINT ( 'NONE',  ( 9.459375000614517859, 4.119189519843966529, -2.378215178124998275 ) ) ;
#34665 = CARTESIAN_POINT ( 'NONE',  ( 29.40937500061451715, 0.000000000000000000, 5.243569643749999010 ) ) ;
#34666 = CARTESIAN_POINT ( 'NONE',  ( -1.999999999999997113, 12.08750000122903501, -26.53589838486224295 ) ) ;
#34667 = CARTESIAN_POINT ( 'NONE',  ( 4.243569643749999010, 16.97187500061451360, -32.45002607614398471 ) ) ;
#34668 = EDGE_CURVE ( 'NONE', #66446, #33991, #16920, .T. ) ;
#34669 = CARTESIAN_POINT ( 'NONE',  ( 5.212500001229032343, 4.330127018922192761, -2.499999999999997780 ) ) ;
#34670 = CARTESIAN_POINT ( 'NONE',  ( 8.962500000000002132, -5.773502691896255534, -1.060575238724906372E-15 ) ) ;
#34671 = CARTESIAN_POINT ( 'NONE',  ( 5.062500001229035540, -4.330127018922190985, -2.500000000000001332 ) ) ;
#34672 = CARTESIAN_POINT ( 'NONE',  ( 8.934375000614517504, 6.421520780324663323E-16, -5.243569643749999010 ) ) ;
#34673 = CARTESIAN_POINT ( 'NONE',  ( 3.947751918878622757, -3.068428716296062841, 3.947751918878600108 ) ) ;
#34674 = CARTESIAN_POINT ( 'NONE',  ( 3.571875000614517237, 3.027376345333613106, -5.243569643749998122 ) ) ;
#34675 = CARTESIAN_POINT ( 'NONE',  ( 28.08749999999999858, 5.773502691896255534, 3.535250795749688401E-16 ) ) ;
#34676 = CARTESIAN_POINT ( 'NONE',  ( 17.06250000122903288, 0.000000000000000000, 4.999999999999998224 ) ) ;
#34677 = CARTESIAN_POINT ( 'NONE',  ( 7.996875000614519280, -3.027376345333610441, -5.243569643749999898 ) ) ;
#34678 = CARTESIAN_POINT ( 'NONE',  ( 13.43437500061451750, 6.421520780324663323E-16, -5.243569643749999010 ) ) ;
#34679 = CYLINDRICAL_SURFACE ( 'NONE', #10049, 4.999999999999998224 ) ;
#34680 = CARTESIAN_POINT ( 'NONE',  ( 6.787500000000001421, -2.886751345948125991, -5.000000000000000000 ) ) ;
#34681 = CARTESIAN_POINT ( 'NONE',  ( 4.243569643749999898, 17.77812500061459744, 30.00000000000000000 ) ) ;
#34682 = CARTESIAN_POINT ( 'NONE',  ( 20.70937500061451786, 4.541064518000418104, -2.621784821874998173 ) ) ;
#34683 = SURFACE_SIDE_STYLE ('',( #45422 ) ) ;
#34684 = CARTESIAN_POINT ( 'NONE',  ( 25.98750000122903003, 4.330127018922191873, 2.499999999999999556 ) ) ;
#34685 = CARTESIAN_POINT ( 'NONE',  ( 17.03437500061451715, 5.492252693125287522, 3.363034840372157021E-16 ) ) ;
#34686 = CARTESIAN_POINT ( 'NONE',  ( 21.96562500061451573, 3.027376345333613106, -5.243569643749998122 ) ) ;
#34687 = CARTESIAN_POINT ( 'NONE',  ( 16.45312500061451289, -4.541064518000417216, -2.621784821875001281 ) ) ;
#34688 = CARTESIAN_POINT ( 'NONE',  ( 26.48437500061450933, 5.492252693125287522, 3.363034840372157021E-16 ) ) ;
#34689 = CARTESIAN_POINT ( 'NONE',  ( 12.64687500061451608, 6.054752690667223547, 3.707466751127219781E-16 ) ) ;
#34690 = CARTESIAN_POINT ( 'NONE',  ( 29.66249999999999432, -5.773502691896255534, -1.060575238724906372E-15 ) ) ;
#34691 = CARTESIAN_POINT ( 'NONE',  ( 26.02500000122903145, 2.886751345948126879, 4.999999999999999112 ) ) ;
#34692 = AXIS2_PLACEMENT_3D ( 'NONE', #41315, #6238, #63825 ) ;
#34693 = CARTESIAN_POINT ( 'NONE',  ( 28.64999999999999858, 0.000000000000000000, 4.999999999999998224 ) ) ;
#34694 = CARTESIAN_POINT ( 'NONE',  ( 11.59687500061451892, -3.027376345333610441, -5.243569643749999898 ) ) ;
#34695 = CARTESIAN_POINT ( 'NONE',  ( 29.74687500061451217, 6.054752690667223547, 3.707466751127219781E-16 ) ) ;
#34696 = CARTESIAN_POINT ( 'NONE',  ( 3.609375000614516882, 4.541064518000418104, -2.621784821874998173 ) ) ;
#34697 = CARTESIAN_POINT ( 'NONE',  ( 18.30000000000000071, 0.000000000000000000, 4.999999999999998224 ) ) ;
#34698 = CARTESIAN_POINT ( 'NONE',  ( 23.37187500061451573, 3.027376345333613106, -5.243569643749998122 ) ) ;
#34699 = CARTESIAN_POINT ( 'NONE',  ( 15.23437500061451644, 6.421520780324663323E-16, -5.243569643749999010 ) ) ;
#34700 = CARTESIAN_POINT ( 'NONE',  ( -3.756430356249999214, 18.34062499938548640, 27.83122392262697531 ) ) ;
#34701 = CARTESIAN_POINT ( 'NONE',  ( 25.61250000000000071, -5.773502691896255534, -1.060575238724906372E-15 ) ) ;
#34702 = CARTESIAN_POINT ( 'NONE',  ( 1.999999999999997335, 13.32499999999999929, 33.46410161513775705 ) ) ;
#34703 = CARTESIAN_POINT ( 'NONE',  ( 27.12187500061451573, 2.746126346562643317, 4.756430356249998326 ) ) ;
#34704 = CARTESIAN_POINT ( 'NONE',  ( 17.39062500061451644, -3.027376345333610441, -5.243569643749999898 ) ) ;
#34705 = CARTESIAN_POINT ( 'NONE',  ( 6.937499999999999112, 5.773502691896255534, 3.535250795749688894E-16 ) ) ;
#34706 = CARTESIAN_POINT ( 'NONE',  ( 1.626862140677534273E-15, 13.47500000122903252, 34.00000000000000000 ) ) ;
#34707 = CARTESIAN_POINT ( 'NONE',  ( 14.43750000000000000, -2.886751345948125991, -5.000000000000000000 ) ) ;
#34708 = CARTESIAN_POINT ( 'NONE',  ( 9.001249775931846008E-16, 10.01562500061451644, 34.90005215228797653 ) ) ;
#34709 = CYLINDRICAL_SURFACE ( 'NONE', #45487, 4.999999999999998224 ) ;
#34710 = CARTESIAN_POINT ( 'NONE',  ( 26.07187500061451857, 3.027376345333613106, -5.243569643749998122 ) ) ;
#34711 = ORIENTED_EDGE ( 'NONE', *, *, #63337, .F. ) ;
#34712 = CARTESIAN_POINT ( 'NONE',  ( 20.80312500061451431, 0.000000000000000000, 5.243569643749999010 ) ) ;
#34713 = CARTESIAN_POINT ( 'NONE',  ( 20.44687500061451857, -3.027376345333614438, 5.243569643749998122 ) ) ;
#34714 = CARTESIAN_POINT ( 'NONE',  ( 3.975000000000002753, -4.330127018922194537, 2.499999999999995559 ) ) ;
#34715 = CARTESIAN_POINT ( 'NONE',  ( 6.778125000614518392, 4.541064518000418104, 2.621784821874999949 ) ) ;
#34716 = CARTESIAN_POINT ( 'NONE',  ( 23.27812500061451573, 6.421520780324663323E-16, -5.243569643749999010 ) ) ;
#34717 = CARTESIAN_POINT ( 'NONE',  ( 13.47187500061451537, 3.027376345333613106, -5.243569643749998122 ) ) ;
#34718 = CARTESIAN_POINT ( 'NONE',  ( 16.65937500061452070, 4.541064518000418104, -2.621784821874998173 ) ) ;
#34719 = CARTESIAN_POINT ( 'NONE',  ( 9.001249775931846008E-16, 17.21562500061451928, 34.90005215228797653 ) ) ;
#34720 = CARTESIAN_POINT ( 'NONE',  ( 17.88750000122903216, 4.330127018922191873, 2.499999999999999556 ) ) ;
#34721 = CARTESIAN_POINT ( 'NONE',  ( 15.64687500061451608, -2.746126346562641984, -4.756430356249999214 ) ) ;
#34722 = CARTESIAN_POINT ( 'NONE',  ( 8.878125000614515372, 6.421520780324663323E-16, -5.243569643749999010 ) ) ;
#34723 = CARTESIAN_POINT ( 'NONE',  ( 4.659375000614518925, 0.000000000000000000, 5.243569643749999010 ) ) ;
#34724 = CARTESIAN_POINT ( 'NONE',  ( 4.734375000614518214, -4.541064518000419881, 2.621784821874995952 ) ) ;
#34725 = VERTEX_POINT ( 'NONE', #7872 ) ;
#34726 = EDGE_CURVE ( 'NONE', #44169, #2080, #41851, .T. ) ;
#34727 = CARTESIAN_POINT ( 'NONE',  ( 25.58437500061451431, 6.421520780324663323E-16, -5.243569643749999010 ) ) ;
#34728 = CARTESIAN_POINT ( 'NONE',  ( 16.94062500061451715, -3.027376345333610441, -5.243569643749999898 ) ) ;
#34729 = CARTESIAN_POINT ( 'NONE',  ( 27.93750000122903288, -4.330127018922194537, 2.499999999999995559 ) ) ;
#34730 = CARTESIAN_POINT ( 'NONE',  ( 27.14062500061451644, -3.027376345333614438, 5.243569643749998122 ) ) ;
#34731 = CARTESIAN_POINT ( 'NONE',  ( 22.17187500061451644, 3.027376345333611329, 5.243569643749999010 ) ) ;
#34732 = CARTESIAN_POINT ( 'NONE',  ( 17.05312500061451786, 4.541064518000418104, -2.621784821874998173 ) ) ;
#34733 = CARTESIAN_POINT ( 'NONE',  ( 4.243569643749999898, 16.89687500061451786, 32.45002607614398471 ) ) ;
#34734 = CARTESIAN_POINT ( 'NONE',  ( 21.70312500061451644, 0.000000000000000000, 5.243569643749999010 ) ) ;
#34735 = DIRECTION ( 'NONE',  ( 0.000000000000000000, 0.000000000000000000, 1.000000000000000000 ) ) ;
#34736 = ORIENTED_EDGE ( 'NONE', *, *, #57642, .F. ) ;
#34737 = ORIENTED_EDGE ( 'NONE', *, *, #56333, .T. ) ;
#34738 = CARTESIAN_POINT ( 'NONE',  ( 25.83749999999999858, 5.773502691896255534, 3.535250795749688894E-16 ) ) ;
#34739 = CARTESIAN_POINT ( 'NONE',  ( 3.999999999999998668, 13.96250000000000213, -32.30940107675850470 ) ) ;
#34740 = CARTESIAN_POINT ( 'NONE',  ( 7.320879633048903241E-15, 18.20000000122903216, 26.00000000000000355 ) ) ;
#34741 = CARTESIAN_POINT ( 'NONE',  ( 3.309375000614518836, 0.000000000000000000, 5.243569643749999010 ) ) ;
#34742 = CARTESIAN_POINT ( 'NONE',  ( 10.22812500061451679, 6.421520780324663323E-16, -5.243569643749999010 ) ) ;
#34743 = CARTESIAN_POINT ( 'NONE',  ( 22.35000000122903074, 5.773502691896255534, 3.535250795749688894E-16 ) ) ;
#34744 = CARTESIAN_POINT ( 'NONE',  ( 28.22812500061451502, 6.421520780324663323E-16, -5.243569643749999010 ) ) ;
#34745 = CARTESIAN_POINT ( 'NONE',  ( 27.41250000000000142, -5.773502691896255534, -1.060575238724906372E-15 ) ) ;
#34746 = CARTESIAN_POINT ( 'NONE',  ( 3.999999999999999112, 18.98750000122903359, -30.00000000000000000 ) ) ;
#34747 = DIRECTION ( 'NONE',  ( -0.9848080501874559856, 0.000000000000000000, 0.1736464922939166267 ) ) ;
#34748 = CARTESIAN_POINT ( 'NONE',  ( 9.890625000614516438, 6.054752690667223547, 3.707466751127219781E-16 ) ) ;
#34749 = ORIENTED_EDGE ( 'NONE', *, *, #40081, .F. ) ;
#34750 = CARTESIAN_POINT ( 'NONE',  ( 8.765625000614518214, -6.054752690667223547, -1.112240025338166033E-15 ) ) ;
#34751 = VECTOR ( 'NONE', #57382, 1000.000000000000000 ) ;
#34752 = CARTESIAN_POINT ( 'NONE',  ( 5.278125000614516615, 6.421520780324663323E-16, -5.243569643749999010 ) ) ;
#34753 = CARTESIAN_POINT ( 'NONE',  ( 17.18437500061451573, 4.119189519843966529, 2.378215178124999607 ) ) ;
#34754 = CARTESIAN_POINT ( 'NONE',  ( 30.00000000000000000, 0.000000000000000000, 4.999999999999998224 ) ) ;
#34755 = CARTESIAN_POINT ( 'NONE',  ( 14.47499999999999964, 6.123233995736764310E-16, -4.999999999999998224 ) ) ;
#34757 = CARTESIAN_POINT ( 'NONE',  ( 15.87187500061451573, 3.027376345333611329, 5.243569643749999010 ) ) ;
#34756 = VECTOR ( 'NONE', #70400, 1000.000000000000000 ) ;
#34758 = CARTESIAN_POINT ( 'NONE',  ( 11.51250000122903216, 4.330127018922192761, -2.499999999999997780 ) ) ;
#34759 = CARTESIAN_POINT ( 'NONE',  ( 18.57187500061451857, 3.027376345333611329, 5.243569643749999010 ) ) ;
#34760 = CARTESIAN_POINT ( 'NONE',  ( 17.47499999999999787, -4.330127018922194537, 2.499999999999995559 ) ) ;
#34761 = CARTESIAN_POINT ( 'NONE',  ( 21.49687500061451573, -3.027376345333610441, -5.243569643749999898 ) ) ;
#34762 = CARTESIAN_POINT ( 'NONE',  ( 2.121784821874999061, 14.25312500061451715, -33.67503911421598417 ) ) ;
#34763 = VECTOR ( 'NONE', #5081, 1000.000000000000000 ) ;
#34764 = CARTESIAN_POINT ( 'NONE',  ( 34.99999999999999289, -2.499999999999999556, -5.500000000000000000 ) ) ;
#34765 = CARTESIAN_POINT ( 'NONE',  ( 25.99687500061451573, 4.119189519843966529, -2.378215178124998275 ) ) ;
#34766 = CARTESIAN_POINT ( 'NONE',  ( 1.071796769724489895, 11.76740381056766616, -34.00000000000000000 ) ) ;
#34767 = EDGE_CURVE ( 'NONE', #8342, #48969, #52936, .T. ) ;
#34768 = CARTESIAN_POINT ( 'NONE',  ( 24.85312500061451502, 0.000000000000000000, 5.243569643749999010 ) ) ;
#34769 = CARTESIAN_POINT ( 'NONE',  ( 24.86250000000000426, 2.886751345948146419, -4.999999999999968914 ) ) ;
#34770 = CARTESIAN_POINT ( 'NONE',  ( 27.79687500061451999, -3.027376345333610441, -5.243569643749999898 ) ) ;
#34771 =( BOUNDED_CURVE ( )  B_SPLINE_CURVE ( 2, ( #31504, #59559, #55770, #69927, #48864, #47759, #19296 ),
 .UNSPECIFIED., .F., .F. ) 
 B_SPLINE_CURVE_WITH_KNOTS ( ( 3, 2, 2, 3 ),
 ( 0.6500000000000001332, 0.6527777777777779011, 0.6555555555555556690, 0.6583333333333334370 ),
 .UNSPECIFIED. ) 
 CURVE ( )  GEOMETRIC_REPRESENTATION_ITEM ( )  RATIONAL_B_SPLINE_CURVE ( ( 0.9999999999999946709, 0.8660254037844440367, 1.000000000000000000, 0.8660254037844387076, 1.000000000000000000, 0.8660254037844333785, 1.000000000000005329 ) ) 
 REPRESENTATION_ITEM ( '' )  );
#34772 = CARTESIAN_POINT ( 'NONE',  ( 23.17500000000000071, 4.330127018922191873, 2.499999999999999556 ) ) ;
#34773 = CARTESIAN_POINT ( 'NONE',  ( 7.265625000614516438, 3.027376345333611329, 5.243569643749999010 ) ) ;
#34774 = CARTESIAN_POINT ( 'NONE',  ( 23.70937500061451075, 2.746126346562645981, -4.756430356249997438 ) ) ;
#34775 = CARTESIAN_POINT ( 'NONE',  ( 19.69687500061451857, -3.027376345333610441, -5.243569643749999898 ) ) ;
#34776 = CARTESIAN_POINT ( 'NONE',  ( 11.37187500061451573, -4.119189519843968306, 2.378215178124996054 ) ) ;
#34777 = CARTESIAN_POINT ( 'NONE',  ( 5.128125000614516260, -4.541064518000419881, 2.621784821874995952 ) ) ;
#34778 = CARTESIAN_POINT ( 'NONE',  ( 9.084375000614517859, 4.541064518000418104, 2.621784821874999949 ) ) ;
#34779 = ORIENTED_EDGE ( 'NONE', *, *, #15234, .F. ) ;
#34780 = CARTESIAN_POINT ( 'NONE',  ( 18.15937500061451715, 0.000000000000000000, 5.243569643749999010 ) ) ;
#34781 = CARTESIAN_POINT ( 'NONE',  ( 13.87500000122903288, 2.886751345948193936, 4.999999999999883649 ) ) ;
#34782 = CARTESIAN_POINT ( 'NONE',  ( 27.93750000000000000, -2.886751345948125991, -5.000000000000000000 ) ) ;
#34783 = CARTESIAN_POINT ( 'NONE',  ( 3.487500000000000711, -2.886751345948129988, 4.999999999999997335 ) ) ;
#34784 = CARTESIAN_POINT ( 'NONE',  ( 1.626862140677534273E-15, 16.17500000122903359, 34.00000000000000000 ) ) ;
#34785 = CARTESIAN_POINT ( 'NONE',  ( 17.66249999999999787, 2.886751345948185055, -4.999999999999902300 ) ) ;
#34786 = ORIENTED_EDGE ( 'NONE', *, *, #57824, .T. ) ;
#34787 = CARTESIAN_POINT ( 'NONE',  ( 9.637499999999999289, 5.773502691896255534, 3.535250795749688894E-16 ) ) ;
#34788 = CARTESIAN_POINT ( 'NONE',  ( 11.25937500061451679, 2.746126346562643317, 4.756430356249998326 ) ) ;
#34789 = CARTESIAN_POINT ( 'NONE',  ( 23.72812500061451502, 6.421520780324663323E-16, -5.243569643749999010 ) ) ;
#34790 = CARTESIAN_POINT ( 'NONE',  ( 14.77500000000000036, -4.330127018922194537, 2.499999999999995559 ) ) ;
#34791 = CARTESIAN_POINT ( 'NONE',  ( 11.47500000122903252, 2.886751345948129099, -4.999999999999998224 ) ) ;
#34792 = CARTESIAN_POINT ( 'NONE',  ( 8.990625000614516082, 6.054752690667223547, 3.707466751127219781E-16 ) ) ;
#34793 = CARTESIAN_POINT ( 'NONE',  ( 23.21250000000000213, 2.886751345948126879, 4.999999999999999112 ) ) ;
#34794 = CARTESIAN_POINT ( 'NONE',  ( 21.51562500061451644, 3.027376345333613106, -5.243569643749998122 ) ) ;
#34795 = CARTESIAN_POINT ( 'NONE',  ( 4.898587196589412829E-16, 27.50000000000000000, 34.00000000000000000 ) ) ;
#34796 = CARTESIAN_POINT ( 'NONE',  ( 27.56250000122902932, -4.330127018922190985, -2.500000000000001332 ) ) ;
#34797 = CARTESIAN_POINT ( 'NONE',  ( 2.655984681222220721E-16, 17.25312499938548072, 25.66244784525396483 ) ) ;
#34798 = CARTESIAN_POINT ( 'NONE',  ( 6.524999999999999467, 4.330127018922191873, 2.499999999999999556 ) ) ;
#34799 = AXIS2_PLACEMENT_3D ( 'NONE', #43470, #54913, #9845 ) ;
#34800 = ORIENTED_EDGE ( 'NONE', *, *, #42990, .F. ) ;
#34801 = CARTESIAN_POINT ( 'NONE',  ( 21.10312500061451502, 4.541064518000418104, -2.621784821874998173 ) ) ;
#34802 = CARTESIAN_POINT ( 'NONE',  ( 28.07812500061451289, -4.541064518000419881, 2.621784821874995952 ) ) ;
#34803 = CARTESIAN_POINT ( 'NONE',  ( 27.79687500061451999, -3.027376345333610441, -5.243569643749999898 ) ) ;
#34804 = CARTESIAN_POINT ( 'NONE',  ( 18.15937500061451715, 0.000000000000000000, 5.243569643749999010 ) ) ;
#34805 = CARTESIAN_POINT ( 'NONE',  ( 13.49062500061451608, 6.054752690667223547, 3.707466751127219781E-16 ) ) ;
#34806 = CARTESIAN_POINT ( 'NONE',  ( -4.243569643749999898, 9.903125000614593887, -30.00000000000000000 ) ) ;
#34807 = VECTOR ( 'NONE', #2426, 1000.000000000000000 ) ;
#34808 = CARTESIAN_POINT ( 'NONE',  ( 25.23750000122903359, -4.330127018922194537, 2.499999999999995559 ) ) ;
#34809 = CARTESIAN_POINT ( 'NONE',  ( 22.28437500061451715, -4.119189519843968306, 2.378215178124996054 ) ) ;
#34810 = CARTESIAN_POINT ( 'NONE',  ( 15.92812500061451608, -4.541064518000419881, 2.621784821874995952 ) ) ;
#34811 = CARTESIAN_POINT ( 'NONE',  ( 1.071796769724491893, 13.83259618943233527, 33.99999999999999289 ) ) ;
#34812 = CARTESIAN_POINT ( 'NONE',  ( 3.112500001229034918, 0.000000000000000000, 4.999999999999998224 ) ) ;
#34813 = CARTESIAN_POINT ( 'NONE',  ( 11.97187500061451892, -6.054752690667223547, -1.112240025338166033E-15 ) ) ;
#34814 = CARTESIAN_POINT ( 'NONE',  ( 12.15937500061451892, 4.541064518000418104, -2.621784821874998173 ) ) ;
#34815 = CARTESIAN_POINT ( 'NONE',  ( 21.00937500061451857, -4.541064518000417216, -2.621784821875001281 ) ) ;
#34816 = EDGE_LOOP ( 'NONE', ( #67440, #5642, #22543, #61504 ) ) ;
#34817 = CARTESIAN_POINT ( 'NONE',  ( -5.191270968837347510, 8.550562458943613109, 33.03294266662791046 ) ) ;
#34818 = CARTESIAN_POINT ( 'NONE',  ( 24.96562500061451573, -6.054752690667223547, -1.112240025338166033E-15 ) ) ;
#34819 = EDGE_CURVE ( 'NONE', #24506, #57706, #24851, .T. ) ;
#34820 = AXIS2_PLACEMENT_3D ( 'NONE', #53797, #3192, #65603 ) ;
#34821 = CARTESIAN_POINT ( 'NONE',  ( 18.04687500061451999, 6.054752690667223547, 3.707466751127219781E-16 ) ) ;
#34822 = CARTESIAN_POINT ( 'NONE',  ( 24.06562500061451715, -6.054752690667223547, -1.112240025338166033E-15 ) ) ;
#34823 = CARTESIAN_POINT ( 'NONE',  ( 15.20625000122903181, 0.000000000000000000, 4.999999999999998224 ) ) ;
#34824 = CARTESIAN_POINT ( 'NONE',  ( 8.484601909799253346E-16, 16.96250000000000213, 34.61880215351700230 ) ) ;
#34825 = CARTESIAN_POINT ( 'NONE',  ( 29.46562500061451573, -6.054752690667223547, -1.112240025338166033E-15 ) ) ;
#34826 = CARTESIAN_POINT ( 'NONE',  ( 10.53750000122903252, 6.123233995736764310E-16, -4.999999999999998224 ) ) ;
#34827 = VECTOR ( 'NONE', #19772, 1000.000000000000000 ) ;
#34828 = CARTESIAN_POINT ( 'NONE',  ( 8.025000001229035007, 2.886751345948126879, 4.999999999999999112 ) ) ;
#34829 = CARTESIAN_POINT ( 'NONE',  ( 4.000000000000000000, 19.73749999999999716, -27.69059892324149530 ) ) ;
#34830 = CARTESIAN_POINT ( 'NONE',  ( 26.40000000122902790, 5.773502691896255534, 3.535250795749688894E-16 ) ) ;
#34831 = CARTESIAN_POINT ( 'NONE',  ( -4.000000000000000888, 19.45624999877097139, 32.30940107675850470 ) ) ;
#34832 = CARTESIAN_POINT ( 'NONE',  ( 16.44375000122903074, 5.773502691896255534, 3.535250795749688894E-16 ) ) ;
#34833 = CARTESIAN_POINT ( 'NONE',  ( 9.684375000614517504, -4.541064518000419881, 2.621784821874995952 ) ) ;
#34834 = DIRECTION ( 'NONE',  ( 0.000000000000000000, 0.000000000000000000, 1.000000000000000000 ) ) ;
#34835 = CARTESIAN_POINT ( 'NONE',  ( 18.59062500061451573, -3.027376345333614438, 5.243569643749998122 ) ) ;
#34836 = CARTESIAN_POINT ( 'NONE',  ( 10.58437500061451964, -4.541064518000419881, 2.621784821874995952 ) ) ;
#34837 = CARTESIAN_POINT ( 'NONE',  ( 28.42500000122904069, -5.773502691896255534, -1.060575238724906372E-15 ) ) ;
#34838 = CARTESIAN_POINT ( 'NONE',  ( 20.55937500061451573, -4.541064518000417216, -2.621784821875001281 ) ) ;
#34839 = CARTESIAN_POINT ( 'NONE',  ( 6.909375000614518036, 0.000000000000000000, 5.243569643749999010 ) ) ;
#34840 = CARTESIAN_POINT ( 'NONE',  ( 10.83750000000000036, -2.886751345948237457, -4.999999999999807265 ) ) ;
#34841 = CARTESIAN_POINT ( 'NONE',  ( 8.278125000614515727, -4.541064518000419881, 2.621784821874995952 ) ) ;
#34842 =( BOUNDED_CURVE ( )  B_SPLINE_CURVE ( 2, ( #53511, #30978, #69061, #7355, #41345, #29884, #18421, #40987, #63503 ),
 .UNSPECIFIED., .F., .F. ) 
 B_SPLINE_CURVE_WITH_KNOTS ( ( 3, 2, 2, 2, 3 ),
 ( 0.5760869565217391353, 0.5797101449275362528, 0.5869565217391304879, 0.5942028985507246119, 0.5978260869565217295 ),
 .UNSPECIFIED. ) 
 CURVE ( )  GEOMETRIC_REPRESENTATION_ITEM ( )  RATIONAL_B_SPLINE_CURVE ( ( 0.9330127018922194093, 0.9330127018922194093, 1.000000000000000000, 0.8660254037844387076, 1.000000000000000000, 0.8660254037844387076, 1.000000000000000000, 0.9330127018922194093, 0.9330127018922194093 ) ) 
 REPRESENTATION_ITEM ( '' )  );
#34843 = CARTESIAN_POINT ( 'NONE',  ( 16.60312500061451857, 4.541064518000418104, -2.621784821874998173 ) ) ;
#34844 = ORIENTED_EDGE ( 'NONE', *, *, #62019, .F. ) ;
#34845 = CARTESIAN_POINT ( 'NONE',  ( 5.887500001229034829, -4.330127018922194537, 2.499999999999995559 ) ) ;
#34846 = CARTESIAN_POINT ( 'NONE',  ( 15.17812500061451608, 6.421520780324663323E-16, -5.243569643749999010 ) ) ;
#34847 = CARTESIAN_POINT ( 'NONE',  ( 14.24062500061451608, -3.027376345333610441, -5.243569643749999898 ) ) ;
#34848 = CARTESIAN_POINT ( 'NONE',  ( 24.00937500061451502, 0.000000000000000000, 4.756430356249998326 ) ) ;
#34849 = CARTESIAN_POINT ( 'NONE',  ( 13.35000000000000142, 0.000000000000000000, 4.999999999999998224 ) ) ;
#34850 = CARTESIAN_POINT ( 'NONE',  ( 7.837500001229035007, 6.123233995736764310E-16, -4.999999999999998224 ) ) ;
#34851 = CARTESIAN_POINT ( 'NONE',  ( 5.240625000614516971, -3.027376345333610441, -5.243569643749999898 ) ) ;
#34852 = CARTESIAN_POINT ( 'NONE',  ( 17.92500000122903359, 2.886751345948126879, 4.999999999999999112 ) ) ;
#34853 = CARTESIAN_POINT ( 'NONE',  ( 25.80000000000000071, 4.330127018922192761, -2.499999999999997780 ) ) ;
#34854 = CARTESIAN_POINT ( 'NONE',  ( -4.243569643749999898, 10.37187500061451750, -32.45002607614398471 ) ) ;
#34855 = DIRECTION ( 'NONE',  ( -0.000000000000000000, -1.000000000000000000, -0.000000000000000000 ) ) ;
#34856 = CARTESIAN_POINT ( 'NONE',  ( 2.925000001229034918, 2.886751345948129099, -4.999999999999998224 ) ) ;
#34857 = CARTESIAN_POINT ( 'NONE',  ( 6.600000000000001421, 0.000000000000000000, 4.999999999999998224 ) ) ;
#34858 = CARTESIAN_POINT ( 'NONE',  ( 13.83749999999999858, -2.886751345948130876, 4.999999999999996447 ) ) ;
#34859 = CARTESIAN_POINT ( 'NONE',  ( 18.04687500061451999, 6.054752690667223547, 3.707466751127219781E-16 ) ) ;
#34860 = VECTOR ( 'NONE', #18780, 1000.000000000000000 ) ;
#34861 = CARTESIAN_POINT ( 'NONE',  ( 13.26562500061451644, -6.054752690667223547, -1.112240025338166033E-15 ) ) ;
#34862 = CARTESIAN_POINT ( 'NONE',  ( 10.06875000122903252, 2.886751345948129099, -4.999999999999998224 ) ) ;
#34863 = CARTESIAN_POINT ( 'NONE',  ( 18.97499999999999787, 6.123233995736764310E-16, -4.999999999999998224 ) ) ;
#34864 = CARTESIAN_POINT ( 'NONE',  ( 26.18437500061451573, 4.541064518000418104, 2.621784821874999949 ) ) ;
#34865 = CARTESIAN_POINT ( 'NONE',  ( 17.52187500061451431, 4.119189519843966529, 2.378215178124999607 ) ) ;
#34866 = CARTESIAN_POINT ( 'NONE',  ( 12.47812500061451502, 6.421520780324663323E-16, -5.243569643749999010 ) ) ;
#34867 = CARTESIAN_POINT ( 'NONE',  ( 10.77187500061451786, 3.027376345333613106, -5.243569643749998122 ) ) ;
#34868 = EDGE_LOOP ( 'NONE', ( #59205, #24075, #62735, #72370 ) ) ;
#34869 = CARTESIAN_POINT ( 'NONE',  ( 29.35312500061451502, 0.000000000000000000, 5.243569643749999010 ) ) ;
#34870 = CARTESIAN_POINT ( 'NONE',  ( 20.84062500061451573, -3.027376345333614438, 5.243569643749998122 ) ) ;
#34871 = CARTESIAN_POINT ( 'NONE',  ( 29.46562500061451573, -6.054752690667223547, -1.112240025338166033E-15 ) ) ;
#34872 = CARTESIAN_POINT ( 'NONE',  ( 1.626862140677534273E-15, 15.27500000122903501, -26.00000000000000355 ) ) ;
#34873 = CARTESIAN_POINT ( 'NONE',  ( 8.962500000000002132, -5.773502691896255534, -1.060575238724906372E-15 ) ) ;
#34874 = CARTESIAN_POINT ( 'NONE',  ( 19.76250000122903216, 0.000000000000000000, 4.999999999999998224 ) ) ;
#34875 = CARTESIAN_POINT ( 'NONE',  ( -2.000000000000000000, 18.68750000122903288, -33.46410161513775705 ) ) ;
#34876 = CARTESIAN_POINT ( 'NONE',  ( 11.22187500061451537, 4.119189519843966529, 2.378215178124999607 ) ) ;
#34877 = EDGE_LOOP ( 'NONE', ( #12003, #24739, #44270, #17374 ) ) ;
#34878 = CARTESIAN_POINT ( 'NONE',  ( 18.41250000000000142, -5.773502691896255534, -1.060575238724906372E-15 ) ) ;
#34879 = CARTESIAN_POINT ( 'NONE',  ( 20.77500000000000213, 6.123233995736764310E-16, -4.999999999999998224 ) ) ;
#34880 = CARTESIAN_POINT ( 'NONE',  ( 19.54687500061451644, -3.027376345333614438, 5.243569643749998122 ) ) ;
#34881 = CARTESIAN_POINT ( 'NONE',  ( 25.75312500061451715, 0.000000000000000000, 5.243569643749999010 ) ) ;
#34882 = ORIENTED_EDGE ( 'NONE', *, *, #34218, .F. ) ;
#34883 = EDGE_CURVE ( 'NONE', #58840, #63177, #53671, .T. ) ;
#34884 = CARTESIAN_POINT ( 'NONE',  ( -1.071796769724483234, 16.87009619066137134, 25.99999999999999645 ) ) ;
#34885 = CARTESIAN_POINT ( 'NONE',  ( 8.840625000614515727, -3.027376345333610441, -5.243569643749999898 ) ) ;
#34886 = DIRECTION ( 'NONE',  ( -1.000000000000000000, -0.000000000000000000, -0.000000000000000000 ) ) ;
#34887 = CARTESIAN_POINT ( 'NONE',  ( 13.95000000000000107, -4.330127018922190985, -2.500000000000001332 ) ) ;
#34888 = CARTESIAN_POINT ( 'NONE',  ( 4.243569643749999898, 18.22812500061451502, 30.00000000000000000 ) ) ;
#34889 = CARTESIAN_POINT ( 'NONE',  ( 3.046875000614519990, -3.027376345333610441, -5.243569643749999898 ) ) ;
#34890 = CARTESIAN_POINT ( 'NONE',  ( 10.16249999999999964, 2.886751345948126879, 4.999999999999999112 ) ) ;
#34891 = CARTESIAN_POINT ( 'NONE',  ( -1.878215178124999163, 14.14062499938548356, 26.74683588394047007 ) ) ;
#34892 = CARTESIAN_POINT ( 'NONE',  ( 25.92187500061451999, -6.054752690667223547, -1.112240025338166033E-15 ) ) ;
#34893 = ORIENTED_EDGE ( 'NONE', *, *, #47275, .T. ) ;
#34894 = CARTESIAN_POINT ( 'NONE',  ( 24.89062500061451644, -3.027376345333614438, 5.243569643749998122 ) ) ;
#34895 = CARTESIAN_POINT ( 'NONE',  ( 23.10937500061451644, 0.000000000000000000, 5.243569643749999010 ) ) ;
#34896 = CARTESIAN_POINT ( 'NONE',  ( -3.000416591977282496E-16, 17.44062500061459176, -34.90005215228797653 ) ) ;
#34897 = CARTESIAN_POINT ( 'NONE',  ( 10.57500000000000107, 4.330127018922191873, 2.499999999999999556 ) ) ;
#34898 = ADVANCED_FACE ( 'NONE', ( #25594 ), #37408, .F. ) ;
#34899 = CARTESIAN_POINT ( 'NONE',  ( 8.615625000614517859, 3.027376345333611329, 5.243569643749999010 ) ) ;
#34900 = CARTESIAN_POINT ( 'NONE',  ( 29.22187500061451715, 2.746126346562645981, -4.756430356249997438 ) ) ;
#34901 = CARTESIAN_POINT ( 'NONE',  ( 28.11562500061451431, -6.054752690667223547, -1.112240025338166033E-15 ) ) ;
#34902 = CARTESIAN_POINT ( 'NONE',  ( 23.57812500061451289, -4.541064518000419881, 2.621784821874995952 ) ) ;
#34903 = CARTESIAN_POINT ( 'NONE',  ( 27.79687500061451289, 4.119189519843966529, -2.378215178124998275 ) ) ;
#34904 = CARTESIAN_POINT ( 'NONE',  ( 12.64687500061451608, 5.492252693125287522, 3.363034840372157021E-16 ) ) ;
#34905 = CARTESIAN_POINT ( 'NONE',  ( 19.62187500061451573, -6.054752690667223547, -1.112240025338166033E-15 ) ) ;
#34906 = CARTESIAN_POINT ( 'NONE',  ( -4.243569643749999898, 11.72187500061451892, 27.54997392385601529 ) ) ;
#34907 = CARTESIAN_POINT ( 'NONE',  ( 19.28437500061451360, 6.421520780324663323E-16, -5.243569643749999010 ) ) ;
#34908 = CARTESIAN_POINT ( 'NONE',  ( 26.67187500061451644, 3.027376345333611329, 5.243569643749999010 ) ) ;
#34909 = CARTESIAN_POINT ( 'NONE',  ( 4.243569643749999010, 16.07187500061451857, 27.54997392385601174 ) ) ;
#34910 = CARTESIAN_POINT ( 'NONE',  ( 7.903125000614515727, -4.541064518000417216, -2.621784821875001281 ) ) ;
#34911 = EDGE_CURVE ( 'NONE', #68252, #16431, #57037, .T. ) ;
#34912 = CARTESIAN_POINT ( 'NONE',  ( 4.921875000614518214, 3.027376345333613106, -5.243569643749998122 ) ) ;
#34913 = CARTESIAN_POINT ( 'NONE',  ( 4.000000000000000000, 15.68750000000000000, -27.69059892324149885 ) ) ;
#34914 = AXIS2_PLACEMENT_3D ( 'NONE', #63991, #52915, #51830 ) ;
#34915 = CARTESIAN_POINT ( 'NONE',  ( 5.503125000614516260, 0.000000000000000000, 5.243569643749999010 ) ) ;
#34916 = CARTESIAN_POINT ( 'NONE',  ( 9.234375000614518214, -4.541064518000419881, 2.621784821874995952 ) ) ;
#34917 = CARTESIAN_POINT ( 'NONE',  ( 16.87500000122903288, 2.886751345948129099, -4.999999999999998224 ) ) ;
#34918 = CARTESIAN_POINT ( 'NONE',  ( 5.521875000614517859, 3.027376345333611329, 5.243569643749999010 ) ) ;
#34919 = CARTESIAN_POINT ( 'NONE',  ( 6.515625000614516438, -6.054752690667223547, -1.112240025338166033E-15 ) ) ;
#34920 = CARTESIAN_POINT ( 'NONE',  ( 5.540625000614515905, -3.027376345333614438, 5.243569643749998122 ) ) ;
#34921 = CARTESIAN_POINT ( 'NONE',  ( 23.04375000122903216, -2.886751345948125991, -5.000000000000000000 ) ) ;
#34922 = CARTESIAN_POINT ( 'NONE',  ( 16.50937500061451502, -4.541064518000417216, -2.621784821875001281 ) ) ;
#34923 = CARTESIAN_POINT ( 'NONE',  ( -3.305247878049081707E-15, 5.000000000000034639, -34.00000000000004263 ) ) ;
#34924 = EDGE_LOOP ( 'NONE', ( #3819, #1367, #68499, #17300 ) ) ;
#34925 = CARTESIAN_POINT ( 'NONE',  ( 24.02812500061451573, -4.541064518000419881, 2.621784821874995952 ) ) ;
#34926 = CARTESIAN_POINT ( 'NONE',  ( 8.953125000614518214, 4.541064518000418104, -2.621784821874998173 ) ) ;
#34927 = CARTESIAN_POINT ( 'NONE',  ( 27.00937500061451857, 4.541064518000418104, -2.621784821874998173 ) ) ;
#34928 = CARTESIAN_POINT ( 'NONE',  ( 9.853125000614516793, 4.541064518000418104, -2.621784821874998173 ) ) ;
#34929 = CARTESIAN_POINT ( 'NONE',  ( -4.243569643749999898, 9.921875000614516438, -32.45002607614398471 ) ) ;
#34930 = EDGE_CURVE ( 'NONE', #23775, #45011, #51872, .T. ) ;
#34931 = CARTESIAN_POINT ( 'NONE',  ( 10.98750000122903536, 6.123233995736764310E-16, -4.999999999999998224 ) ) ;
#34932 = CARTESIAN_POINT ( 'NONE',  ( 26.31562500061451715, -6.054752690667223547, -1.112240025338166033E-15 ) ) ;
#34933 = CARTESIAN_POINT ( 'NONE',  ( 2.121784821875001281, 13.20312500061451821, -26.32496088578401938 ) ) ;
#34934 = CARTESIAN_POINT ( 'NONE',  ( 12.33750000122903145, 6.123233995736764310E-16, -4.999999999999998224 ) ) ;
#34935 = CARTESIAN_POINT ( 'NONE',  ( 21.10312500061451502, 4.541064518000418104, -2.621784821874998173 ) ) ;
#34936 = CARTESIAN_POINT ( 'NONE',  ( 10.16249999999999964, 2.886751345948126879, 4.999999999999999112 ) ) ;
#34937 = CARTESIAN_POINT ( 'NONE',  ( 20.09062500061451573, -3.027376345333610441, -5.243569643749999898 ) ) ;
#34938 = CARTESIAN_POINT ( 'NONE',  ( 4.959375000614516971, 4.541064518000418104, -2.621784821874998173 ) ) ;
#34939 = CARTESIAN_POINT ( 'NONE',  ( 21.26249999999999574, 2.886751345948129099, -4.999999999999998224 ) ) ;
#34940 = CARTESIAN_POINT ( 'NONE',  ( 7.537500001229033408, 4.330127018922191873, 2.499999999999999556 ) ) ;
#34941 = CARTESIAN_POINT ( 'NONE',  ( 15.52500000122903323, 2.886751345948129099, -4.999999999999998224 ) ) ;
#34942 = CARTESIAN_POINT ( 'NONE',  ( 13.52812500061451750, 4.541064518000418104, 2.621784821874999949 ) ) ;
#34943 = CARTESIAN_POINT ( 'NONE',  ( 14.80312500061451608, 4.541064518000418104, -2.621784821874998173 ) ) ;
#34944 = CARTESIAN_POINT ( 'NONE',  ( 25.23750000122903359, -4.330127018922194537, 2.499999999999995559 ) ) ;
#34945 = CARTESIAN_POINT ( 'NONE',  ( 20.40000000000000213, 4.330127018922192761, -2.499999999999997780 ) ) ;
#34946 = CARTESIAN_POINT ( 'NONE',  ( 22.95937500061451431, 4.541064518000418104, -2.621784821874998173 ) ) ;
#34947 = CARTESIAN_POINT ( 'NONE',  ( 22.33125000122903003, 4.330127018922191873, 2.499999999999999556 ) ) ;
#34948 = CARTESIAN_POINT ( 'NONE',  ( 11.13750000122903216, 4.330127018922191873, 2.499999999999999556 ) ) ;
#34949 = CARTESIAN_POINT ( 'NONE',  ( 9.609375000614518214, 0.000000000000000000, 5.243569643749999010 ) ) ;
#34950 = CARTESIAN_POINT ( 'NONE',  ( 25.09687500061451715, -3.027376345333610441, -5.243569643749999898 ) ) ;
#34951 = CARTESIAN_POINT ( 'NONE',  ( 3.196875000614516793, 6.054752690667223547, 3.707466751127219781E-16 ) ) ;
#34952 = CARTESIAN_POINT ( 'NONE',  ( 20.39062500061451644, -3.027376345333614438, 5.243569643749998122 ) ) ;
#34953 = CARTESIAN_POINT ( 'NONE',  ( 26.74687500061451573, -3.027376345333614438, 5.243569643749998122 ) ) ;
#34954 = CARTESIAN_POINT ( 'NONE',  ( 1.878215178124997609, 16.27812499938548285, 33.25316411605952993 ) ) ;
#34955 = CARTESIAN_POINT ( 'NONE',  ( 19.25625000122903430, 0.000000000000000000, 4.999999999999998224 ) ) ;
#34956 = VECTOR ( 'NONE', #70940, 1000.000000000000000 ) ;
#34957 = CARTESIAN_POINT ( 'NONE',  ( 7.584375000614516082, 6.421520780324663323E-16, -5.243569643749999010 ) ) ;
#34958 = CARTESIAN_POINT ( 'NONE',  ( 18.66562500061451146, -6.054752690667223547, -1.112240025338166033E-15 ) ) ;
#34959 = EDGE_LOOP ( 'NONE', ( #72249, #31278, #12968, #39766 ) ) ;
#34960 = CARTESIAN_POINT ( 'NONE',  ( 4.550098044277414822, 3.654122216399865675, 4.158013951629233595 ) ) ;
#34961 = CARTESIAN_POINT ( 'NONE',  ( 28.00312500061451715, 0.000000000000000000, 5.243569643749999010 ) ) ;
#34962 = CARTESIAN_POINT ( 'NONE',  ( 3.421875000614516882, -6.054752690667223547, -1.112240025338166033E-15 ) ) ;
#34963 = CARTESIAN_POINT ( 'NONE',  ( 22.80000000122903359, 5.773502691896255534, 3.535250795749688401E-16 ) ) ;
#34964 = CARTESIAN_POINT ( 'NONE',  ( 27.58125000122903359, 6.123233995736764310E-16, -4.999999999999998224 ) ) ;
#34965 = CARTESIAN_POINT ( 'NONE',  ( 17.21249999999999858, 2.886751345948129099, -4.999999999999998224 ) ) ;
#34966 = ORIENTED_EDGE ( 'NONE', *, *, #41247, .F. ) ;
#34967 = CARTESIAN_POINT ( 'NONE',  ( 24.82499999999999929, 6.123233995736764310E-16, -4.999999999999998224 ) ) ;
#34968 = CARTESIAN_POINT ( 'NONE',  ( 27.08437500061451786, 4.541064518000418104, 2.621784821874999949 ) ) ;
#34969 = VERTEX_POINT ( 'NONE', #42586 ) ;
#34970 = CARTESIAN_POINT ( 'NONE',  ( 16.34062500061451573, -3.027376345333614438, 5.243569643749998122 ) ) ;
#34971 = CARTESIAN_POINT ( 'NONE',  ( 7.078125000614516438, 6.421520780324663323E-16, -5.243569643749999010 ) ) ;
#34972 = CARTESIAN_POINT ( 'NONE',  ( 18.49687500061451573, 0.000000000000000000, 4.756430356249998326 ) ) ;
#34973 = CARTESIAN_POINT ( 'NONE',  ( 29.76562500061451644, 3.027376345333611329, 5.243569643749999010 ) ) ;
#34974 = CARTESIAN_POINT ( 'NONE',  ( 16.12500000122903288, 2.886751345948126879, 4.999999999999999112 ) ) ;
#34975 = CARTESIAN_POINT ( 'NONE',  ( 20.92500000000000071, 4.330127018922191873, 2.499999999999999556 ) ) ;
#34976 = CARTESIAN_POINT ( 'NONE',  ( 29.84999999999999787, 4.330127018922192761, -2.499999999999997780 ) ) ;
#34977 = CARTESIAN_POINT ( 'NONE',  ( 4.471875000614518925, 3.027376345333613106, -5.243569643749998122 ) ) ;
#34978 = CARTESIAN_POINT ( 'NONE',  ( 9.459375000614517859, 4.541064518000418104, -2.621784821874998173 ) ) ;
#34979 = CARTESIAN_POINT ( 'NONE',  ( 21.64687500061451786, 6.054752690667223547, 3.707466751127219781E-16 ) ) ;
#34980 = EDGE_CURVE ( 'NONE', #55912, #39861, #65112, .T. ) ;
#34981 = CYLINDRICAL_SURFACE ( 'NONE', #4159, 4.999999999999998224 ) ;
#34982 = ORIENTED_EDGE ( 'NONE', *, *, #13710, .T. ) ;
#34983 = CARTESIAN_POINT ( 'NONE',  ( 3.121875000614518836, 3.027376345333613106, -5.243569643749998122 ) ) ;
#34984 = CARTESIAN_POINT ( 'NONE',  ( 5.025000000000002132, 6.123233995736764310E-16, -4.999999999999998224 ) ) ;
#34985 = CARTESIAN_POINT ( 'NONE',  ( 7.659375000614518036, 4.541064518000418104, -2.621784821874998173 ) ) ;
#34986 = CARTESIAN_POINT ( 'NONE',  ( 19.04999999999999716, 4.330127018922192761, -2.499999999999997780 ) ) ;
#34987 = CARTESIAN_POINT ( 'NONE',  ( 15.14062500061451644, -3.027376345333610441, -5.243569643749999898 ) ) ;
#34988 = CARTESIAN_POINT ( 'NONE',  ( -4.000000000000000000, 19.92499999999999716, 30.00000000000000000 ) ) ;
#34989 = CARTESIAN_POINT ( 'NONE',  ( 24.90000000122903501, -2.886751345948142422, -4.999999999999970690 ) ) ;
#34990 = CARTESIAN_POINT ( 'NONE',  ( 20.29687500061451644, 5.492252693125287522, 3.363034840372157021E-16 ) ) ;
#34991 = CARTESIAN_POINT ( 'NONE',  ( 10.94062500061451537, -3.027376345333614438, 5.243569643749998122 ) ) ;
#34992 = CARTESIAN_POINT ( 'NONE',  ( 27.00937500061451857, 4.541064518000418104, -2.621784821874998173 ) ) ;
#34993 = CARTESIAN_POINT ( 'NONE',  ( 9.001249775931846008E-16, 19.07187500061451502, 34.90005215228797653 ) ) ;
#34994 = CARTESIAN_POINT ( 'NONE',  ( 25.43437500061451573, -4.541064518000419881, 2.621784821874995952 ) ) ;
#34995 = CARTESIAN_POINT ( 'NONE',  ( 7.950000000000001954, 0.000000000000000000, 4.999999999999998224 ) ) ;
#34996 = CARTESIAN_POINT ( 'NONE',  ( -2.828200636599751609E-16, 12.35000000122903430, 25.38119784648299770 ) ) ;
#34997 = CARTESIAN_POINT ( 'NONE',  ( 13.82812500061451466, 6.421520780324663323E-16, -5.243569643749999010 ) ) ;
#34998 = CARTESIAN_POINT ( 'NONE',  ( 7.500000001229034652, 5.773502691896255534, 3.535250795749688894E-16 ) ) ;
#34999 = CARTESIAN_POINT ( 'NONE',  ( 18.60937500061451644, 0.000000000000000000, 5.243569643749999010 ) ) ;
#35000 = CARTESIAN_POINT ( 'NONE',  ( 12.68437500061451573, 4.541064518000418104, 2.621784821874999949 ) ) ;
#35001 = CARTESIAN_POINT ( 'NONE',  ( -3.779748323423378853, 3.276532024208882010, -28.66603734123481573 ) ) ;
#35002 = ORIENTED_EDGE ( 'NONE', *, *, #68503, .F. ) ;
#35003 = CARTESIAN_POINT ( 'NONE',  ( 13.22812500061451502, -4.541064518000419881, 2.621784821874995952 ) ) ;
#35004 = CARTESIAN_POINT ( 'NONE',  ( 26.88750000122903216, 4.330127018922191873, 2.499999999999999556 ) ) ;
#35005 = CARTESIAN_POINT ( 'NONE',  ( 13.73437500061451821, -4.541064518000419881, 2.621784821874995952 ) ) ;
#35006 = CARTESIAN_POINT ( 'NONE',  ( 15.36562500061451608, 3.027376345333611329, 5.243569643749999010 ) ) ;
#35007 = CARTESIAN_POINT ( 'NONE',  ( -5.000000000000000000, 0.000000000000000000, 50.00000000000000000 ) ) ;
#35008 = CARTESIAN_POINT ( 'NONE',  ( 24.42187500061451999, 3.027376345333611329, 5.243569643749999010 ) ) ;
#35009 = CYLINDRICAL_SURFACE ( 'NONE', #71474, 4.000000000000000000 ) ;
#35010 = CARTESIAN_POINT ( 'NONE',  ( 12.78750000122903430, 6.123233995736764310E-16, -4.999999999999998224 ) ) ;
#35011 = CARTESIAN_POINT ( 'NONE',  ( 8.409375000614518925, -4.119189519843965641, -2.378215178125001383 ) ) ;
#35012 = CARTESIAN_POINT ( 'NONE',  ( 1.138803498474273873E-14, 15.48124999877096641, 34.00000000000000000 ) ) ;
#35013 = CARTESIAN_POINT ( 'NONE',  ( 2.121784821874999061, 17.90937500061451715, -33.67503911421598417 ) ) ;
#35014 = CARTESIAN_POINT ( 'NONE',  ( 18.45937500061451431, 4.541064518000418104, -2.621784821874998173 ) ) ;
#35015 = CARTESIAN_POINT ( 'NONE',  ( 19.01250000122903216, -4.330127018922190985, -2.500000000000001332 ) ) ;
#35016 = CARTESIAN_POINT ( 'NONE',  ( 13.62187500061451750, 3.027376345333611329, 5.243569643749999010 ) ) ;
#35017 = CARTESIAN_POINT ( 'NONE',  ( -4.243569643749999898, 9.959375000614517859, 30.00000000000000000 ) ) ;
#35018 = CARTESIAN_POINT ( 'NONE',  ( 18.78750000122903430, 4.330127018922191873, 2.499999999999999556 ) ) ;
#35019 = VECTOR ( 'NONE', #61663, 1000.000000000000000 ) ;
#35020 = CARTESIAN_POINT ( 'NONE',  ( 16.15312500061451573, 4.541064518000418104, -2.621784821874998173 ) ) ;
#35021 = ORIENTED_EDGE ( 'NONE', *, *, #33319, .F. ) ;
#35022 = ORIENTED_EDGE ( 'NONE', *, *, #5433, .T. ) ;
#35023 = CARTESIAN_POINT ( 'NONE',  ( 19.04999999999999716, 4.330127018922192761, -2.499999999999997780 ) ) ;
#35024 = CARTESIAN_POINT ( 'NONE',  ( 1.071796769724491893, 14.20759618943233527, 34.00000000000000000 ) ) ;
#35025 = CARTESIAN_POINT ( 'NONE',  ( 3.890625000614517326, -3.027376345333610441, -5.243569643749999898 ) ) ;
#35026 = CARTESIAN_POINT ( 'NONE',  ( 14.92500000122903181, -5.773502691896255534, -1.060575238724906372E-15 ) ) ;
#35027 = CARTESIAN_POINT ( 'NONE',  ( 26.25937500061451857, 0.000000000000000000, 5.243569643749999010 ) ) ;
#35028 = CARTESIAN_POINT ( 'NONE',  ( 20.69062500061451715, 6.054752690667223547, 3.707466751127219781E-16 ) ) ;
#35029 = CARTESIAN_POINT ( 'NONE',  ( 21.89062500061451289, -3.027376345333610441, -5.243569643749999898 ) ) ;
#35030 = CARTESIAN_POINT ( 'NONE',  ( 4.040625000614517681, 6.054752690667223547, 3.707466751127219781E-16 ) ) ;
#35031 = CARTESIAN_POINT ( 'NONE',  ( 26.69999999999999929, 4.330127018922192761, -2.499999999999997780 ) ) ;
#35032 = CARTESIAN_POINT ( 'NONE',  ( 27.99375000122903145, -2.886751345948126435, -5.000000000000000000 ) ) ;
#35033 = CARTESIAN_POINT ( 'NONE',  ( 9.084375000614517859, 4.119189519843966529, 2.378215178124999607 ) ) ;
#35034 = CARTESIAN_POINT ( 'NONE',  ( 1.071796769724488785, 17.80759618943233491, 34.00000000000000000 ) ) ;
#35035 = CARTESIAN_POINT ( 'NONE',  ( 24.14999999999999858, 0.000000000000000000, 4.999999999999998224 ) ) ;
#35036 = CARTESIAN_POINT ( 'NONE',  ( -3.000416591977282496E-16, 17.04687500061451644, -34.90005215228797653 ) ) ;
#35037 = CARTESIAN_POINT ( 'NONE',  ( 6.075000001229034829, 2.886751345948129099, -4.999999999999998224 ) ) ;
#35038 = CARTESIAN_POINT ( 'NONE',  ( 5.850000000000001421, -4.330127018922190985, -2.500000000000001332 ) ) ;
#35039 = EDGE_CURVE ( 'NONE', #3790, #20937, #4214, .T. ) ;
#35040 = CARTESIAN_POINT ( 'NONE',  ( 2.962500001229034119, 4.330127018922192761, -2.499999999999997780 ) ) ;
#35041 = CARTESIAN_POINT ( 'NONE',  ( 9.009375000614518569, 4.541064518000418104, -2.621784821874998173 ) ) ;
#35042 = CARTESIAN_POINT ( 'NONE',  ( 19.35000000122903430, -2.886751345948163738, 4.999999999999939604 ) ) ;
#35043 = CARTESIAN_POINT ( 'NONE',  ( 27.63750000122903216, 6.123233995736764310E-16, -4.999999999999998224 ) ) ;
#35044 = CARTESIAN_POINT ( 'NONE',  ( -5.999929701724457054, 8.000052723701786661, -30.20526279067533792 ) ) ;
#35045 = CARTESIAN_POINT ( 'NONE',  ( 30.00000000000000000, 0.000000000000000000, 0.000000000000000000 ) ) ;
#35046 = CARTESIAN_POINT ( 'NONE',  ( 8.784375000614518925, -4.541064518000419881, 2.621784821874995952 ) ) ;
#35047 = CARTESIAN_POINT ( 'NONE',  ( 11.40937500061451892, 0.000000000000000000, 5.243569643749999010 ) ) ;
#35048 = CARTESIAN_POINT ( 'NONE',  ( 7.350000000000002309, 4.330127018922192761, -2.499999999999997780 ) ) ;
#35049 = CARTESIAN_POINT ( 'NONE',  ( 4.243569643749999898, 14.14062500061459460, 32.45002607614398471 ) ) ;
#35050 = CARTESIAN_POINT ( 'NONE',  ( 22.13437500061451502, 4.541064518000418104, 2.621784821874999949 ) ) ;
#35051 = CARTESIAN_POINT ( 'NONE',  ( 22.85625000122903216, 0.000000000000000000, 4.999999999999998224 ) ) ;
#35052 =( BOUNDED_CURVE ( )  B_SPLINE_CURVE ( 2, ( #47687, #70591, #59492, #31061, #2625, #54342, #19966 ),
 .UNSPECIFIED., .F., .F. ) 
 B_SPLINE_CURVE_WITH_KNOTS ( ( 3, 2, 2, 3 ),
 ( 0.9200000000000001510, 0.9233333333333334503, 0.9266666666666667496, 0.9300000000000001599 ),
 .UNSPECIFIED. ) 
 CURVE ( )  GEOMETRIC_REPRESENTATION_ITEM ( )  RATIONAL_B_SPLINE_CURVE ( ( 0.9999999999999955591, 0.8660254037844431485, 1.000000000000000000, 0.8660254037844387076, 1.000000000000000000, 0.8660254037844342667, 1.000000000000004441 ) ) 
 REPRESENTATION_ITEM ( '' )  );
#35053 = CARTESIAN_POINT ( 'NONE',  ( 6.450000000000001066, 4.330127018922192761, -2.499999999999997780 ) ) ;
#35054 = CARTESIAN_POINT ( 'NONE',  ( 26.28750000122903430, 6.123233995736764310E-16, -4.999999999999998224 ) ) ;
#35055 = CARTESIAN_POINT ( 'NONE',  ( 16.62187500061451573, 4.119189519843966529, 2.378215178124999607 ) ) ;
#35056 = CARTESIAN_POINT ( 'NONE',  ( 21.62812500061451360, 4.541064518000418104, 2.621784821874999949 ) ) ;
#35057 = CARTESIAN_POINT ( 'NONE',  ( 13.04062500061451502, 6.054752690667223547, 3.707466751127219781E-16 ) ) ;
#35058 = CARTESIAN_POINT ( 'NONE',  ( 27.08437500061451431, -2.746126346562646425, 4.756430356249996549 ) ) ;
#35059 = CARTESIAN_POINT ( 'NONE',  ( 11.67187500061451821, 3.027376345333613106, -5.243569643749998122 ) ) ;
#35060 = CARTESIAN_POINT ( 'NONE',  ( 28.94999999999999929, 4.330127018922192761, -2.499999999999997780 ) ) ;
#35061 = CARTESIAN_POINT ( 'NONE',  ( 22.50000000122903288, -2.886751345948129988, 4.999999999999997335 ) ) ;
#35062 = DIRECTION ( 'NONE',  ( 0.000000000000000000, 0.000000000000000000, -1.000000000000000000 ) ) ;
#35063 = CARTESIAN_POINT ( 'NONE',  ( 10.69687500061451679, -3.027376345333610441, -5.243569643749999898 ) ) ;
#35064 = CARTESIAN_POINT ( 'NONE',  ( 27.98437500061451289, 4.541064518000418104, 2.621784821874999949 ) ) ;
#35065 = EDGE_CURVE ( 'NONE', #9585, #47310, #58983, .T. ) ;
#35066 = CARTESIAN_POINT ( 'NONE',  ( 21.91875000122903216, 2.886751345948154857, 4.999999999999951150 ) ) ;
#35067 = CARTESIAN_POINT ( 'NONE',  ( -3.999999999999997335, 12.95000000122903216, -27.69059892324149530 ) ) ;
#35068 = CARTESIAN_POINT ( 'NONE',  ( 22.73437500061451644, -4.541064518000419881, 2.621784821874995952 ) ) ;
#35069 = CARTESIAN_POINT ( 'NONE',  ( 13.05937500061451750, 4.541064518000418104, -2.621784821874998173 ) ) ;
#35070 = CARTESIAN_POINT ( 'NONE',  ( -1.878215178125001827, 17.55312499938548498, 33.25316411605952283 ) ) ;
#35071 = CARTESIAN_POINT ( 'NONE',  ( 26.02499999999999858, -4.330127018922194537, 2.499999999999995559 ) ) ;
#35072 = CARTESIAN_POINT ( 'NONE',  ( -3.756430356250000102, 20.51562499938548356, 30.00000000000000000 ) ) ;
#35073 = CARTESIAN_POINT ( 'NONE',  ( 27.72187500061451715, -5.492252693125287522, -1.008910452111647106E-15 ) ) ;
#35074 = CARTESIAN_POINT ( 'NONE',  ( 16.45312500061451289, -4.541064518000417216, -2.621784821875001281 ) ) ;
#35075 = CARTESIAN_POINT ( 'NONE',  ( 7.612500000000000711, -5.773502691896255534, -1.060575238724906372E-15 ) ) ;
#35076 = CARTESIAN_POINT ( 'NONE',  ( 12.11250000122903181, 0.000000000000000000, 4.999999999999998224 ) ) ;
#35077 = CARTESIAN_POINT ( 'NONE',  ( 15.86250000000000249, 2.886751345948129099, -4.999999999999998224 ) ) ;
#35078 = CARTESIAN_POINT ( 'NONE',  ( -4.243569643749997233, 9.940625000614515372, 32.45002607614398471 ) ) ;
#35079 = CARTESIAN_POINT ( 'NONE',  ( 0.000000000000000000, 20.00000000000000000, 26.00000000000000000 ) ) ;
#35080 = CARTESIAN_POINT ( 'NONE',  ( 24.15937500061451715, -4.541064518000417216, -2.621784821875001281 ) ) ;
#35081 = ORIENTED_EDGE ( 'NONE', *, *, #63436, .F. ) ;
#35082 = CARTESIAN_POINT ( 'NONE',  ( 21.25312500061451715, 0.000000000000000000, 5.243569643749999010 ) ) ;
#35083 = CARTESIAN_POINT ( 'NONE',  ( 20.52187500061451786, -6.054752690667223547, -1.112240025338166033E-15 ) ) ;
#35084 = CARTESIAN_POINT ( 'NONE',  ( 3.412500000000002309, 2.886751345948126879, 4.999999999999999112 ) ) ;
#35085 = CARTESIAN_POINT ( 'NONE',  ( 7.753125000614518036, 0.000000000000000000, 5.243569643749999010 ) ) ;
#35086 = CARTESIAN_POINT ( 'NONE',  ( 22.26562500061451644, -6.054752690667223547, -1.112240025338166033E-15 ) ) ;
#35087 = CARTESIAN_POINT ( 'NONE',  ( 12.94687500061451857, -3.027376345333610441, -5.243569643749999898 ) ) ;
#35088 = CARTESIAN_POINT ( 'NONE',  ( 17.78437500061451715, -4.541064518000419881, 2.621784821874995952 ) ) ;
#35089 = CARTESIAN_POINT ( 'NONE',  ( -4.243569643749999898, 16.65312500061451573, 30.00000000000000000 ) ) ;
#35090 = EDGE_CURVE ( 'NONE', #41056, #54204, #1830, .T. ) ;
#35091 = CARTESIAN_POINT ( 'NONE',  ( 18.11250000122903359, -4.330127018922190985, -2.500000000000001332 ) ) ;
#35092 = CARTESIAN_POINT ( 'NONE',  ( 15.75937500061451857, 4.119189519843966529, -2.378215178124998275 ) ) ;
#35093 = CARTESIAN_POINT ( 'NONE',  ( 8.690625000614515372, -3.027376345333614438, 5.243569643749998122 ) ) ;
#35094 = CARTESIAN_POINT ( 'NONE',  ( 4.434375000614519280, 6.421520780324663323E-16, -5.243569643749999010 ) ) ;
#35095 = CARTESIAN_POINT ( 'NONE',  ( 5.484375000614518214, 4.541064518000418104, 2.621784821874999949 ) ) ;
#35096 = CARTESIAN_POINT ( 'NONE',  ( 25.02187500061451431, -6.054752690667223547, -1.112240025338166033E-15 ) ) ;
#35097 = CARTESIAN_POINT ( 'NONE',  ( 16.82812500061451644, -4.541064518000419881, 2.621784821874995952 ) ) ;
#35098 = CARTESIAN_POINT ( 'NONE',  ( 26.66250000122903430, -4.330127018922190985, -2.500000000000001332 ) ) ;
#35099 = CARTESIAN_POINT ( 'NONE',  ( 26.16562500061451502, 3.027376345333611329, 5.243569643749999010 ) ) ;
#35100 = CARTESIAN_POINT ( 'NONE',  ( 22.20937500061451431, 0.000000000000000000, 5.243569643749999010 ) ) ;
#35101 = CARTESIAN_POINT ( 'NONE',  ( 17.84062500061451573, -3.027376345333610441, -5.243569643749999898 ) ) ;
#35102 = CARTESIAN_POINT ( 'NONE',  ( 4.243569643749999010, 17.42187500061451999, 27.54997392385601174 ) ) ;
#35103 = CARTESIAN_POINT ( 'NONE',  ( 23.20312500061451644, -4.541064518000417216, -2.621784821875001281 ) ) ;
#35104 = CARTESIAN_POINT ( 'NONE',  ( 29.23125000122903216, -4.330127018922194537, 2.499999999999995559 ) ) ;
#35105 = ORIENTED_EDGE ( 'NONE', *, *, #43096, .T. ) ;
#35106 = CARTESIAN_POINT ( 'NONE',  ( 25.91250000000000142, 2.886751345948126879, 4.999999999999999112 ) ) ;
#35107 = CARTESIAN_POINT ( 'NONE',  ( 1.999999999999998668, 13.55000000000000071, -33.46410161513775705 ) ) ;
#35108 = CARTESIAN_POINT ( 'NONE',  ( 1.878215178124997609, 19.87812499938548072, 33.25316411605952993 ) ) ;
#35109 = CARTESIAN_POINT ( 'NONE',  ( 29.24062500061451431, 6.054752690667223547, 3.707466751127219781E-16 ) ) ;
#35110 = CARTESIAN_POINT ( 'NONE',  ( 10.71562500061451928, 3.027376345333613106, -5.243569643749998122 ) ) ;
#35111 = CARTESIAN_POINT ( 'NONE',  ( 22.72500000122903430, 2.886751345948129099, -4.999999999999998224 ) ) ;
#35112 = AXIS2_PLACEMENT_3D ( 'NONE', #13929, #40937, #52368 ) ;
#35113 = CARTESIAN_POINT ( 'NONE',  ( 27.51562500061451644, 3.027376345333611329, 5.243569643749999010 ) ) ;
#35114 = CARTESIAN_POINT ( 'NONE',  ( 25.91250000000000142, 2.886751345948126879, 4.999999999999999112 ) ) ;
#35115 = CARTESIAN_POINT ( 'NONE',  ( 2.000000000000001332, 16.66250000122903430, -26.53589838486224650 ) ) ;
#35116 = CARTESIAN_POINT ( 'NONE',  ( -1.999999999999997113, 12.53750000122903430, 33.46410161513775705 ) ) ;
#35117 = CARTESIAN_POINT ( 'NONE',  ( 9.665625000614515017, -6.054752690667223547, -1.112240025338166033E-15 ) ) ;
#35118 = ORIENTED_EDGE ( 'NONE', *, *, #66833, .F. ) ;
#35119 = CARTESIAN_POINT ( 'NONE',  ( 25.67812500061451431, 4.541064518000418104, 2.621784821874999949 ) ) ;
#35120 = CARTESIAN_POINT ( 'NONE',  ( 8.353125000614518569, -4.541064518000417216, -2.621784821875001281 ) ) ;
#35121 = UNCERTAINTY_MEASURE_WITH_UNIT (LENGTH_MEASURE( 1.000000000000000082E-05 ), #24909, 'distance_accuracy_value', 'NONE');
#35122 = CARTESIAN_POINT ( 'NONE',  ( 6.478125000614516793, -4.541064518000419881, 2.621784821874995952 ) ) ;
#35123 = CARTESIAN_POINT ( 'NONE',  ( 15.75937500061451857, 4.119189519843966529, -2.378215178124998275 ) ) ;
#35124 = CARTESIAN_POINT ( 'NONE',  ( 17.92500000122903359, 2.886751345948126879, 4.999999999999998224 ) ) ;
#35125 = CARTESIAN_POINT ( 'NONE',  ( 13.23750000000000071, 5.773502691896255534, 3.535250795749688894E-16 ) ) ;
#35126 = CARTESIAN_POINT ( 'NONE',  ( 13.65937500061451715, 0.000000000000000000, 5.243569643749999010 ) ) ;
#35127 = CARTESIAN_POINT ( 'NONE',  ( 12.00000000122903465, 5.773502691896255534, 3.535250795749688894E-16 ) ) ;
#35128 = CARTESIAN_POINT ( 'NONE',  ( 16.95937500061451786, -4.541064518000417216, -2.621784821875001281 ) ) ;
#35129 = CARTESIAN_POINT ( 'NONE',  ( 18.18750000000000000, 5.773502691896255534, 3.535250795749688894E-16 ) ) ;
#35130 = CARTESIAN_POINT ( 'NONE',  ( 9.384375000614518569, 6.421520780324663323E-16, -5.243569643749999010 ) ) ;
#35131 = CARTESIAN_POINT ( 'NONE',  ( 4.243569643749999010, 11.96562500061451750, -32.45002607614398471 ) ) ;
#35132 = DIRECTION ( 'NONE',  ( 0.000000000000000000, 0.000000000000000000, 1.000000000000000000 ) ) ;
#35133 = CARTESIAN_POINT ( 'NONE',  ( 24.15937500061451715, 2.746126346562645981, -4.756430356249997438 ) ) ;
#35134 = CARTESIAN_POINT ( 'NONE',  ( 1.071796769724489673, 13.43615380933863435, 26.00000000000000000 ) ) ;
#35135 = CARTESIAN_POINT ( 'NONE',  ( 24.29062500061451502, 6.054752690667223547, 3.707466751127219781E-16 ) ) ;
#35136 = CARTESIAN_POINT ( 'NONE',  ( -1.394453263437886604E-15, 19.66249999999999787, -26.00000000000000000 ) ) ;
#35137 = CARTESIAN_POINT ( 'NONE',  ( 28.84687500061452070, 6.054752690667223547, 3.707466751127219781E-16 ) ) ;
#35138 = ADVANCED_FACE ( 'NONE', ( #67325 ), #66582, .F. ) ;
#35139 = CARTESIAN_POINT ( 'NONE',  ( 23.81250000000000000, -5.773502691896255534, -1.060575238724906372E-15 ) ) ;
#35140 = B_SPLINE_CURVE_WITH_KNOTS ( 'NONE', 3,
 ( #36965, #31431, #53971, #4467, #50259, #26997, #43619, #66886, #38061, #60958 ),
 .UNSPECIFIED., .F., .F.,
 ( 4, 3, 3, 4 ),
 ( 2.168404344971008868E-19, 0.0001125111793028066998, 0.0001785213024883201523, 0.0002445501373023005053 ),
 .UNSPECIFIED. ) ;
#35141 = CARTESIAN_POINT ( 'NONE',  ( 5.690625000614516260, -3.027376345333610441, -5.243569643749999898 ) ) ;
#35142 = CARTESIAN_POINT ( 'NONE',  ( 25.43437500061451217, -2.746126346562642428, -4.756430356249999214 ) ) ;
#35143 = CARTESIAN_POINT ( 'NONE',  ( 19.39687500061451786, 6.054752690667223547, 3.707466751127219781E-16 ) ) ;
#35144 = CARTESIAN_POINT ( 'NONE',  ( 11.14687500061451608, 4.119189519843966529, -2.378215178124998275 ) ) ;
#35145 = CARTESIAN_POINT ( 'NONE',  ( 28.61250000122903359, 4.330127018922192761, -2.499999999999997780 ) ) ;
#35146 = CARTESIAN_POINT ( 'NONE',  ( 8.259375000614518569, 0.000000000000000000, 5.243569643749999010 ) ) ;
#35147 = ORIENTED_EDGE ( 'NONE', *, *, #65184, .F. ) ;
#35148 = CARTESIAN_POINT ( 'NONE',  ( 18.79687500061451644, -3.027376345333610441, -5.243569643749999898 ) ) ;
#35149 = CARTESIAN_POINT ( 'NONE',  ( 13.23750000122903359, 6.123233995736764310E-16, -4.999999999999998224 ) ) ;
#35150 = CARTESIAN_POINT ( 'NONE',  ( 27.63749999999999929, 5.773502691896255534, 3.535250795749688894E-16 ) ) ;
#35151 = CARTESIAN_POINT ( 'NONE',  ( 3.225000000000002309, 6.123233995736764310E-16, -4.999999999999998224 ) ) ;
#35152 = CARTESIAN_POINT ( 'NONE',  ( 1.071796769724491893, 12.14509619066136814, 33.99999999999999289 ) ) ;
#35153 = CARTESIAN_POINT ( 'NONE',  ( 17.84999999999999787, 0.000000000000000000, 4.999999999999998224 ) ) ;
#35154 = ORIENTED_EDGE ( 'NONE', *, *, #52783, .F. ) ;
#35155 = CARTESIAN_POINT ( 'NONE',  ( 10.72500000000000142, -4.330127018922194537, 2.499999999999995559 ) ) ;
#35156 = CARTESIAN_POINT ( 'NONE',  ( 11.48437500061451821, -2.746126346562642428, -4.756430356249999214 ) ) ;
#35157 = CARTESIAN_POINT ( 'NONE',  ( 24.70312500061451644, 4.541064518000418104, -2.621784821874998173 ) ) ;
#35158 = CARTESIAN_POINT ( 'NONE',  ( 13.79999999999999893, 0.000000000000000000, 4.999999999999998224 ) ) ;
#35159 = CARTESIAN_POINT ( 'NONE',  ( 10.42500000122903536, -5.773502691896255534, -1.060575238724906372E-15 ) ) ;
#35160 = CARTESIAN_POINT ( 'NONE',  ( 8.203125000614518214, 0.000000000000000000, 5.243569643749999010 ) ) ;
#35161 = CARTESIAN_POINT ( 'NONE',  ( 21.97500000000000142, -4.330127018922194537, 2.499999999999995559 ) ) ;
#35162 = CARTESIAN_POINT ( 'NONE',  ( 20.09062500061451573, -3.027376345333610441, -5.243569643749999898 ) ) ;
#35163 = CARTESIAN_POINT ( 'NONE',  ( 16.16250000122903430, 0.000000000000000000, 4.999999999999998224 ) ) ;
#35164 = CARTESIAN_POINT ( 'NONE',  ( 26.51250000122903216, 0.000000000000000000, 4.999999999999998224 ) ) ;
#35165 = CARTESIAN_POINT ( 'NONE',  ( 2.655984681222220721E-16, 17.70312499938548356, 25.66244784525396483 ) ) ;
#35166 = CARTESIAN_POINT ( 'NONE',  ( 5.549999999999998934, 4.330127018922192761, -2.499999999999997780 ) ) ;
#35167 = ORIENTED_EDGE ( 'NONE', *, *, #24217, .T. ) ;
#35168 = CARTESIAN_POINT ( 'NONE',  ( 21.81562500061451004, -6.054752690667223547, -1.112240025338166033E-15 ) ) ;
#35169 = CARTESIAN_POINT ( 'NONE',  ( 29.76562500061451644, 3.027376345333611329, 5.243569643749999010 ) ) ;
#35170 = CARTESIAN_POINT ( 'NONE',  ( 26.78437500061451360, -4.541064518000419881, 2.621784821874995952 ) ) ;
#35171 = CARTESIAN_POINT ( 'NONE',  ( 18.57187500061451857, 3.027376345333611329, 5.243569643749999010 ) ) ;
#35172 = CARTESIAN_POINT ( 'NONE',  ( 13.15312500061451750, 0.000000000000000000, 5.243569643749999010 ) ) ;
#35173 = CARTESIAN_POINT ( 'NONE',  ( 11.55000000000000071, 0.000000000000000000, 4.999999999999998224 ) ) ;
#35174 = CARTESIAN_POINT ( 'NONE',  ( 25.16250000122903074, 0.000000000000000000, 4.999999999999998224 ) ) ;
#35175 = CARTESIAN_POINT ( 'NONE',  ( 21.27187500061451786, 2.746126346562643317, 4.756430356249998326 ) ) ;
#35176 = CARTESIAN_POINT ( 'NONE',  ( 15.89062500061451644, -3.027376345333614438, 5.243569643749998122 ) ) ;
#35177 = CARTESIAN_POINT ( 'NONE',  ( 1.071796769724476572, 11.24509619066136779, -25.99999999999999289 ) ) ;
#35178 = CARTESIAN_POINT ( 'NONE',  ( 6.037500001229035185, 6.123233995736764310E-16, -4.999999999999998224 ) ) ;
#35179 = CARTESIAN_POINT ( 'NONE',  ( 11.74687500061451573, 6.054752690667223547, 3.707466751127219781E-16 ) ) ;
#35180 = CARTESIAN_POINT ( 'NONE',  ( 12.04687500061451821, -3.027376345333610441, -5.243569643749999898 ) ) ;
#35181 = CARTESIAN_POINT ( 'NONE',  ( 19.54687500061451644, -3.027376345333614438, 5.243569643749998122 ) ) ;
#35182 = ORIENTED_EDGE ( 'NONE', *, *, #68596, .T. ) ;
#35183 = CARTESIAN_POINT ( 'NONE',  ( 23.31562500061451715, 3.027376345333613106, -5.243569643749998122 ) ) ;
#35184 = CARTESIAN_POINT ( 'NONE',  ( 19.09687500061451360, -3.027376345333614438, 5.243569643749998122 ) ) ;
#35185 = CARTESIAN_POINT ( 'NONE',  ( 24.14062500061451289, -3.027376345333610441, -5.243569643749999898 ) ) ;
#35186 = DIRECTION ( 'NONE',  ( -1.000000000000000000, -0.000000000000000000, -0.000000000000000000 ) ) ;
#35187 = CARTESIAN_POINT ( 'NONE',  ( -3.999999999999997335, 15.53749999999999964, 32.30940107675850470 ) ) ;
#35188 = CARTESIAN_POINT ( 'NONE',  ( 3.346875000614518036, -3.027376345333614438, 5.243569643749998122 ) ) ;
#35189 = CARTESIAN_POINT ( 'NONE',  ( 9.150000001229033231, -2.886751345948125991, -5.000000000000000000 ) ) ;
#35190 = CARTESIAN_POINT ( 'NONE',  ( 4.087500001229035007, -4.330127018922194537, 2.499999999999995559 ) ) ;
#35191 = CYLINDRICAL_SURFACE ( 'NONE', #19753, 4.999999999999998224 ) ;
#35192 = CARTESIAN_POINT ( 'NONE',  ( 26.06250000122903288, 0.000000000000000000, 4.999999999999998224 ) ) ;
#35193 = CARTESIAN_POINT ( 'NONE',  ( 3.756430356250000546, 13.69062499938548250, 27.83122392262697886 ) ) ;
#35194 = CARTESIAN_POINT ( 'NONE',  ( 16.14375000122903359, -2.886751345948129988, 4.999999999999997335 ) ) ;
#35195 = CARTESIAN_POINT ( 'NONE',  ( 9.871875000614517504, 3.027376345333613106, -5.243569643749998122 ) ) ;
#35196 = CARTESIAN_POINT ( 'NONE',  ( 10.18125000122903323, 4.330127018922191873, 2.499999999999999556 ) ) ;
#35197 = EDGE_CURVE ( 'NONE', #42898, #22963, #38132, .T. ) ;
#35198 = CARTESIAN_POINT ( 'NONE',  ( 18.10312500061451502, 0.000000000000000000, 5.243569643749999010 ) ) ;
#35199 = CARTESIAN_POINT ( 'NONE',  ( 12.04687500061451821, -3.027376345333610441, -5.243569643749999898 ) ) ;
#35200 = CARTESIAN_POINT ( 'NONE',  ( 29.10000000122903074, 5.773502691896255534, 3.535250795749688894E-16 ) ) ;
#35201 = ADVANCED_FACE ( 'NONE', ( #72483 ), #60654, .F. ) ;
#35202 = CARTESIAN_POINT ( 'NONE',  ( 18.98437500061451644, 4.541064518000418104, 2.621784821874999949 ) ) ;
#35203 = CARTESIAN_POINT ( 'NONE',  ( 7.509375000614517681, -4.541064518000417216, -2.621784821875001281 ) ) ;
#35204 = CARTESIAN_POINT ( 'NONE',  ( 3.328125000614516438, -4.541064518000419881, 2.621784821874995952 ) ) ;
#35205 = CARTESIAN_POINT ( 'NONE',  ( -1.071796769724487453, 17.65759618943233633, 26.00000000000000000 ) ) ;
#35206 = CARTESIAN_POINT ( 'NONE',  ( 8.353125000614518569, -4.541064518000417216, -2.621784821875001281 ) ) ;
#35207 = CARTESIAN_POINT ( 'NONE',  ( 17.46562500061451217, 3.027376345333613106, -5.243569643749998122 ) ) ;
#35208 = ORIENTED_EDGE ( 'NONE', *, *, #5562, .F. ) ;
#35209 = CARTESIAN_POINT ( 'NONE',  ( 5.362500001229033586, 0.000000000000000000, 4.999999999999998224 ) ) ;
#35210 = CARTESIAN_POINT ( 'NONE',  ( 13.97812500061451679, 4.541064518000418104, 2.621784821874999949 ) ) ;
#35211 = CARTESIAN_POINT ( 'NONE',  ( 12.14062500061451821, 6.054752690667223547, 3.707466751127219781E-16 ) ) ;
#35212 = CARTESIAN_POINT ( 'NONE',  ( 22.62187500061451573, 2.746126346562643317, 4.756430356249998326 ) ) ;
#35213 = CARTESIAN_POINT ( 'NONE',  ( 13.31250000000000178, 2.886751345948126879, 4.999999999999999112 ) ) ;
#35214 = CARTESIAN_POINT ( 'NONE',  ( 7.162500001229032520, 0.000000000000000000, 4.999999999999998224 ) ) ;
#35215 = CARTESIAN_POINT ( 'NONE',  ( 3.553125000614516082, 4.541064518000418104, -2.621784821874998173 ) ) ;
#35216 =( BOUNDED_CURVE ( )  B_SPLINE_CURVE ( 2, ( #58186, #30128, #1702, #64466, #52659, #53023, #63016 ),
 .UNSPECIFIED., .F., .F. ) 
 B_SPLINE_CURVE_WITH_KNOTS ( ( 3, 2, 2, 3 ),
 ( 0.2000000000000000389, 0.2033333333333333659, 0.2066666666666667207, 0.2100000000000000477 ),
 .UNSPECIFIED. ) 
 CURVE ( )  GEOMETRIC_REPRESENTATION_ITEM ( )  RATIONAL_B_SPLINE_CURVE ( ( 0.9999999999999988898, 0.8660254037844398178, 1.000000000000000000, 0.8660254037844387076, 1.000000000000000000, 0.8660254037844364872, 1.000000000000002220 ) ) 
 REPRESENTATION_ITEM ( '' )  );
#35217 = CARTESIAN_POINT ( 'NONE',  ( 18.60000000122903430, -2.886751345948125991, -5.000000000000000000 ) ) ;
#35218 = CARTESIAN_POINT ( 'NONE',  ( 25.50000000000000000, 0.000000000000000000, 4.999999999999998224 ) ) ;
#35219 = CARTESIAN_POINT ( 'NONE',  ( -4.243569643749999898, 11.27187500061451608, -32.45002607614398471 ) ) ;
#35220 = CARTESIAN_POINT ( 'NONE',  ( 0.000000000000000000, 27.50000000000000000, 26.00000000000000000 ) ) ;
#35221 = CARTESIAN_POINT ( 'NONE',  ( 12.84375000122903288, 5.773502691896255534, 3.535250795749688401E-16 ) ) ;
#35222 = EDGE_CURVE ( 'NONE', #28145, #37967, #32600, .T. ) ;
#35223 = CARTESIAN_POINT ( 'NONE',  ( -3.999999999999999112, 13.25000000000000178, 30.00000000000000000 ) ) ;
#35224 = CARTESIAN_POINT ( 'NONE',  ( 17.52187500061451431, 3.027376345333613106, -5.243569643749998122 ) ) ;
#35225 = CARTESIAN_POINT ( 'NONE',  ( 22.89375000122903003, -2.886751345948130876, 4.999999999999996447 ) ) ;
#35226 = CARTESIAN_POINT ( 'NONE',  ( 14.05312500061451431, 0.000000000000000000, 5.243569643749999010 ) ) ;
#35227 = CARTESIAN_POINT ( 'NONE',  ( 9.318750001229034297, 2.886751345948126879, 4.999999999999999112 ) ) ;
#35228 = LINE ( 'NONE', #1263, #24756 ) ;
#35229 = CARTESIAN_POINT ( 'NONE',  ( 25.58437500061451431, 6.421520780324663323E-16, -5.243569643749999010 ) ) ;
#35230 = CARTESIAN_POINT ( 'NONE',  ( 18.60937500061450578, -5.492252693125287522, -1.008910452111647106E-15 ) ) ;
#35231 = CARTESIAN_POINT ( 'NONE',  ( 13.30312500061451786, -4.541064518000417216, -2.621784821875001281 ) ) ;
#35232 = CARTESIAN_POINT ( 'NONE',  ( 15.79687500061451821, 6.054752690667223547, 3.707466751127219781E-16 ) ) ;
#35233 = ORIENTED_EDGE ( 'NONE', *, *, #37992, .F. ) ;
#35234 = CARTESIAN_POINT ( 'NONE',  ( 26.76562500061451644, -6.054752690667223547, -1.112240025338166033E-15 ) ) ;
#35235 = CARTESIAN_POINT ( 'NONE',  ( 19.75312500061451360, 4.541064518000418104, -2.621784821874998173 ) ) ;
#35236 = CARTESIAN_POINT ( 'NONE',  ( 29.09062500061451573, -3.027376345333610441, -5.243569643749999898 ) ) ;
#35237 = CARTESIAN_POINT ( 'NONE',  ( -1.394453263437886801E-15, 19.66249999999999787, 33.99999999999999289 ) ) ;
#35238 = CARTESIAN_POINT ( 'NONE',  ( 9.000000000000001776, -4.330127018922190985, -2.500000000000001332 ) ) ;
#35239 = CARTESIAN_POINT ( 'NONE',  ( 18.82500000122903216, 2.886751345948126879, 4.999999999999999112 ) ) ;
#35240 = CARTESIAN_POINT ( 'NONE',  ( -0.6945831915928805111, 10.00052343484236772, 26.06076730949330411 ) ) ;
#35241 = CARTESIAN_POINT ( 'NONE',  ( 10.88437500061451679, -2.746126346562646425, 4.756430356249996549 ) ) ;
#35242 = ORIENTED_EDGE ( 'NONE', *, *, #46955, .F. ) ;
#35243 = CARTESIAN_POINT ( 'NONE',  ( 18.26249999999999929, 2.886751345948126879, 4.999999999999999112 ) ) ;
#35244 = CARTESIAN_POINT ( 'NONE',  ( 21.41250000000000497, 2.886751345948126879, 4.999999999999999112 ) ) ;
#35245 = CARTESIAN_POINT ( 'NONE',  ( 19.20937500061451786, -4.541064518000417216, -2.621784821875001281 ) ) ;
#35246 = CARTESIAN_POINT ( 'NONE',  ( 24.14062500061451289, -3.027376345333610441, -5.243569643749999898 ) ) ;
#35247 = ORIENTED_EDGE ( 'NONE', *, *, #51473, .T. ) ;
#35248 = CARTESIAN_POINT ( 'NONE',  ( 5.353125000614515905, 4.541064518000418104, -2.621784821874998173 ) ) ;
#35249 = CARTESIAN_POINT ( 'NONE',  ( 9.131250001229034297, 6.123233995736764310E-16, -4.999999999999998224 ) ) ;
#35250 = CARTESIAN_POINT ( 'NONE',  ( 15.00000000000000000, 4.330127018922192761, -2.499999999999997780 ) ) ;
#35251 = CARTESIAN_POINT ( 'NONE',  ( 4.243569643749999010, 17.36562500061451786, 27.54997392385601174 ) ) ;
#35252 = CARTESIAN_POINT ( 'NONE',  ( 29.80312500061451431, 0.000000000000000000, 5.243569643749999010 ) ) ;
#35253 = CARTESIAN_POINT ( 'NONE',  ( 10.95000000000000107, 4.330127018922192761, -2.499999999999997780 ) ) ;
#35254 = CARTESIAN_POINT ( 'NONE',  ( -3.756430356250001434, 17.85312499938548214, 32.16877607737301048 ) ) ;
#35255 = CARTESIAN_POINT ( 'NONE',  ( 26.78437500061451360, -4.541064518000419881, 2.621784821874995952 ) ) ;
#35256 = EDGE_LOOP ( 'NONE', ( #21125, #73100, #58950, #33206, #44030, #38993 ) ) ;
#35257 = CARTESIAN_POINT ( 'NONE',  ( 22.64062500061451644, -3.027376345333614438, 5.243569643749998122 ) ) ;
#35258 = CARTESIAN_POINT ( 'NONE',  ( 22.43437500061451573, 6.421520780324663323E-16, -5.243569643749999010 ) ) ;
#35259 = CARTESIAN_POINT ( 'NONE',  ( 4.243569643749999898, 17.29062500061459318, -27.54997392385601529 ) ) ;
#35260 = CARTESIAN_POINT ( 'NONE',  ( 7.003125000614518036, -4.541064518000417216, -2.621784821875001281 ) ) ;
#35261 = CARTESIAN_POINT ( 'NONE',  ( 29.82187500061451502, 2.746126346562643317, 4.756430356249998326 ) ) ;
#35262 = CARTESIAN_POINT ( 'NONE',  ( 24.74062500061451786, 6.054752690667223547, 3.707466751127219781E-16 ) ) ;
#35263 = CARTESIAN_POINT ( 'NONE',  ( 27.53437500061451360, -2.746126346562646425, 4.756430356249996549 ) ) ;
#35264 = CARTESIAN_POINT ( 'NONE',  ( 12.19687500061451679, 5.492252693125287522, 3.363034840372157021E-16 ) ) ;
#35265 = CARTESIAN_POINT ( 'NONE',  ( 16.24687500061451573, 6.054752690667223547, 3.707466751127219781E-16 ) ) ;
#35266 = CARTESIAN_POINT ( 'NONE',  ( 19.58437500061451786, -4.541064518000419881, 2.621784821874995952 ) ) ;
#35267 = CARTESIAN_POINT ( 'NONE',  ( 27.60937500061451644, 0.000000000000000000, 5.243569643749999010 ) ) ;
#35268 = CARTESIAN_POINT ( 'NONE',  ( 2.121784821875001281, 15.50937500061451857, 33.67503911421598417 ) ) ;
#35269 = CARTESIAN_POINT ( 'NONE',  ( 7.453125000614516438, -4.541064518000417216, -2.621784821875001281 ) ) ;
#35271 =( BOUNDED_CURVE ( )  B_SPLINE_CURVE ( 2, ( #66137, #26624, #26993, #49161, #33250, #65771, #43615, #71692, #55426 ),
 .UNSPECIFIED., .F., .F. ) 
 B_SPLINE_CURVE_WITH_KNOTS ( ( 3, 2, 2, 2, 3 ),
 ( 0.4027777777777777901, 0.4074074074074073848, 0.4166666666666666852, 0.4259259259259259300, 0.4305555555555555802 ),
 .UNSPECIFIED. ) 
 CURVE ( )  GEOMETRIC_REPRESENTATION_ITEM ( )  RATIONAL_B_SPLINE_CURVE ( ( 0.9330127018922194093, 0.9330127018922197424, 1.000000000000000000, 0.8660254037844387076, 1.000000000000000000, 0.8660254037844387076, 1.000000000000000000, 0.9330127018922189652, 0.9330127018922194093 ) ) 
 REPRESENTATION_ITEM ( '' )  );
#35270 = CYLINDRICAL_SURFACE ( 'NONE', #50195, 4.999999999999998224 ) ;
#35272 = CARTESIAN_POINT ( 'NONE',  ( 4.021875000614516082, 3.027376345333613106, -5.243569643749998122 ) ) ;
#35273 = CARTESIAN_POINT ( 'NONE',  ( 8.737500001229033586, 6.123233995736764310E-16, -4.999999999999998224 ) ) ;
#35274 = CARTESIAN_POINT ( 'NONE',  ( 6.065625000614516260, -6.054752690667223547, -1.112240025338166033E-15 ) ) ;
#35275 = CARTESIAN_POINT ( 'NONE',  ( 8.596875000614518925, 6.054752690667223547, 3.707466751127219781E-16 ) ) ;
#35276 = CARTESIAN_POINT ( 'NONE',  ( 16.80000000122903359, -2.886751345948125991, -5.000000000000000000 ) ) ;
#35277 = CARTESIAN_POINT ( 'NONE',  ( 5.634375000614519458, -4.541064518000419881, 2.621784821874995952 ) ) ;
#35278 = CARTESIAN_POINT ( 'NONE',  ( 6.778125000614518392, 4.541064518000418104, 2.621784821874999949 ) ) ;
#35279 = CARTESIAN_POINT ( 'NONE',  ( -8.484601909799255319E-16, 13.68124999877096748, 34.61880215351700940 ) ) ;
#35280 = CARTESIAN_POINT ( 'NONE',  ( 22.78125000122903288, 4.330127018922191873, 2.499999999999999556 ) ) ;
#35281 = CARTESIAN_POINT ( 'NONE',  ( 17.74687500061451928, -3.027376345333614438, 5.243569643749998122 ) ) ;
#35282 = CARTESIAN_POINT ( 'NONE',  ( -2.498395430326213790E-14, 19.30624999877096926, 26.00000000000000000 ) ) ;
#35283 = ORIENTED_EDGE ( 'NONE', *, *, #72649, .T. ) ;
#35284 = CARTESIAN_POINT ( 'NONE',  ( 24.17812500061451786, 6.421520780324663323E-16, -5.243569643749999010 ) ) ;
#35285 = CARTESIAN_POINT ( 'NONE',  ( 10.79062500061451679, 6.054752690667223547, 3.707466751127219781E-16 ) ) ;
#35286 = CARTESIAN_POINT ( 'NONE',  ( 27.45937500061451786, 4.541064518000418104, -2.621784821874998173 ) ) ;
#35287 = CARTESIAN_POINT ( 'NONE',  ( 9.140625000614518214, -3.027376345333614438, 5.243569643749998122 ) ) ;
#35288 = CARTESIAN_POINT ( 'NONE',  ( -3.000416591977282496E-16, 10.74687500061451928, -34.90005215228797653 ) ) ;
#35289 = CARTESIAN_POINT ( 'NONE',  ( 11.47500000122903252, 2.886751345948129099, -4.999999999999998224 ) ) ;
#35290 = EDGE_CURVE ( 'NONE', #10453, #1565, #34393, .T. ) ;
#35291 = CARTESIAN_POINT ( 'NONE',  ( 25.82812500061451644, -4.541064518000419881, 2.621784821874995952 ) ) ;
#35292 = CARTESIAN_POINT ( 'NONE',  ( 9.001249775931846008E-16, 12.71562500061451750, -25.09994784771203058 ) ) ;
#35293 = CARTESIAN_POINT ( 'NONE',  ( 12.18750000122903465, -4.330127018922194537, 2.499999999999995559 ) ) ;
#35294 = CARTESIAN_POINT ( 'NONE',  ( 22.30312500061451431, -4.541064518000417216, -2.621784821875001281 ) ) ;
#35295 = CARTESIAN_POINT ( 'NONE',  ( 11.02500000000000036, 4.330127018922191873, 2.499999999999999556 ) ) ;
#35296 = CARTESIAN_POINT ( 'NONE',  ( 19.30312500061451786, 4.541064518000418104, -2.621784821874998173 ) ) ;
#35297 = CARTESIAN_POINT ( 'NONE',  ( 6.196875000614517681, -3.027376345333610441, -5.243569643749999898 ) ) ;
#35298 = CARTESIAN_POINT ( 'NONE',  ( 21.60000000000000142, -4.330127018922190985, -2.500000000000001332 ) ) ;
#35299 = CARTESIAN_POINT ( 'NONE',  ( 12.71250000122903145, -4.330127018922190985, -2.500000000000001332 ) ) ;
#35300 = CARTESIAN_POINT ( 'NONE',  ( 13.94062500061451892, 6.054752690667223547, 3.707466751127219781E-16 ) ) ;
#35301 = CARTESIAN_POINT ( 'NONE',  ( 16.34062500061451573, -3.027376345333614438, 5.243569643749998122 ) ) ;
#35302 = CARTESIAN_POINT ( 'NONE',  ( 25.12500000122903288, 2.886751345948126879, 4.999999999999999112 ) ) ;
#35303 = CARTESIAN_POINT ( 'NONE',  ( 21.41250000000000497, 2.886751345948126879, 4.999999999999999112 ) ) ;
#35304 = CARTESIAN_POINT ( 'NONE',  ( 23.97187500061451360, 3.027376345333611329, 5.243569643749999010 ) ) ;
#35305 = FACE_OUTER_BOUND ( 'NONE', #60177, .T. ) ;
#35306 = CARTESIAN_POINT ( 'NONE',  ( 6.712500001229034119, 0.000000000000000000, 4.999999999999998224 ) ) ;
#35307 = CARTESIAN_POINT ( 'NONE',  ( 9.009375000614518569, 4.541064518000418104, -2.621784821874998173 ) ) ;
#35308 = CARTESIAN_POINT ( 'NONE',  ( 25.39687500061451431, -3.027376345333614438, 5.243569643749998122 ) ) ;
#35309 = EDGE_CURVE ( 'NONE', #12269, #23263, #13671, .T. ) ;
#35310 = CARTESIAN_POINT ( 'NONE',  ( 30.00000000000000000, 0.000000000000000000, 4.999999999999998224 ) ) ;
#35311 = CARTESIAN_POINT ( 'NONE',  ( 21.51562500061451644, 3.027376345333613106, -5.243569643749998122 ) ) ;
#35312 = CARTESIAN_POINT ( 'NONE',  ( 27.83437500061451786, 6.421520780324663323E-16, -5.243569643749999010 ) ) ;
#35313 = CARTESIAN_POINT ( 'NONE',  ( -3.756430356250000990, 17.06562499938548072, 32.16877607737301048 ) ) ;
#35314 = CARTESIAN_POINT ( 'NONE',  ( 18.71250000000000213, 2.886751345948161074, 4.999999999999941380 ) ) ;
#35315 = CARTESIAN_POINT ( 'NONE',  ( 8.409375000614518925, -4.541064518000417216, -2.621784821875001281 ) ) ;
#35316 = CARTESIAN_POINT ( 'NONE',  ( 18.51562500061451289, 3.027376345333611329, 5.243569643749999010 ) ) ;
#35317 = ORIENTED_EDGE ( 'NONE', *, *, #46133, .F. ) ;
#35318 = DIRECTION ( 'NONE',  ( -0.000000000000000000, -1.000000000000000000, -0.000000000000000000 ) ) ;
#35319 = CARTESIAN_POINT ( 'NONE',  ( 28.52812500061451573, -4.541064518000419881, 2.621784821874995952 ) ) ;
#35320 = CARTESIAN_POINT ( 'NONE',  ( 3.159375000614518036, 4.541064518000418104, -2.621784821874998173 ) ) ;
#35321 = CARTESIAN_POINT ( 'NONE',  ( 22.87500000122903288, 2.886751345948126879, 4.999999999999998224 ) ) ;
#35322 = CARTESIAN_POINT ( 'NONE',  ( 30.00000000000000000, 0.000000000000000000, 0.000000000000000000 ) ) ;
#35323 = CARTESIAN_POINT ( 'NONE',  ( 17.58749999999999858, -2.886751345948125991, -5.000000000000000000 ) ) ;
#35324 = CARTESIAN_POINT ( 'NONE',  ( 21.36562500061451431, -6.054752690667223547, -1.112240025338166033E-15 ) ) ;
#35325 = ORIENTED_EDGE ( 'NONE', *, *, #62575, .T. ) ;
#35326 = CARTESIAN_POINT ( 'NONE',  ( 24.60000000000000142, 0.000000000000000000, 4.999999999999998224 ) ) ;
#35327 = CARTESIAN_POINT ( 'NONE',  ( 26.10937500061451644, 4.541064518000418104, -2.621784821874998173 ) ) ;
#35328 = VERTEX_POINT ( 'NONE', #32962 ) ;
#35329 = CARTESIAN_POINT ( 'NONE',  ( 16.00312500061451715, -4.541064518000417216, -2.621784821875001281 ) ) ;
#35330 = CARTESIAN_POINT ( 'NONE',  ( 5.015625000614518214, 3.027376345333611329, 5.243569643749999010 ) ) ;
#35331 = CARTESIAN_POINT ( 'NONE',  ( 18.15937500061451715, -5.492252693125287522, -1.008910452111647106E-15 ) ) ;
#35332 = CARTESIAN_POINT ( 'NONE',  ( 29.31562500061451715, 3.027376345333611329, 5.243569643749999010 ) ) ;
#35333 = CARTESIAN_POINT ( 'NONE',  ( 16.16250000122903430, 0.000000000000000000, 4.999999999999998224 ) ) ;
#35334 = CARTESIAN_POINT ( 'NONE',  ( 22.23750000000000071, 5.773502691896255534, 3.535250795749688894E-16 ) ) ;
#35335 = CARTESIAN_POINT ( 'NONE',  ( 28.19999999999999929, 0.000000000000000000, 4.999999999999998224 ) ) ;
#35336 = CARTESIAN_POINT ( 'NONE',  ( 5.334375000614517859, 6.421520780324663323E-16, -5.243569643749999010 ) ) ;
#35337 = CARTESIAN_POINT ( 'NONE',  ( 9.609375000614518214, 0.000000000000000000, 5.243569643749999010 ) ) ;
#35338 = CARTESIAN_POINT ( 'NONE',  ( 19.20937500061451786, -4.541064518000417216, -2.621784821875001281 ) ) ;
#35339 = CARTESIAN_POINT ( 'NONE',  ( -2.000000000000000000, 15.08750000122903501, -33.46410161513775705 ) ) ;
#35340 = ORIENTED_EDGE ( 'NONE', *, *, #49345, .T. ) ;
#35341 = CARTESIAN_POINT ( 'NONE',  ( 28.11562500061451431, -6.054752690667223547, -1.112240025338166033E-15 ) ) ;
#35342 = CARTESIAN_POINT ( 'NONE',  ( 3.112500000000000711, -5.773502691896255534, -1.060575238724906372E-15 ) ) ;
#35343 = CARTESIAN_POINT ( 'NONE',  ( 4.696875000614518569, -3.027376345333614438, 5.243569643749998122 ) ) ;
#35344 = CARTESIAN_POINT ( 'NONE',  ( 18.11250000000000071, 2.886751345948129099, -4.999999999999998224 ) ) ;
#35345 = CARTESIAN_POINT ( 'NONE',  ( 12.55312500061451786, 4.541064518000418104, -2.621784821874998173 ) ) ;
#35346 = CARTESIAN_POINT ( 'NONE',  ( 26.88749999999999929, -2.886751345948121994, 5.000000000000011546 ) ) ;
#35347 = CARTESIAN_POINT ( 'NONE',  ( 4.763386231524743053, 8.796087519298447788, 26.33157461438974423 ) ) ;
#35348 = CARTESIAN_POINT ( 'NONE',  ( 20.59687500061451360, -2.746126346562642428, -4.756430356249999214 ) ) ;
#35349 = CARTESIAN_POINT ( 'NONE',  ( 7.340625000614518392, -3.027376345333614438, 5.243569643749998122 ) ) ;
#35350 = CARTESIAN_POINT ( 'NONE',  ( 24.98437500061451644, -4.541064518000419881, 2.621784821874995952 ) ) ;
#35351 = CARTESIAN_POINT ( 'NONE',  ( 19.68750000122903288, 4.330127018922191873, 2.499999999999999556 ) ) ;
#35352 = CARTESIAN_POINT ( 'NONE',  ( 25.88437500061451502, -4.541064518000419881, 2.621784821874995952 ) ) ;
#35353 = CARTESIAN_POINT ( 'NONE',  ( 6.562500000000001776, 2.886751345948126879, 4.999999999999999112 ) ) ;
#35354 = CARTESIAN_POINT ( 'NONE',  ( -3.999999999999999556, 13.32500000122903572, 27.69059892324149530 ) ) ;
#35355 = CARTESIAN_POINT ( 'NONE',  ( 15.70312500061451644, 4.541064518000418104, -2.621784821874998173 ) ) ;
#35356 = CARTESIAN_POINT ( 'NONE',  ( 6.150000001229033231, 5.773502691896255534, 3.535250795749688894E-16 ) ) ;
#35357 = CARTESIAN_POINT ( 'NONE',  ( 16.92187500061451999, -6.054752690667223547, -1.112240025338166033E-15 ) ) ;
#35358 = CARTESIAN_POINT ( 'NONE',  ( 11.70937500061451608, 4.541064518000418104, -2.621784821874998173 ) ) ;
#35359 = DIRECTION ( 'NONE',  ( -0.000000000000000000, -1.000000000000000000, -0.000000000000000000 ) ) ;
#35360 = VERTEX_POINT ( 'NONE', #4893 ) ;
#35361 = CARTESIAN_POINT ( 'NONE',  ( 11.72812500061451857, 4.541064518000418104, 2.621784821874999949 ) ) ;
#35362 = CARTESIAN_POINT ( 'NONE',  ( 30.00000000000000000, 0.000000000000000000, 4.999999999999998224 ) ) ;
#35363 = CARTESIAN_POINT ( 'NONE',  ( 23.55000000122903359, -2.886751345948125991, -5.000000000000000000 ) ) ;
#35364 = CARTESIAN_POINT ( 'NONE',  ( 12.27187500061451786, 3.027376345333611329, 5.243569643749999010 ) ) ;
#35365 = CARTESIAN_POINT ( 'NONE',  ( 3.834375000614519635, -4.541064518000419881, 2.621784821874995952 ) ) ;
#35366 = CARTESIAN_POINT ( 'NONE',  ( 14.42812500061451786, 4.541064518000418104, 2.621784821874999949 ) ) ;
#35367 = DIRECTION ( 'NONE',  ( -1.000000000000000000, -0.000000000000000000, -0.000000000000000000 ) ) ;
#35368 = CARTESIAN_POINT ( 'NONE',  ( 23.25937500061451857, -4.541064518000417216, -2.621784821875001281 ) ) ;
#35369 = DIRECTION ( 'NONE',  ( -1.000000000000000000, -0.000000000000000000, -0.000000000000000000 ) ) ;
#35370 = CARTESIAN_POINT ( 'NONE',  ( 12.60000000122903430, -2.886751345948129988, 4.999999999999997335 ) ) ;
#35371 = CARTESIAN_POINT ( 'NONE',  ( 23.69999999999999929, 0.000000000000000000, 4.999999999999998224 ) ) ;
#35372 = CARTESIAN_POINT ( 'NONE',  ( 22.81875000122903074, 2.886751345948126879, 4.999999999999998224 ) ) ;
#35373 = CARTESIAN_POINT ( 'NONE',  ( 4.243569643749999898, 17.38437500061451502, -30.00000000000000000 ) ) ;
#35374 = CARTESIAN_POINT ( 'NONE',  ( 18.19687500061451502, -3.027376345333614438, 5.243569643749998122 ) ) ;
#35375 = CARTESIAN_POINT ( 'NONE',  ( 17.10000000122903430, -2.886751345948129988, 4.999999999999997335 ) ) ;
#35376 = CARTESIAN_POINT ( 'NONE',  ( 12.68437500061451573, 4.541064518000418104, 2.621784821874999949 ) ) ;
#35377 = CARTESIAN_POINT ( 'NONE',  ( -2.121784821874996840, 10.48437500061451821, 33.67503911421598417 ) ) ;
#35378 = CARTESIAN_POINT ( 'NONE',  ( 20.92500000122903714, 2.886751345948129099, -4.999999999999998224 ) ) ;
#35379 = CARTESIAN_POINT ( 'NONE',  ( 13.97812500061451679, 4.541064518000418104, 2.621784821874999949 ) ) ;
#35380 = ORIENTED_EDGE ( 'NONE', *, *, #73023, .F. ) ;
#35381 = VERTEX_POINT ( 'NONE', #5252 ) ;
#35382 = CARTESIAN_POINT ( 'NONE',  ( 18.97499999999999787, 6.123233995736764310E-16, -4.999999999999998224 ) ) ;
#35383 = CARTESIAN_POINT ( 'NONE',  ( 2.000000000000000444, 14.37500000000000000, 26.53589838486224650 ) ) ;
#35384 = CARTESIAN_POINT ( 'NONE',  ( 4.027123420325200875, 2.963623535648654883, 4.154172641102294783 ) ) ;
#35385 = CARTESIAN_POINT ( 'NONE',  ( 15.97500000122903430, 2.886751345948129099, -4.999999999999998224 ) ) ;
#35386 = CARTESIAN_POINT ( 'NONE',  ( 26.55937500061451573, 4.541064518000418104, -2.621784821874998173 ) ) ;
#35387 = CARTESIAN_POINT ( 'NONE',  ( 19.22812500061451502, 6.421520780324663323E-16, -5.243569643749999010 ) ) ;
#35388 = CARTESIAN_POINT ( 'NONE',  ( 22.71562500061451573, -6.054752690667223547, -1.112240025338166033E-15 ) ) ;
#35389 = CARTESIAN_POINT ( 'NONE',  ( 29.55000000122903003, 5.773502691896255534, 3.535250795749688894E-16 ) ) ;
#35390 = CARTESIAN_POINT ( 'NONE',  ( 28.23750000000000426, -2.886751345948129988, 4.999999999999997335 ) ) ;
#35391 = CARTESIAN_POINT ( 'NONE',  ( 3.999999999999998668, 11.82500000122903394, 27.69059892324149530 ) ) ;
#35392 = CARTESIAN_POINT ( 'NONE',  ( 8.409375000614518925, -4.119189519843965641, -2.378215178125001383 ) ) ;
#35393 = CARTESIAN_POINT ( 'NONE',  ( 12.78750000122903430, 6.123233995736764310E-16, -4.999999999999998224 ) ) ;
#35394 = CARTESIAN_POINT ( 'NONE',  ( 4.243569643749999010, 15.62187500061451928, -32.45002607614398471 ) ) ;
#35395 = CARTESIAN_POINT ( 'NONE',  ( 5.887500001229034829, -4.330127018922194537, 2.499999999999995559 ) ) ;
#35396 = CARTESIAN_POINT ( 'NONE',  ( 5.737499999999998934, -2.886751345948129988, 4.999999999999997335 ) ) ;
#35397 = EDGE_CURVE ( 'NONE', #49807, #57706, #39596, .T. ) ;
#35398 = CARTESIAN_POINT ( 'NONE',  ( 2.971875000614517592, -6.054752690667223547, -1.112240025338166033E-15 ) ) ;
#35399 = CARTESIAN_POINT ( 'NONE',  ( 10.02187500061451964, 3.027376345333611329, 5.243569643749999010 ) ) ;
#35400 = CARTESIAN_POINT ( 'NONE',  ( 29.39062500061451289, -3.027376345333614438, 5.243569643749998122 ) ) ;
#35401 = CARTESIAN_POINT ( 'NONE',  ( 27.41250000122903430, 0.000000000000000000, 4.999999999999998224 ) ) ;
#35402 = CARTESIAN_POINT ( 'NONE',  ( -5.790145606462772321, 8.153486631126842354, -28.41457251781636728 ) ) ;
#35403 = CARTESIAN_POINT ( 'NONE',  ( 24.20625000122903359, 0.000000000000000000, 4.999999999999998224 ) ) ;
#35404 = CARTESIAN_POINT ( 'NONE',  ( 8.521875000614516082, 3.027376345333613106, -5.243569643749998122 ) ) ;
#35405 = CARTESIAN_POINT ( 'NONE',  ( 11.33437500061451608, 4.541064518000418104, 2.621784821874999949 ) ) ;
#35406 = CARTESIAN_POINT ( 'NONE',  ( 6.412500000000001421, 2.886751345948129099, -4.999999999999998224 ) ) ;
#35407 = CARTESIAN_POINT ( 'NONE',  ( -4.243569643749999898, 14.81562500061459531, 27.54997392385601529 ) ) ;
#35408 =( BOUNDED_SURFACE ( )  B_SPLINE_SURFACE ( 1, 2, ( 
 ( #25564, #10405, #20003, #43299, #26299, #48105, #20373, #42556, #54379, #38482, #65083, #70628, #14474, #42924, #4512, #14840, #72094, #31474, #21478, #65448, #37380, #54741, #44031, #37008, #10040, #32574, #59904, #9309, #45838, #11130, #51018, #10767, #50660, #61370, #5948, #28132, #62817, #27767, #414, #62456, #11854, #72458, #22923, #34017, #21843, #12209, #50307, #55838, #11495, #40295, #33300, #67653, #5225, #56554, #34373, #45118, #64, #45481, #72829, #39578, #22570, #68013, #17385, #16301, #66932, #62101, #44766, #38855, #39943, #44406, #5595, #56906, #33657, #55475, #22212, #67301, #28481, #16659, #51379, #39217, #6311, #28840, #781, #61729, #23290, #56202, #68375, #17736, #4867, #17019, #27403, #49933, #46197, #41384, #68738, #69102, #52464, #69463, #63178, #18464, #57630, #42112, #13653, #70177, #64635, #36196, #69818, #63543, #25101, #35106, #18821, #34738, #19554, #51743, #1871, #35464, #57267, #52102, #1142, #12929, #47645, #23653, #6679, #29207, #29565, #58714, #46560, #30653, #18096, #8126, #1507, #12572, #63896, #2582, #40657, #35823, #57986, #41027, #7036, #24011, #7396, #30293, #29924, #24377, #46925, #58346, #13286, #7757, #52825, #2227, #41737, #64265, #24740, #47284, #19184, #53185, #43943, #8854, #14389, #43213, #72012, #19924, #26214, #42478, #3325, #32486, #8485, #4056, #37295, #20654, #37655, #70916, #36926, #54653, #25477, #71651, #48753, #3689, #59818, #59447, #49480, #70549, #26953, #2949, #25851, #48023, #65001, #31391, #65733, #53930, #60543, #71277, #32119, #15118, #54297, #21387, #14021, #15476, #48388, #36561, #60178, #9587, #20287, #42841, #26582, #49122, #65362, #21024, #43577, #14752, #66098, #38020, #9949, #59081, #4425, #55021, #9223, #31018, #53552, #31760, #33930, #10678, #11413, #45392, #60914, #56472, #16933, #73101, #17301, #67568, #22840, #27314, #44313, #44680, #50574, #66843, #28755, #22483, #38766, #55747, #33208, #61285, #67211, #56115, #5864, #11041, #39488, #49847, #67928, #5141, #696, #72372, #331, #16572, #39124, #28396, #27676, #39862, #23205, #50934, #10317, #62374, #11772, #34288, #56820, #62010, #6227, #5507, #61639, #51295, #16213, #45033, #33567, #66467, #15844, #21752, #4780, #38390, #50214, #72739, #32849, #55386, #28045, #22125, #1423, #45758, #34655, #29127, #24296, #36111, #1062, #30574, #35023, #24656, #35382, #69017, #35745, #6953, #41303, #53100, #51660, #63813, #18018, #47202, #2496, #13205, #18380, #12495, #68294, #69733, #40574, #23572, #1786, #13567, #62736, #46844, #40948, #29485, #17654, #58632, #23929, #58265, #46117, #63462, #68654, #69384, #12849, #40214, #63094, #7671, #52740, #2145, #12128, #30209, #18739, #57184, #6597, #57551, #52022, #19102, #46479, #57905, #7314, #29844, #52379, #64179, #41657, #8039, #48299, #31672, #48663, #8767, #47935, #65644, #36476, #9502, #59727, #14662, #70825, #25392, #60455, #26124, #9863, #37935, #37205, #20199, #32394, #43489, #53470, #43120, #8400, #15032, #31301, #25763, #71188, #30929, #54934, #9135, #54205, #25020, #2862, #47562, #42753, #59355, #70092, #70464, #20938, #64547, #3602, #20562, #32031, #64913, #37569, #42026, #60093, #54567, #3970, #42391, #26492, #15393, #58994, #49035, #19839, #53841, #65274, #71563, #14303, #3236, #36841, #19469, #66013, #13940, #11689, #5782, #39405, #33124, #67844, #4696, #39041, #34205, #62293, #21302, #44596, #5057, #4340, #21667, #43856, #55661, #17216, #66381, #26865, #49396, #72289, #28313, #16127, #249, #60825, #71927, #44224, #27226, #33478, #15757, #10231, #16484, #32765, #66757, #22757, #38297, #67486, #27594, #10957, #27958, #61201, #49763, #44949, #55302, #61923, #61555, #67127, #50126, #38680, #39777, #5420, #10596, #72657, #56028, #22037, #50490, #45308, #73016, #22400, #16849, #11329, #33848, #56392, #50849, #68210, #35656, #29400, #1331, #56739, #40133, #28672, #57462, #46031, #7581, #62647, #41216, #23120, #46391, #63375, #52292, #51575, #23843, #612, #68926, #18283, #12759, #29040, #1693, #63724, #17571, #40858, #12044, #23484, #6868, #35295, #34567, #68567, #57096, #6141, #69291, #51212, #45674, #6505, #974, #29755, #17926, #57816, #58176, #40489, #63004, #51934, #13116, #46756, #12401, #7226, #24204, #18654, #34936, #38537, #72151, #49624, #44457, #51072, #61424, #45540, #32988, #470, #66988, #27457, #5649, #17438, #66612, #50713, #72884, #33352, #6364, #39995, #5279, #45172, #4922, #44818, #55528, #116, #22265, #56960, #21901, #67703, #56607, #6003, #15988, #17075, #28184, #61061, #55890, #21530, #62509, #27825, #39636, #49988, #67352, #72512, #22621, #16715, #44085, #16350, #62154, #28536, #22978, #10459, #11551, #34067, #38905, #10818, #50357, #39270, #68069, #34431, #61782, #11186, #33713, #56258, #11907, #18767, #59025, #35772, #7702, #25049, #29872, #8426, #64943, #19499, #52049, #47592, #30963, #70121, #2529, #36143, #13967, #24685, #30238, #30602, #12877, #19131, #52771, #42056, #64579, #69045, #46507, #41685, #24324, #18408, #36505, #1453, #58295, #53498, #63843, #35053, #23959, #40974, #13597, #25421, #63489, #19869, #46873, #2890, #47230, #2173, #47964, #69412, #53129, #42422, #35410, #70491, #7342, #57580, #6983, #29514, #69763, #1817, #57935, #52409, #41333, #13234, #64208, #58662, #8070, #25793, #66044, #31700, #60861, #71594, #32429, #49065, #54598, #72320, #21700, #15792, #42782, #36868, #4003, #37966, #65302, #59758, #20968, #54966, #20230, #43522, #43889, #71218, #9893, #49426, #15422, #14335, #4727, #10264, #70856, #21335, #53873, #48695, #4371, #26156, #32796, #14693, #38332, #9165, #37235, #60487, #55333, #31331, #26901, #37601, #20595, #44257, #27262, #43154, #71961, #54235, #9532, #3632, #66414, #60123, #59387, #65675, #49794, #8797, #3265, #48331, #15064, #32066 ),
 ( #26526, #28341, #56421, #39434, #67158, #29070, #67873, #51606, #6537, #5810, #61954, #1006, #12076, #22070, #11717, #50158, #56767, #50520, #67515, #39805, #72688, #23513, #50878, #277, #66790, #44629, #16161, #11358, #27991, #38713, #16518, #62681, #33156, #22786, #62321, #642, #33509, #45338, #10627, #17245, #34233, #6171, #10989, #51240, #57126, #5089, #28700, #27625, #73048, #33876, #23151, #39071, #22430, #61586, #61232, #45705, #55694, #56058, #68239, #17602, #44977, #5451, #16879, #40162, #34598, #30873, #63036, #13147, #46788, #2805, #63405, #12434, #1726, #58937, #34968, #68598, #46063, #40890, #47506, #8344, #53413, #70036, #7982, #24239, #36422, #46423, #7614, #17958, #40520, #57495, #35688, #69323, #6899, #12790, #29430, #18683, #51967, #1366, #23876, #68961, #35327, #19409, #57850, #41968, #18318, #64490, #7259, #29787, #2090, #13882, #52324, #47147, #41246, #63758, #58209, #30150, #52684, #41602, #24599, #69678, #19044, #64121, #13507, #36054, #58574, #30518, #53044, #2439, #24961, #20884, #3916, #42333, #55251, #20143, #25706, #54513, #10179, #31242, #37517, #53783, #48979, #43438, #71876, #65219, #48609, #31979, #71508, #9081, #48243, #65960, #36783, #9809, #60038, #14980, #71134, #70767, #60772, #26438, #32714, #38243, #9449, #20507, #25333, #43802, #3179, #15340, #8709, #37880, #31617, #26070, #60401, #42697, #47878, #32341, #54879, #70407, #14609, #19783, #43064, #59673, #64857, #37147, #21248, #14245, #4285, #26811, #49344, #54153, #66327, #59299, #15705, #3548, #65589, #21985, #62242, #68158, #16074, #11278, #38624, #38991, #22349, #39356, #33071, #61506, #27540, #11993, #56690, #67790, #10903, #5369, #50797, #61148, #62597, #61870, #33798, #4647, #10543, #27176, #44901, #33431, #34516, #55610, #559, #44172, #56342, #200, #11638, #44544, #5731, #21617, #28266, #22705, #45257, #67075, #34153, #17521, #5006, #17164, #50072, #55975, #67438, #39723, #72604, #27908, #16434, #49710, #6090, #40083, #72238, #28621, #51158, #50442, #66702, #72967, #23069, #16799, #45624, #924, #24151, #57766, #13799, #1279, #23432, #12708, #69953, #45978, #6451, #57046, #51881, #58488, #68874, #52962, #40434, #7897, #23789, #34880, #13065, #24876, #68513, #58123, #7175, #40804, #28986, #47423, #35245, #52602, #12345, #52241, #62951, #7531, #29703, #64406, #29348, #2008, #64038, #13417, #17875, #24519, #35604, #57409, #51524, #46340, #6814, #30064, #41877, #18230, #69240, #63317, #47063, #69597, #30434, #1645, #46705, #63675, #18959, #18602, #41166, #41519, #35966, #2359, #19323, #27000, #9998, #37698, #72787, #38438, #22170, #50262, #49530, #32533, #44723, #55796, #65779, #55434, #20700, #43258, #72054, #15161, #60964, #32894, #10726, #4105, #60589, #43990, #10363, #21072, #60220, #4826, #47785, #21798, #21433, #66511, #55069, #9633, #67258, #27360, #36339, #58853, #15892, #4470, #8263, #5186, #32167, #49891, #54700, #72416, #43623, #38065, #44363, #26632, #30794, #66890, #16258, #53324, #49169, #2723, #38813, #71700, #25239, #66145, #33258, #71325, #61328, #27724, #15523, #56514, #742, #33614, #23251, #17697, #34699, #33975, #1107, #6998, #28090, #45801, #50618, #50976, #34333, #51340, #45076, #373, #39535, #23974, #68700, #52064, #46522, #18060, #51704, #45439, #29529, #16978, #68337, #16616, #1468, #56158, #56866, #17345, #39171, #5907, #5552, #67972, #61687, #23, #11086, #22529, #11454, #40620, #28441, #12535, #67612, #63140, #22881, #62060, #40258, #57595, #39904, #62779, #62417, #11816, #6271, #28799, #12171, #57228, #6643, #29170, #23614, #46160, #35069, #3282, #41347, #64594, #2907, #25438, #12892, #13981, #47606, #35425, #25810, #63857, #69425, #25063, #53891, #24339, #52786, #18782, #69063, #47981, #31350, #18423, #70509, #30980, #24701, #59405, #13247, #30615, #40989, #63505, #57949, #36157, #69778, #7357, #35785, #29886, #47245, #8813, #52425, #1831, #46887, #58308, #19885, #7719, #64960, #30253, #42438, #2187, #19145, #70136, #36886, #41699, #19514, #64223, #13612, #58675, #8085, #53145, #36520, #2544, #42072, #59040, #8444, #53513, #14351, #20615, #43906, #55349, #4743, #65321, #66429, #26917, #14712, #5104, #43173, #48713, #4387, #33172, #54253, #60503, #3649, #71976, #15807, #21715, #15079, #71612, #54982, #21349, #32081, #71235, #38349, #59776, #32811, #9909, #37981, #20985, #65692, #10642, #49442, #55710, #61248, #32447, #43538, #48348, #66805, #26172, #60876, #31717, #10280, #54612, #49084, #27277, #37616, #70873, #49810, #72335, #20247, #60138, #42799, #66059, #9547, #37254, #4018, #44274, #9182, #16176, #38728, #26543, #15437, #11732, #44643, #34248, #28716, #45720, #44994, #12092, #17976, #39087, #56781, #61604, #61970, #45354, #62336, #293, #34985, #73064, #23166, #34613, #57143, #67173, #68255, #6187, #16534, #57513, #22445, #28007, #51256, #12454, #33526, #39821, #56076, #658, #17617, #1023, #67531, #50893, #40177, #62696, #11372, #50536, #6555, #11005, #29087, #51622, #17260, #22802, #16894, #63052, #23529, #27638, #40536, #46079, #67888, #50174, #68614, #5467, #72702, #39449, #22084, #33891, #28357, #56435, #5825, #64874, #41619, #13525, #6915, #63421, #29445, #24617, #41263, #14262, #12808, #2822, #46439, #36072, #2456, #13899, #46804, #64138, #23892, #58592, #7999, #24979, #24256, #64507, #70424, #18335, #30535, #40908, #63775, #47164, #53062, #35343, #13163, #29805, #36801, #58953, #42351, #51983, #8361, #41987, #35704, #19799, #7275, #47524, #1382, #68978, #57866, #69696, #7631, #52340, #69340, #1742, #58226, #18699, #30168, #52700, #2106, #19061, #30890, #70053, #25350, #19426, #53432, #36439, #47896, #15356, #27190, #3196, #60416, #9465, #43081, #16091, #49725, #14995, #54895, #14625, #54529, #65235, #9825, #25723, #32357 ) ),
 .UNSPECIFIED., .F., .F., .F. ) 
 B_SPLINE_SURFACE_WITH_KNOTS ( ( 2, 2 ),
 ( 3, 2, 2, 2, 2, 2, 2, 2, 2, 2, 2, 2, 2, 2, 2, 2, 2, 2, 2, 2, 2, 2, 2, 2, 2, 2, 2, 2, 2, 2, 2, 2, 2, 2, 2, 2, 2, 2, 2, 2, 2, 2, 2, 2, 2, 2, 2, 2, 2, 2, 2, 2, 2, 2, 2, 2, 2, 2, 2, 2, 2, 2, 2, 2, 2, 2, 2, 2, 2, 2, 2, 2, 2, 2, 2, 2, 2, 2, 2, 2, 2, 2, 2, 2, 2, 2, 2, 2, 2, 2, 2, 2, 2, 2, 2, 2, 2, 2, 2, 2, 2, 2, 2, 2, 2, 2, 2, 2, 2, 2, 2, 2, 2, 2, 2, 2, 2, 2, 2, 2, 2, 2, 2, 2, 2, 2, 2, 2, 2, 2, 2, 2, 2, 2, 2, 2, 2, 2, 2, 2, 2, 2, 2, 2, 2, 2, 2, 2, 2, 2, 2, 2, 2, 2, 2, 2, 2, 2, 2, 2, 2, 2, 2, 2, 2, 2, 2, 2, 2, 2, 2, 2, 2, 2, 2, 2, 2, 2, 2, 2, 2, 2, 2, 2, 2, 2, 2, 2, 2, 2, 2, 2, 2, 2, 2, 2, 2, 2, 2, 2, 2, 2, 2, 2, 2, 2, 2, 2, 2, 2, 2, 2, 2, 2, 2, 2, 2, 2, 2, 2, 2, 2, 2, 2, 2, 2, 2, 2, 2, 2, 2, 2, 2, 2, 2, 2, 2, 2, 2, 2, 2, 2, 2, 2, 2, 2, 2, 2, 2, 2, 2, 2, 2, 2, 2, 2, 2, 2, 2, 2, 2, 2, 2, 2, 2, 2, 2, 2, 2, 2, 2, 2, 2, 2, 2, 2, 2, 2, 2, 2, 2, 2, 2, 2, 2, 2, 2, 2, 2, 2, 2, 2, 2, 2, 2, 2, 2, 2, 2, 2, 2, 2, 2, 2, 2, 2, 2, 2, 2, 2, 2, 2, 2, 2, 2, 2, 2, 2, 2, 2, 2, 2, 2, 2, 2, 2, 2, 2, 2, 2, 2, 2, 2, 2, 2, 2, 2, 2, 2, 2, 2, 2, 2, 2, 2, 2, 2, 2, 2, 2, 2, 2, 2, 2, 2, 2, 2, 2, 2, 2, 3 ),
 ( 0.000000000000000000, 1.000000000000000000 ),
 ( 0.000000000000000000, 0.002777777777777777884, 0.005555555555555555768, 0.008333333333333333218, 0.01111111111111111154, 0.01388888888888888812, 0.01666666666666666644, 0.01944444444444444475, 0.02222222222222222307, 0.02500000000000000139, 0.02777777777777777624, 0.03055555555555555455, 0.03333333333333333287, 0.03611111111111110772, 0.03888888888888888951, 0.04166666666666666435, 0.04444444444444444614, 0.04722222222222222099, 0.05000000000000000278, 0.05277777777777777762, 0.05555555555555555247, 0.05833333333333333426, 0.06111111111111110911, 0.06388888888888888395, 0.06666666666666666574, 0.06944444444444444753, 0.07222222222222221544, 0.07499999999999999722, 0.07777777777777777901, 0.08055555555555556080, 0.08333333333333332871, 0.08611111111111111049, 0.08888888888888889228, 0.09166666666666666019, 0.09444444444444444198, 0.09722222222222222376, 0.1000000000000000056, 0.1027777777777777735, 0.1055555555555555552, 0.1083333333333333370, 0.1111111111111111049, 0.1138888888888888867, 0.1166666666666666685, 0.1194444444444444503, 0.1222222222222222182, 0.1250000000000000000, 0.1277777777777777679, 0.1305555555555555636, 0.1333333333333333315, 0.1361111111111110994, 0.1388888888888888951, 0.1416666666666666630, 0.1444444444444444309, 0.1472222222222222265, 0.1499999999999999944, 0.1527777777777777901, 0.1555555555555555580, 0.1583333333333333259, 0.1611111111111111216, 0.1638888888888888895, 0.1666666666666666574, 0.1694444444444444531, 0.1722222222222222210, 0.1749999999999999889, 0.1777777777777777846, 0.1805555555555555525, 0.1833333333333333204, 0.1861111111111111160, 0.1888888888888888840, 0.1916666666666666796, 0.1944444444444444475, 0.1972222222222222154, 0.2000000000000000111, 0.2027777777777777790, 0.2055555555555555469, 0.2083333333333333426, 0.2111111111111111105, 0.2138888888888888784, 0.2166666666666666741, 0.2194444444444444420, 0.2222222222222222099, 0.2250000000000000056, 0.2277777777777777735, 0.2305555555555555691, 0.2333333333333333370, 0.2361111111111111049, 0.2388888888888889006, 0.2416666666666666685, 0.2444444444444444364, 0.2472222222222222321, 0.2500000000000000000, 0.2527777777777777679, 0.2555555555555555358, 0.2583333333333333592, 0.2611111111111111271, 0.2638888888888888951, 0.2666666666666666630, 0.2694444444444444309, 0.2722222222222221988, 0.2750000000000000222, 0.2777777777777777901, 0.2805555555555555580, 0.2833333333333333259, 0.2861111111111110938, 0.2888888888888888618, 0.2916666666666666852, 0.2944444444444444531, 0.2972222222222222210, 0.2999999999999999889, 0.3027777777777777568, 0.3055555555555555802, 0.3083333333333333481, 0.3111111111111111160, 0.3138888888888888840, 0.3166666666666666519, 0.3194444444444444198, 0.3222222222222222432, 0.3250000000000000111, 0.3277777777777777790, 0.3305555555555555469, 0.3333333333333333148, 0.3361111111111111382, 0.3388888888888889062, 0.3416666666666666741, 0.3444444444444444420, 0.3472222222222222099, 0.3499999999999999778, 0.3527777777777778012, 0.3555555555555555691, 0.3583333333333333370, 0.3611111111111111049, 0.3638888888888888729, 0.3666666666666666408, 0.3694444444444444642, 0.3722222222222222321, 0.3750000000000000000, 0.3777777777777777679, 0.3805555555555555358, 0.3833333333333333592, 0.3861111111111111271, 0.3888888888888888951, 0.3916666666666666630, 0.3944444444444444309, 0.3972222222222221988, 0.4000000000000000222, 0.4027777777777777901, 0.4055555555555555580, 0.4083333333333333259, 0.4111111111111110938, 0.4138888888888888618, 0.4166666666666666852, 0.4194444444444444531, 0.4222222222222222210, 0.4249999999999999889, 0.4277777777777777568, 0.4305555555555555802, 0.4333333333333333481, 0.4361111111111111160, 0.4388888888888888840, 0.4416666666666666519, 0.4444444444444444198, 0.4472222222222222432, 0.4500000000000000111, 0.4527777777777777790, 0.4555555555555555469, 0.4583333333333333148, 0.4611111111111111382, 0.4638888888888889062, 0.4666666666666666741, 0.4694444444444444420, 0.4722222222222222099, 0.4749999999999999778, 0.4777777777777778012, 0.4805555555555555691, 0.4833333333333333370, 0.4861111111111111049, 0.4888888888888888729, 0.4916666666666666408, 0.4944444444444444642, 0.4972222222222222321, 0.5000000000000000000, 0.5027777777777777679, 0.5055555555555555358, 0.5083333333333333037, 0.5111111111111110716, 0.5138888888888888395, 0.5166666666666667185, 0.5194444444444444864, 0.5222222222222222543, 0.5250000000000000222, 0.5277777777777777901, 0.5305555555555555580, 0.5333333333333333259, 0.5361111111111110938, 0.5388888888888888618, 0.5416666666666666297, 0.5444444444444443976, 0.5472222222222222765, 0.5500000000000000444, 0.5527777777777778123, 0.5555555555555555802, 0.5583333333333333481, 0.5611111111111111160, 0.5638888888888888840, 0.5666666666666666519, 0.5694444444444444198, 0.5722222222222221877, 0.5749999999999999556, 0.5777777777777777235, 0.5805555555555556024, 0.5833333333333333703, 0.5861111111111111382, 0.5888888888888889062, 0.5916666666666666741, 0.5944444444444444420, 0.5972222222222222099, 0.5999999999999999778, 0.6027777777777777457, 0.6055555555555555136, 0.6083333333333332815, 0.6111111111111111605, 0.6138888888888889284, 0.6166666666666666963, 0.6194444444444444642, 0.6222222222222222321, 0.6250000000000000000, 0.6277777777777777679, 0.6305555555555555358, 0.6333333333333333037, 0.6361111111111110716, 0.6388888888888888395, 0.6416666666666667185, 0.6444444444444444864, 0.6472222222222222543, 0.6500000000000000222, 0.6527777777777777901, 0.6555555555555555580, 0.6583333333333333259, 0.6611111111111110938, 0.6638888888888888618, 0.6666666666666666297, 0.6694444444444443976, 0.6722222222222222765, 0.6750000000000000444, 0.6777777777777778123, 0.6805555555555555802, 0.6833333333333333481, 0.6861111111111111160, 0.6888888888888888840, 0.6916666666666666519, 0.6944444444444444198, 0.6972222222222221877, 0.6999999999999999556, 0.7027777777777777235, 0.7055555555555556024, 0.7083333333333333703, 0.7111111111111111382, 0.7138888888888889062, 0.7166666666666666741, 0.7194444444444444420, 0.7222222222222222099, 0.7249999999999999778, 0.7277777777777777457, 0.7305555555555555136, 0.7333333333333332815, 0.7361111111111111605, 0.7388888888888889284, 0.7416666666666666963, 0.7444444444444444642, 0.7472222222222222321, 0.7500000000000000000, 0.7527777777777777679, 0.7555555555555555358, 0.7583333333333333037, 0.7611111111111110716, 0.7638888888888888395, 0.7666666666666667185, 0.7694444444444444864, 0.7722222222222222543, 0.7750000000000000222, 0.7777777777777777901, 0.7805555555555555580, 0.7833333333333333259, 0.7861111111111110938, 0.7888888888888888618, 0.7916666666666666297, 0.7944444444444443976, 0.7972222222222222765, 0.8000000000000000444, 0.8027777777777778123, 0.8055555555555555802, 0.8083333333333333481, 0.8111111111111111160, 0.8138888888888888840, 0.8166666666666666519, 0.8194444444444444198, 0.8222222222222221877, 0.8249999999999999556, 0.8277777777777777235, 0.8305555555555556024, 0.8333333333333333703, 0.8361111111111111382, 0.8388888888888889062, 0.8416666666666666741, 0.8444444444444444420, 0.8472222222222222099, 0.8499999999999999778, 0.8527777777777777457, 0.8555555555555555136, 0.8583333333333332815, 0.8611111111111111605, 0.8638888888888889284, 0.8666666666666666963, 0.8694444444444444642, 0.8722222222222222321, 0.8750000000000000000, 0.8777777777777777679, 0.8805555555555555358, 0.8833333333333333037, 0.8861111111111110716, 0.8888888888888888395, 0.8916666666666667185, 0.8944444444444444864, 0.8972222222222222543, 0.9000000000000000222, 0.9027777777777777901, 0.9055555555555555580, 0.9083333333333333259, 0.9111111111111110938, 0.9138888888888888618, 0.9166666666666666297, 0.9194444444444443976, 0.9222222222222222765, 0.9250000000000000444, 0.9277777777777778123, 0.9305555555555555802, 0.9333333333333333481, 0.9361111111111111160, 0.9388888888888888840, 0.9416666666666666519, 0.9444444444444444198, 0.9472222222222221877, 0.9499999999999999556, 0.9527777777777777235, 0.9555555555555556024, 0.9583333333333333703, 0.9611111111111111382, 0.9638888888888889062, 0.9666666666666666741, 0.9694444444444444420, 0.9722222222222222099, 0.9749999999999999778, 0.9777777777777777457, 0.9805555555555555136, 0.9833333333333332815, 0.9861111111111111605, 0.9888888888888889284, 0.9916666666666666963, 0.9944444444444444642, 0.9972222222222222321, 1.000000000000000000 ),
 .UNSPECIFIED. ) 
 GEOMETRIC_REPRESENTATION_ITEM ( )  RATIONAL_B_SPLINE_SURFACE ( (
 ( 1.000000000000000000, 0.8660254037844387076, 1.000000000000000000, 0.8660254037844387076, 1.000000000000000000, 0.8660254037844387076, 1.000000000000000000, 0.8660254037844387076, 1.000000000000000000, 0.8660254037844387076, 1.000000000000000000, 0.8660254037844387076, 1.000000000000000000, 0.8660254037844387076, 1.000000000000000000, 0.8660254037844387076, 1.000000000000000000, 0.8660254037844387076, 1.000000000000000000, 0.8660254037844387076, 1.000000000000000000, 0.8660254037844387076, 1.000000000000000000, 0.8660254037844387076, 1.000000000000000000, 0.8660254037844387076, 1.000000000000000000, 0.8660254037844387076, 1.000000000000000000, 0.8660254037844387076, 1.000000000000000000, 0.8660254037844387076, 1.000000000000000000, 0.8660254037844387076, 1.000000000000000000, 0.8660254037844387076, 1.000000000000000000, 0.8660254037844387076, 1.000000000000000000, 0.8660254037844387076, 1.000000000000000000, 0.8660254037844387076, 1.000000000000000000, 0.8660254037844387076, 1.000000000000000000, 0.8660254037844387076, 1.000000000000000000, 0.8660254037844387076, 1.000000000000000000, 0.8660254037844387076, 1.000000000000000000, 0.8660254037844387076, 1.000000000000000000, 0.8660254037844387076, 1.000000000000000000, 0.8660254037844387076, 1.000000000000000000, 0.8660254037844387076, 1.000000000000000000, 0.8660254037844387076, 1.000000000000000000, 0.8660254037844387076, 1.000000000000000000, 0.8660254037844387076, 1.000000000000000000, 0.8660254037844387076, 1.000000000000000000, 0.8660254037844387076, 1.000000000000000000, 0.8660254037844387076, 1.000000000000000000, 0.8660254037844387076, 1.000000000000000000, 0.8660254037844387076, 1.000000000000000000, 0.8660254037844387076, 1.000000000000000000, 0.8660254037844387076, 1.000000000000000000, 0.8660254037844387076, 1.000000000000000000, 0.8660254037844387076, 1.000000000000000000, 0.8660254037844387076, 1.000000000000000000, 0.8660254037844387076, 1.000000000000000000, 0.8660254037844387076, 1.000000000000000000, 0.8660254037844387076, 1.000000000000000000, 0.8660254037844387076, 1.000000000000000000, 0.8660254037844387076, 1.000000000000000000, 0.8660254037844387076, 1.000000000000000000, 0.8660254037844387076, 1.000000000000000000, 0.8660254037844387076, 1.000000000000000000, 0.8660254037844387076, 1.000000000000000000, 0.8660254037844387076, 1.000000000000000000, 0.8660254037844387076, 1.000000000000000000, 0.8660254037844387076, 1.000000000000000000, 0.8660254037844387076, 1.000000000000000000, 0.8660254037844387076, 1.000000000000000000, 0.8660254037844387076, 1.000000000000000000, 0.8660254037844387076, 1.000000000000000000, 0.8660254037844387076, 1.000000000000000000, 0.8660254037844387076, 1.000000000000000000, 0.8660254037844387076, 1.000000000000000000, 0.8660254037844387076, 1.000000000000000000, 0.8660254037844387076, 1.000000000000000000, 0.8660254037844387076, 1.000000000000000000, 0.8660254037844387076, 1.000000000000000000, 0.8660254037844387076, 1.000000000000000000, 0.8660254037844387076, 1.000000000000000000, 0.8660254037844387076, 1.000000000000000000, 0.8660254037844387076, 1.000000000000000000, 0.8660254037844387076, 1.000000000000000000, 0.8660254037844387076, 1.000000000000000000, 0.8660254037844387076, 1.000000000000000000, 0.8660254037844387076, 1.000000000000000000, 0.8660254037844387076, 1.000000000000000000, 0.8660254037844387076, 1.000000000000000000, 0.8660254037844387076, 1.000000000000000000, 0.8660254037844387076, 1.000000000000000000, 0.8660254037844387076, 1.000000000000000000, 0.8660254037844387076, 1.000000000000000000, 0.8660254037844387076, 1.000000000000000000, 0.8660254037844387076, 1.000000000000000000, 0.8660254037844387076, 1.000000000000000000, 0.8660254037844387076, 1.000000000000000000, 0.8660254037844387076, 1.000000000000000000, 0.8660254037844387076, 1.000000000000000000, 0.8660254037844387076, 1.000000000000000000, 0.8660254037844387076, 1.000000000000000000, 0.8660254037844387076, 1.000000000000000000, 0.8660254037844387076, 1.000000000000000000, 0.8660254037844387076, 1.000000000000000000, 0.8660254037844387076, 1.000000000000000000, 0.8660254037844387076, 1.000000000000000000, 0.8660254037844387076, 1.000000000000000000, 0.8660254037844387076, 1.000000000000000000, 0.8660254037844387076, 1.000000000000000000, 0.8660254037844387076, 1.000000000000000000, 0.8660254037844387076, 1.000000000000000000, 0.8660254037844387076, 1.000000000000000000, 0.8660254037844387076, 1.000000000000000000, 0.8660254037844387076, 1.000000000000000000, 0.8660254037844387076, 1.000000000000000000, 0.8660254037844387076, 1.000000000000000000, 0.8660254037844387076, 1.000000000000000000, 0.8660254037844387076, 1.000000000000000000, 0.8660254037844387076, 1.000000000000000000, 0.8660254037844387076, 1.000000000000000000, 0.8660254037844387076, 1.000000000000000000, 0.8660254037844387076, 1.000000000000000000, 0.8660254037844387076, 1.000000000000000000, 0.8660254037844387076, 1.000000000000000000, 0.8660254037844387076, 1.000000000000000000, 0.8660254037844387076, 1.000000000000000000, 0.8660254037844387076, 1.000000000000000000, 0.8660254037844387076, 1.000000000000000000, 0.8660254037844387076, 1.000000000000000000, 0.8660254037844387076, 1.000000000000000000, 0.8660254037844387076, 1.000000000000000000, 0.8660254037844387076, 1.000000000000000000, 0.8660254037844387076, 1.000000000000000000, 0.8660254037844387076, 1.000000000000000000, 0.8660254037844387076, 1.000000000000000000, 0.8660254037844387076, 1.000000000000000000, 0.8660254037844387076, 1.000000000000000000, 0.8660254037844387076, 1.000000000000000000, 0.8660254037844387076, 1.000000000000000000, 0.8660254037844387076, 1.000000000000000000, 0.8660254037844387076, 1.000000000000000000, 0.8660254037844387076, 1.000000000000000000, 0.8660254037844387076, 1.000000000000000000, 0.8660254037844387076, 1.000000000000000000, 0.8660254037844387076, 1.000000000000000000, 0.8660254037844387076, 1.000000000000000000, 0.8660254037844387076, 1.000000000000000000, 0.8660254037844387076, 1.000000000000000000, 0.8660254037844387076, 1.000000000000000000, 0.8660254037844387076, 1.000000000000000000, 0.8660254037844387076, 1.000000000000000000, 0.8660254037844387076, 1.000000000000000000, 0.8660254037844387076, 1.000000000000000000, 0.8660254037844387076, 1.000000000000000000, 0.8660254037844387076, 1.000000000000000000, 0.8660254037844387076, 1.000000000000000000, 0.8660254037844387076, 1.000000000000000000, 0.8660254037844387076, 1.000000000000000000, 0.8660254037844387076, 1.000000000000000000, 0.8660254037844387076, 1.000000000000000000, 0.8660254037844387076, 1.000000000000000000, 0.8660254037844387076, 1.000000000000000000, 0.8660254037844387076, 1.000000000000000000, 0.8660254037844387076, 1.000000000000000000, 0.8660254037844387076, 1.000000000000000000, 0.8660254037844387076, 1.000000000000000000, 0.8660254037844387076, 1.000000000000000000, 0.8660254037844387076, 1.000000000000000000, 0.8660254037844387076, 1.000000000000000000, 0.8660254037844387076, 1.000000000000000000, 0.8660254037844387076, 1.000000000000000000, 0.8660254037844387076, 1.000000000000000000, 0.8660254037844387076, 1.000000000000000000, 0.8660254037844387076, 1.000000000000000000, 0.8660254037844387076, 1.000000000000000000, 0.8660254037844387076, 1.000000000000000000, 0.8660254037844387076, 1.000000000000000000, 0.8660254037844387076, 1.000000000000000000, 0.8660254037844387076, 1.000000000000000000, 0.8660254037844387076, 1.000000000000000000, 0.8660254037844387076, 1.000000000000000000, 0.8660254037844387076, 1.000000000000000000, 0.8660254037844387076, 1.000000000000000000, 0.8660254037844387076, 1.000000000000000000, 0.8660254037844387076, 1.000000000000000000, 0.8660254037844387076, 1.000000000000000000, 0.8660254037844387076, 1.000000000000000000, 0.8660254037844387076, 1.000000000000000000, 0.8660254037844387076, 1.000000000000000000, 0.8660254037844387076, 1.000000000000000000, 0.8660254037844387076, 1.000000000000000000, 0.8660254037844387076, 1.000000000000000000, 0.8660254037844387076, 1.000000000000000000, 0.8660254037844387076, 1.000000000000000000, 0.8660254037844387076, 1.000000000000000000, 0.8660254037844387076, 1.000000000000000000, 0.8660254037844387076, 1.000000000000000000, 0.8660254037844387076, 1.000000000000000000, 0.8660254037844387076, 1.000000000000000000, 0.8660254037844387076, 1.000000000000000000, 0.8660254037844387076, 1.000000000000000000, 0.8660254037844387076, 1.000000000000000000, 0.8660254037844387076, 1.000000000000000000, 0.8660254037844387076, 1.000000000000000000, 0.8660254037844387076, 1.000000000000000000, 0.8660254037844387076, 1.000000000000000000, 0.8660254037844387076, 1.000000000000000000, 0.8660254037844387076, 1.000000000000000000, 0.8660254037844387076, 1.000000000000000000, 0.8660254037844387076, 1.000000000000000000, 0.8660254037844387076, 1.000000000000000000, 0.8660254037844387076, 1.000000000000000000, 0.8660254037844387076, 1.000000000000000000, 0.8660254037844387076, 1.000000000000000000, 0.8660254037844387076, 1.000000000000000000, 0.8660254037844387076, 1.000000000000000000, 0.8660254037844387076, 1.000000000000000000, 0.8660254037844387076, 1.000000000000000000, 0.8660254037844387076, 1.000000000000000000, 0.8660254037844387076, 1.000000000000000000, 0.8660254037844387076, 1.000000000000000000, 0.8660254037844387076, 1.000000000000000000, 0.8660254037844387076, 1.000000000000000000, 0.8660254037844387076, 1.000000000000000000, 0.8660254037844387076, 1.000000000000000000, 0.8660254037844387076, 1.000000000000000000, 0.8660254037844387076, 1.000000000000000000, 0.8660254037844387076, 1.000000000000000000, 0.8660254037844387076, 1.000000000000000000, 0.8660254037844387076, 1.000000000000000000, 0.8660254037844387076, 1.000000000000000000, 0.8660254037844387076, 1.000000000000000000, 0.8660254037844387076, 1.000000000000000000, 0.8660254037844387076, 1.000000000000000000, 0.8660254037844387076, 1.000000000000000000, 0.8660254037844387076, 1.000000000000000000, 0.8660254037844387076, 1.000000000000000000, 0.8660254037844387076, 1.000000000000000000, 0.8660254037844387076, 1.000000000000000000, 0.8660254037844387076, 1.000000000000000000, 0.8660254037844387076, 1.000000000000000000, 0.8660254037844387076, 1.000000000000000000, 0.8660254037844387076, 1.000000000000000000, 0.8660254037844387076, 1.000000000000000000, 0.8660254037844387076, 1.000000000000000000, 0.8660254037844387076, 1.000000000000000000, 0.8660254037844387076, 1.000000000000000000, 0.8660254037844387076, 1.000000000000000000, 0.8660254037844387076, 1.000000000000000000, 0.8660254037844387076, 1.000000000000000000, 0.8660254037844387076, 1.000000000000000000, 0.8660254037844387076, 1.000000000000000000, 0.8660254037844387076, 1.000000000000000000, 0.8660254037844387076, 1.000000000000000000, 0.8660254037844387076, 1.000000000000000000, 0.8660254037844387076, 1.000000000000000000, 0.8660254037844387076, 1.000000000000000000, 0.8660254037844387076, 1.000000000000000000, 0.8660254037844387076, 1.000000000000000000, 0.8660254037844387076, 1.000000000000000000, 0.8660254037844387076, 1.000000000000000000, 0.8660254037844387076, 1.000000000000000000, 0.8660254037844387076, 1.000000000000000000, 0.8660254037844387076, 1.000000000000000000, 0.8660254037844387076, 1.000000000000000000, 0.8660254037844387076, 1.000000000000000000, 0.8660254037844387076, 1.000000000000000000, 0.8660254037844387076, 1.000000000000000000, 0.8660254037844387076, 1.000000000000000000, 0.8660254037844387076, 1.000000000000000000, 0.8660254037844387076, 1.000000000000000000, 0.8660254037844387076, 1.000000000000000000, 0.8660254037844387076, 1.000000000000000000, 0.8660254037844387076, 1.000000000000000000, 0.8660254037844387076, 1.000000000000000000, 0.8660254037844387076, 1.000000000000000000, 0.8660254037844387076, 1.000000000000000000, 0.8660254037844387076, 1.000000000000000000, 0.8660254037844387076, 1.000000000000000000, 0.8660254037844387076, 1.000000000000000000, 0.8660254037844387076, 1.000000000000000000, 0.8660254037844387076, 1.000000000000000000, 0.8660254037844387076, 1.000000000000000000, 0.8660254037844387076, 1.000000000000000000, 0.8660254037844387076, 1.000000000000000000, 0.8660254037844387076, 1.000000000000000000, 0.8660254037844387076, 1.000000000000000000, 0.8660254037844387076, 1.000000000000000000, 0.8660254037844387076, 1.000000000000000000, 0.8660254037844387076, 1.000000000000000000, 0.8660254037844387076, 1.000000000000000000, 0.8660254037844387076, 1.000000000000000000, 0.8660254037844387076, 1.000000000000000000, 0.8660254037844387076, 1.000000000000000000, 0.8660254037844387076, 1.000000000000000000, 0.8660254037844387076, 1.000000000000000000, 0.8660254037844387076, 1.000000000000000000, 0.8660254037844387076, 1.000000000000000000, 0.8660254037844387076, 1.000000000000000000, 0.8660254037844387076, 1.000000000000000000, 0.8660254037844387076, 1.000000000000000000, 0.8660254037844387076, 1.000000000000000000, 0.8660254037844387076, 1.000000000000000000, 0.8660254037844387076, 1.000000000000000000, 0.8660254037844387076, 1.000000000000000000, 0.8660254037844387076, 1.000000000000000000, 0.8660254037844387076, 1.000000000000000000, 0.8660254037844387076, 1.000000000000000000, 0.8660254037844387076, 1.000000000000000000, 0.8660254037844387076, 1.000000000000000000, 0.8660254037844387076, 1.000000000000000000, 0.8660254037844387076, 1.000000000000000000, 0.8660254037844387076, 1.000000000000000000, 0.8660254037844387076, 1.000000000000000000, 0.8660254037844387076, 1.000000000000000000, 0.8660254037844387076, 1.000000000000000000, 0.8660254037844387076, 1.000000000000000000, 0.8660254037844387076, 1.000000000000000000, 0.8660254037844387076, 1.000000000000000000, 0.8660254037844387076, 1.000000000000000000, 0.8660254037844387076, 1.000000000000000000, 0.8660254037844387076, 1.000000000000000000, 0.8660254037844387076, 1.000000000000000000, 0.8660254037844387076, 1.000000000000000000, 0.8660254037844387076, 1.000000000000000000, 0.8660254037844387076, 1.000000000000000000, 0.8660254037844387076, 1.000000000000000000, 0.8660254037844387076, 1.000000000000000000, 0.8660254037844387076, 1.000000000000000000, 0.8660254037844387076, 1.000000000000000000, 0.8660254037844387076, 1.000000000000000000, 0.8660254037844387076, 1.000000000000000000, 0.8660254037844387076, 1.000000000000000000, 0.8660254037844387076, 1.000000000000000000, 0.8660254037844387076, 1.000000000000000000, 0.8660254037844387076, 1.000000000000000000, 0.8660254037844387076, 1.000000000000000000, 0.8660254037844387076, 1.000000000000000000, 0.8660254037844387076, 1.000000000000000000, 0.8660254037844387076, 1.000000000000000000, 0.8660254037844387076, 1.000000000000000000, 0.8660254037844387076, 1.000000000000000000, 0.8660254037844387076, 1.000000000000000000, 0.8660254037844387076, 1.000000000000000000, 0.8660254037844387076, 1.000000000000000000, 0.8660254037844387076, 1.000000000000000000, 0.8660254037844387076, 1.000000000000000000, 0.8660254037844387076, 1.000000000000000000, 0.8660254037844387076, 1.000000000000000000, 0.8660254037844387076, 1.000000000000000000, 0.8660254037844387076, 1.000000000000000000, 0.8660254037844387076, 1.000000000000000000, 0.8660254037844387076, 1.000000000000000000, 0.8660254037844387076, 1.000000000000000000, 0.8660254037844387076, 1.000000000000000000, 0.8660254037844387076, 1.000000000000000000, 0.8660254037844387076, 1.000000000000000000, 0.8660254037844387076, 1.000000000000000000, 0.8660254037844387076, 1.000000000000000000, 0.8660254037844387076, 1.000000000000000000, 0.8660254037844387076, 1.000000000000000000, 0.8660254037844387076, 1.000000000000000000, 0.8660254037844387076, 1.000000000000000000, 0.8660254037844387076, 1.000000000000000000, 0.8660254037844387076, 1.000000000000000000, 0.8660254037844387076, 1.000000000000000000, 0.8660254037844387076, 1.000000000000000000, 0.8660254037844387076, 1.000000000000000000, 0.8660254037844387076, 1.000000000000000000, 0.8660254037844387076, 1.000000000000000000, 0.8660254037844387076, 1.000000000000000000, 0.8660254037844387076, 1.000000000000000000, 0.8660254037844387076, 1.000000000000000000, 0.8660254037844387076, 1.000000000000000000),
 ( 1.000000000000000000, 0.8660254037844387076, 1.000000000000000000, 0.8660254037844387076, 1.000000000000000000, 0.8660254037844387076, 1.000000000000000000, 0.8660254037844387076, 1.000000000000000000, 0.8660254037844387076, 1.000000000000000000, 0.8660254037844387076, 1.000000000000000000, 0.8660254037844387076, 1.000000000000000000, 0.8660254037844387076, 1.000000000000000000, 0.8660254037844387076, 1.000000000000000000, 0.8660254037844387076, 1.000000000000000000, 0.8660254037844387076, 1.000000000000000000, 0.8660254037844387076, 1.000000000000000000, 0.8660254037844387076, 1.000000000000000000, 0.8660254037844387076, 1.000000000000000000, 0.8660254037844387076, 1.000000000000000000, 0.8660254037844387076, 1.000000000000000000, 0.8660254037844387076, 1.000000000000000000, 0.8660254037844387076, 1.000000000000000000, 0.8660254037844387076, 1.000000000000000000, 0.8660254037844387076, 1.000000000000000000, 0.8660254037844387076, 1.000000000000000000, 0.8660254037844387076, 1.000000000000000000, 0.8660254037844387076, 1.000000000000000000, 0.8660254037844387076, 1.000000000000000000, 0.8660254037844387076, 1.000000000000000000, 0.8660254037844387076, 1.000000000000000000, 0.8660254037844387076, 1.000000000000000000, 0.8660254037844387076, 1.000000000000000000, 0.8660254037844387076, 1.000000000000000000, 0.8660254037844387076, 1.000000000000000000, 0.8660254037844387076, 1.000000000000000000, 0.8660254037844387076, 1.000000000000000000, 0.8660254037844387076, 1.000000000000000000, 0.8660254037844387076, 1.000000000000000000, 0.8660254037844387076, 1.000000000000000000, 0.8660254037844387076, 1.000000000000000000, 0.8660254037844387076, 1.000000000000000000, 0.8660254037844387076, 1.000000000000000000, 0.8660254037844387076, 1.000000000000000000, 0.8660254037844387076, 1.000000000000000000, 0.8660254037844387076, 1.000000000000000000, 0.8660254037844387076, 1.000000000000000000, 0.8660254037844387076, 1.000000000000000000, 0.8660254037844387076, 1.000000000000000000, 0.8660254037844387076, 1.000000000000000000, 0.8660254037844387076, 1.000000000000000000, 0.8660254037844387076, 1.000000000000000000, 0.8660254037844387076, 1.000000000000000000, 0.8660254037844387076, 1.000000000000000000, 0.8660254037844387076, 1.000000000000000000, 0.8660254037844387076, 1.000000000000000000, 0.8660254037844387076, 1.000000000000000000, 0.8660254037844387076, 1.000000000000000000, 0.8660254037844387076, 1.000000000000000000, 0.8660254037844387076, 1.000000000000000000, 0.8660254037844387076, 1.000000000000000000, 0.8660254037844387076, 1.000000000000000000, 0.8660254037844387076, 1.000000000000000000, 0.8660254037844387076, 1.000000000000000000, 0.8660254037844387076, 1.000000000000000000, 0.8660254037844387076, 1.000000000000000000, 0.8660254037844387076, 1.000000000000000000, 0.8660254037844387076, 1.000000000000000000, 0.8660254037844387076, 1.000000000000000000, 0.8660254037844387076, 1.000000000000000000, 0.8660254037844387076, 1.000000000000000000, 0.8660254037844387076, 1.000000000000000000, 0.8660254037844387076, 1.000000000000000000, 0.8660254037844387076, 1.000000000000000000, 0.8660254037844387076, 1.000000000000000000, 0.8660254037844387076, 1.000000000000000000, 0.8660254037844387076, 1.000000000000000000, 0.8660254037844387076, 1.000000000000000000, 0.8660254037844387076, 1.000000000000000000, 0.8660254037844387076, 1.000000000000000000, 0.8660254037844387076, 1.000000000000000000, 0.8660254037844387076, 1.000000000000000000, 0.8660254037844387076, 1.000000000000000000, 0.8660254037844387076, 1.000000000000000000, 0.8660254037844387076, 1.000000000000000000, 0.8660254037844387076, 1.000000000000000000, 0.8660254037844387076, 1.000000000000000000, 0.8660254037844387076, 1.000000000000000000, 0.8660254037844387076, 1.000000000000000000, 0.8660254037844387076, 1.000000000000000000, 0.8660254037844387076, 1.000000000000000000, 0.8660254037844387076, 1.000000000000000000, 0.8660254037844387076, 1.000000000000000000, 0.8660254037844387076, 1.000000000000000000, 0.8660254037844387076, 1.000000000000000000, 0.8660254037844387076, 1.000000000000000000, 0.8660254037844387076, 1.000000000000000000, 0.8660254037844387076, 1.000000000000000000, 0.8660254037844387076, 1.000000000000000000, 0.8660254037844387076, 1.000000000000000000, 0.8660254037844387076, 1.000000000000000000, 0.8660254037844387076, 1.000000000000000000, 0.8660254037844387076, 1.000000000000000000, 0.8660254037844387076, 1.000000000000000000, 0.8660254037844387076, 1.000000000000000000, 0.8660254037844387076, 1.000000000000000000, 0.8660254037844387076, 1.000000000000000000, 0.8660254037844387076, 1.000000000000000000, 0.8660254037844387076, 1.000000000000000000, 0.8660254037844387076, 1.000000000000000000, 0.8660254037844387076, 1.000000000000000000, 0.8660254037844387076, 1.000000000000000000, 0.8660254037844387076, 1.000000000000000000, 0.8660254037844387076, 1.000000000000000000, 0.8660254037844387076, 1.000000000000000000, 0.8660254037844387076, 1.000000000000000000, 0.8660254037844387076, 1.000000000000000000, 0.8660254037844387076, 1.000000000000000000, 0.8660254037844387076, 1.000000000000000000, 0.8660254037844387076, 1.000000000000000000, 0.8660254037844387076, 1.000000000000000000, 0.8660254037844387076, 1.000000000000000000, 0.8660254037844387076, 1.000000000000000000, 0.8660254037844387076, 1.000000000000000000, 0.8660254037844387076, 1.000000000000000000, 0.8660254037844387076, 1.000000000000000000, 0.8660254037844387076, 1.000000000000000000, 0.8660254037844387076, 1.000000000000000000, 0.8660254037844387076, 1.000000000000000000, 0.8660254037844387076, 1.000000000000000000, 0.8660254037844387076, 1.000000000000000000, 0.8660254037844387076, 1.000000000000000000, 0.8660254037844387076, 1.000000000000000000, 0.8660254037844387076, 1.000000000000000000, 0.8660254037844387076, 1.000000000000000000, 0.8660254037844387076, 1.000000000000000000, 0.8660254037844387076, 1.000000000000000000, 0.8660254037844387076, 1.000000000000000000, 0.8660254037844387076, 1.000000000000000000, 0.8660254037844387076, 1.000000000000000000, 0.8660254037844387076, 1.000000000000000000, 0.8660254037844387076, 1.000000000000000000, 0.8660254037844387076, 1.000000000000000000, 0.8660254037844387076, 1.000000000000000000, 0.8660254037844387076, 1.000000000000000000, 0.8660254037844387076, 1.000000000000000000, 0.8660254037844387076, 1.000000000000000000, 0.8660254037844387076, 1.000000000000000000, 0.8660254037844387076, 1.000000000000000000, 0.8660254037844387076, 1.000000000000000000, 0.8660254037844387076, 1.000000000000000000, 0.8660254037844387076, 1.000000000000000000, 0.8660254037844387076, 1.000000000000000000, 0.8660254037844387076, 1.000000000000000000, 0.8660254037844387076, 1.000000000000000000, 0.8660254037844387076, 1.000000000000000000, 0.8660254037844387076, 1.000000000000000000, 0.8660254037844387076, 1.000000000000000000, 0.8660254037844387076, 1.000000000000000000, 0.8660254037844387076, 1.000000000000000000, 0.8660254037844387076, 1.000000000000000000, 0.8660254037844387076, 1.000000000000000000, 0.8660254037844387076, 1.000000000000000000, 0.8660254037844387076, 1.000000000000000000, 0.8660254037844387076, 1.000000000000000000, 0.8660254037844387076, 1.000000000000000000, 0.8660254037844387076, 1.000000000000000000, 0.8660254037844387076, 1.000000000000000000, 0.8660254037844387076, 1.000000000000000000, 0.8660254037844387076, 1.000000000000000000, 0.8660254037844387076, 1.000000000000000000, 0.8660254037844387076, 1.000000000000000000, 0.8660254037844387076, 1.000000000000000000, 0.8660254037844387076, 1.000000000000000000, 0.8660254037844387076, 1.000000000000000000, 0.8660254037844387076, 1.000000000000000000, 0.8660254037844387076, 1.000000000000000000, 0.8660254037844387076, 1.000000000000000000, 0.8660254037844387076, 1.000000000000000000, 0.8660254037844387076, 1.000000000000000000, 0.8660254037844387076, 1.000000000000000000, 0.8660254037844387076, 1.000000000000000000, 0.8660254037844387076, 1.000000000000000000, 0.8660254037844387076, 1.000000000000000000, 0.8660254037844387076, 1.000000000000000000, 0.8660254037844387076, 1.000000000000000000, 0.8660254037844387076, 1.000000000000000000, 0.8660254037844387076, 1.000000000000000000, 0.8660254037844387076, 1.000000000000000000, 0.8660254037844387076, 1.000000000000000000, 0.8660254037844387076, 1.000000000000000000, 0.8660254037844387076, 1.000000000000000000, 0.8660254037844387076, 1.000000000000000000, 0.8660254037844387076, 1.000000000000000000, 0.8660254037844387076, 1.000000000000000000, 0.8660254037844387076, 1.000000000000000000, 0.8660254037844387076, 1.000000000000000000, 0.8660254037844387076, 1.000000000000000000, 0.8660254037844387076, 1.000000000000000000, 0.8660254037844387076, 1.000000000000000000, 0.8660254037844387076, 1.000000000000000000, 0.8660254037844387076, 1.000000000000000000, 0.8660254037844387076, 1.000000000000000000, 0.8660254037844387076, 1.000000000000000000, 0.8660254037844387076, 1.000000000000000000, 0.8660254037844387076, 1.000000000000000000, 0.8660254037844387076, 1.000000000000000000, 0.8660254037844387076, 1.000000000000000000, 0.8660254037844387076, 1.000000000000000000, 0.8660254037844387076, 1.000000000000000000, 0.8660254037844387076, 1.000000000000000000, 0.8660254037844387076, 1.000000000000000000, 0.8660254037844387076, 1.000000000000000000, 0.8660254037844387076, 1.000000000000000000, 0.8660254037844387076, 1.000000000000000000, 0.8660254037844387076, 1.000000000000000000, 0.8660254037844387076, 1.000000000000000000, 0.8660254037844387076, 1.000000000000000000, 0.8660254037844387076, 1.000000000000000000, 0.8660254037844387076, 1.000000000000000000, 0.8660254037844387076, 1.000000000000000000, 0.8660254037844387076, 1.000000000000000000, 0.8660254037844387076, 1.000000000000000000, 0.8660254037844387076, 1.000000000000000000, 0.8660254037844387076, 1.000000000000000000, 0.8660254037844387076, 1.000000000000000000, 0.8660254037844387076, 1.000000000000000000, 0.8660254037844387076, 1.000000000000000000, 0.8660254037844387076, 1.000000000000000000, 0.8660254037844387076, 1.000000000000000000, 0.8660254037844387076, 1.000000000000000000, 0.8660254037844387076, 1.000000000000000000, 0.8660254037844387076, 1.000000000000000000, 0.8660254037844387076, 1.000000000000000000, 0.8660254037844387076, 1.000000000000000000, 0.8660254037844387076, 1.000000000000000000, 0.8660254037844387076, 1.000000000000000000, 0.8660254037844387076, 1.000000000000000000, 0.8660254037844387076, 1.000000000000000000, 0.8660254037844387076, 1.000000000000000000, 0.8660254037844387076, 1.000000000000000000, 0.8660254037844387076, 1.000000000000000000, 0.8660254037844387076, 1.000000000000000000, 0.8660254037844387076, 1.000000000000000000, 0.8660254037844387076, 1.000000000000000000, 0.8660254037844387076, 1.000000000000000000, 0.8660254037844387076, 1.000000000000000000, 0.8660254037844387076, 1.000000000000000000, 0.8660254037844387076, 1.000000000000000000, 0.8660254037844387076, 1.000000000000000000, 0.8660254037844387076, 1.000000000000000000, 0.8660254037844387076, 1.000000000000000000, 0.8660254037844387076, 1.000000000000000000, 0.8660254037844387076, 1.000000000000000000, 0.8660254037844387076, 1.000000000000000000, 0.8660254037844387076, 1.000000000000000000, 0.8660254037844387076, 1.000000000000000000, 0.8660254037844387076, 1.000000000000000000, 0.8660254037844387076, 1.000000000000000000, 0.8660254037844387076, 1.000000000000000000, 0.8660254037844387076, 1.000000000000000000, 0.8660254037844387076, 1.000000000000000000, 0.8660254037844387076, 1.000000000000000000, 0.8660254037844387076, 1.000000000000000000, 0.8660254037844387076, 1.000000000000000000, 0.8660254037844387076, 1.000000000000000000, 0.8660254037844387076, 1.000000000000000000, 0.8660254037844387076, 1.000000000000000000, 0.8660254037844387076, 1.000000000000000000, 0.8660254037844387076, 1.000000000000000000, 0.8660254037844387076, 1.000000000000000000, 0.8660254037844387076, 1.000000000000000000, 0.8660254037844387076, 1.000000000000000000, 0.8660254037844387076, 1.000000000000000000, 0.8660254037844387076, 1.000000000000000000, 0.8660254037844387076, 1.000000000000000000, 0.8660254037844387076, 1.000000000000000000, 0.8660254037844387076, 1.000000000000000000, 0.8660254037844387076, 1.000000000000000000, 0.8660254037844387076, 1.000000000000000000, 0.8660254037844387076, 1.000000000000000000, 0.8660254037844387076, 1.000000000000000000, 0.8660254037844387076, 1.000000000000000000, 0.8660254037844387076, 1.000000000000000000, 0.8660254037844387076, 1.000000000000000000, 0.8660254037844387076, 1.000000000000000000, 0.8660254037844387076, 1.000000000000000000, 0.8660254037844387076, 1.000000000000000000, 0.8660254037844387076, 1.000000000000000000, 0.8660254037844387076, 1.000000000000000000, 0.8660254037844387076, 1.000000000000000000, 0.8660254037844387076, 1.000000000000000000, 0.8660254037844387076, 1.000000000000000000, 0.8660254037844387076, 1.000000000000000000, 0.8660254037844387076, 1.000000000000000000, 0.8660254037844387076, 1.000000000000000000, 0.8660254037844387076, 1.000000000000000000, 0.8660254037844387076, 1.000000000000000000, 0.8660254037844387076, 1.000000000000000000, 0.8660254037844387076, 1.000000000000000000, 0.8660254037844387076, 1.000000000000000000, 0.8660254037844387076, 1.000000000000000000, 0.8660254037844387076, 1.000000000000000000, 0.8660254037844387076, 1.000000000000000000, 0.8660254037844387076, 1.000000000000000000, 0.8660254037844387076, 1.000000000000000000, 0.8660254037844387076, 1.000000000000000000, 0.8660254037844387076, 1.000000000000000000, 0.8660254037844387076, 1.000000000000000000, 0.8660254037844387076, 1.000000000000000000, 0.8660254037844387076, 1.000000000000000000, 0.8660254037844387076, 1.000000000000000000, 0.8660254037844387076, 1.000000000000000000, 0.8660254037844387076, 1.000000000000000000, 0.8660254037844387076, 1.000000000000000000, 0.8660254037844387076, 1.000000000000000000, 0.8660254037844387076, 1.000000000000000000, 0.8660254037844387076, 1.000000000000000000, 0.8660254037844387076, 1.000000000000000000, 0.8660254037844387076, 1.000000000000000000, 0.8660254037844387076, 1.000000000000000000, 0.8660254037844387076, 1.000000000000000000, 0.8660254037844387076, 1.000000000000000000, 0.8660254037844387076, 1.000000000000000000, 0.8660254037844387076, 1.000000000000000000, 0.8660254037844387076, 1.000000000000000000, 0.8660254037844387076, 1.000000000000000000, 0.8660254037844387076, 1.000000000000000000, 0.8660254037844387076, 1.000000000000000000, 0.8660254037844387076, 1.000000000000000000, 0.8660254037844387076, 1.000000000000000000, 0.8660254037844387076, 1.000000000000000000, 0.8660254037844387076, 1.000000000000000000, 0.8660254037844387076, 1.000000000000000000, 0.8660254037844387076, 1.000000000000000000, 0.8660254037844387076, 1.000000000000000000, 0.8660254037844387076, 1.000000000000000000, 0.8660254037844387076, 1.000000000000000000, 0.8660254037844387076, 1.000000000000000000, 0.8660254037844387076, 1.000000000000000000, 0.8660254037844387076, 1.000000000000000000, 0.8660254037844387076, 1.000000000000000000, 0.8660254037844387076, 1.000000000000000000, 0.8660254037844387076, 1.000000000000000000, 0.8660254037844387076, 1.000000000000000000, 0.8660254037844387076, 1.000000000000000000, 0.8660254037844387076, 1.000000000000000000, 0.8660254037844387076, 1.000000000000000000, 0.8660254037844387076, 1.000000000000000000, 0.8660254037844387076, 1.000000000000000000, 0.8660254037844387076, 1.000000000000000000, 0.8660254037844387076, 1.000000000000000000, 0.8660254037844387076, 1.000000000000000000, 0.8660254037844387076, 1.000000000000000000, 0.8660254037844387076, 1.000000000000000000, 0.8660254037844387076, 1.000000000000000000, 0.8660254037844387076, 1.000000000000000000, 0.8660254037844387076, 1.000000000000000000, 0.8660254037844387076, 1.000000000000000000, 0.8660254037844387076, 1.000000000000000000, 0.8660254037844387076, 1.000000000000000000, 0.8660254037844387076, 1.000000000000000000, 0.8660254037844387076, 1.000000000000000000, 0.8660254037844387076, 1.000000000000000000, 0.8660254037844387076, 1.000000000000000000) ) ) 
 REPRESENTATION_ITEM ( '' )  SURFACE ( )  );
#35409 = CARTESIAN_POINT ( 'NONE',  ( 3.871028493210608712, 25.03395833444976404, 31.04107391399921312 ) ) ;
#35410 = CARTESIAN_POINT ( 'NONE',  ( 5.887500000000000178, -2.886751345948125991, -5.000000000000000000 ) ) ;
#35411 = CARTESIAN_POINT ( 'NONE',  ( 26.62500000122903288, -5.773502691896255534, -1.060575238724906372E-15 ) ) ;
#35412 = CARTESIAN_POINT ( 'NONE',  ( 18.57187500061451857, -4.119189519843968306, 2.378215178124996054 ) ) ;
#35413 = CARTESIAN_POINT ( 'NONE',  ( 22.34062500061451573, -3.027376345333610441, -5.243569643749999898 ) ) ;
#35414 = CARTESIAN_POINT ( 'NONE',  ( 14.05312500061451431, 0.000000000000000000, 5.243569643749999010 ) ) ;
#35415 = CARTESIAN_POINT ( 'NONE',  ( 25.95937500061451431, 2.746126346562645981, -4.756430356249997438 ) ) ;
#35416 = CARTESIAN_POINT ( 'NONE',  ( 8.709375000614517859, 0.000000000000000000, 5.243569643749999010 ) ) ;
#35417 = CARTESIAN_POINT ( 'NONE',  ( 26.39999999999999858, 0.000000000000000000, 4.999999999999998224 ) ) ;
#35418 = CARTESIAN_POINT ( 'NONE',  ( 23.21250000122903501, 4.330127018922192761, -2.499999999999997780 ) ) ;
#35419 = CARTESIAN_POINT ( 'NONE',  ( 8.062500001229034652, 0.000000000000000000, 4.999999999999998224 ) ) ;
#35420 = CARTESIAN_POINT ( 'NONE',  ( 11.22187500061451892, 3.027376345333613106, -5.243569643749998122 ) ) ;
#35421 = CARTESIAN_POINT ( 'NONE',  ( 26.48437500061451644, 6.421520780324663323E-16, -5.243569643749999010 ) ) ;
#35422 = CARTESIAN_POINT ( 'NONE',  ( 3.159375000614518036, 4.541064518000418104, -2.621784821874998173 ) ) ;
#35423 = CYLINDRICAL_SURFACE ( 'NONE', #66752, 1.499999999999999556 ) ;
#35424 = CARTESIAN_POINT ( 'NONE',  ( 22.20937500061451431, 0.000000000000000000, 5.243569643749999010 ) ) ;
#35425 = CARTESIAN_POINT ( 'NONE',  ( 12.72187500061451537, 3.027376345333611329, 5.243569643749999010 ) ) ;
#35426 = CARTESIAN_POINT ( 'NONE',  ( -1.878215178125001827, 19.35312499938548214, 33.25316411605952283 ) ) ;
#35427 = CARTESIAN_POINT ( 'NONE',  ( 24.75000000000000000, -4.330127018922190985, -2.500000000000001332 ) ) ;
#35428 = CARTESIAN_POINT ( 'NONE',  ( -1.878215178125001827, 20.14062499938548356, 33.25316411605952283 ) ) ;
#35429 = CARTESIAN_POINT ( 'NONE',  ( 2.121784821874999061, 12.05937500061451750, -33.67503911421598417 ) ) ;
#35430 = CARTESIAN_POINT ( 'NONE',  ( 27.04687500061451644, 5.492252693125287522, 3.363034840372157021E-16 ) ) ;
#35431 = CARTESIAN_POINT ( 'NONE',  ( 14.16562500061451679, -6.054752690667223547, -1.112240025338166033E-15 ) ) ;
#35432 = CARTESIAN_POINT ( 'NONE',  ( 6.975000000000002309, 4.330127018922191873, 2.499999999999999556 ) ) ;
#35433 = DIRECTION ( 'NONE',  ( -1.000000000000000000, -0.000000000000000000, -0.000000000000000000 ) ) ;
#35434 = CARTESIAN_POINT ( 'NONE',  ( 14.10000000000000142, 4.330127018922192761, -2.499999999999997780 ) ) ;
#35435 = CARTESIAN_POINT ( 'NONE',  ( 8.484601909799253346E-16, 19.32500000122902861, 34.61880215351700230 ) ) ;
#35436 = CARTESIAN_POINT ( 'NONE',  ( 14.85000000122903252, -2.886751345948129988, 4.999999999999997335 ) ) ;
#35437 = CARTESIAN_POINT ( 'NONE',  ( 24.53437500061451715, -4.541064518000419881, 2.621784821874995952 ) ) ;
#35438 = VERTEX_POINT ( 'NONE', #61755 ) ;
#35439 = CARTESIAN_POINT ( 'NONE',  ( 20.65312500061451573, 4.541064518000418104, -2.621784821874998173 ) ) ;
#35440 = CARTESIAN_POINT ( 'NONE',  ( 19.77187500061451786, 3.027376345333613106, -5.243569643749998122 ) ) ;
#35441 = CARTESIAN_POINT ( 'NONE',  ( 5.100000000000000533, 4.330127018922192761, -2.499999999999997780 ) ) ;
#35442 = CARTESIAN_POINT ( 'NONE',  ( 7.678125000614516082, 4.541064518000418104, 2.621784821874999949 ) ) ;
#35443 = CARTESIAN_POINT ( 'NONE',  ( 22.45312500061451644, 4.541064518000418104, -2.621784821874998173 ) ) ;
#35444 = CARTESIAN_POINT ( 'NONE',  ( 11.93437500061451573, -4.541064518000419881, 2.621784821874995952 ) ) ;
#35445 = CARTESIAN_POINT ( 'NONE',  ( 16.62187500061451573, 3.027376345333613106, -5.243569643749998122 ) ) ;
#35446 = CARTESIAN_POINT ( 'NONE',  ( -2.121784821874996840, 15.37812500061451892, 33.67503911421598417 ) ) ;
#35447 = CARTESIAN_POINT ( 'NONE',  ( 18.82500000122903216, 2.886751345948126879, 4.999999999999999112 ) ) ;
#35448 = CARTESIAN_POINT ( 'NONE',  ( 11.33437500061451608, 4.119189519843966529, 2.378215178124999607 ) ) ;
#35449 = CARTESIAN_POINT ( 'NONE',  ( 8.465625000614515727, 3.027376345333612662, -5.243569643749998122 ) ) ;
#35450 = CARTESIAN_POINT ( 'NONE',  ( 3.646875000614520079, 6.054752690667223547, 3.707466751127219781E-16 ) ) ;
#35451 = CARTESIAN_POINT ( 'NONE',  ( 28.49062500061451431, -3.027376345333614438, 5.243569643749998122 ) ) ;
#35452 = CARTESIAN_POINT ( 'NONE',  ( 24.94687500061451502, -3.027376345333614438, 5.243569643749998122 ) ) ;
#35453 = CARTESIAN_POINT ( 'NONE',  ( 18.06562500061451715, 3.027376345333611329, 5.243569643749999010 ) ) ;
#35454 = CARTESIAN_POINT ( 'NONE',  ( 25.23750000122903359, -4.330127018922194537, 2.499999999999995559 ) ) ;
#35455 = EDGE_CURVE ( 'NONE', #69491, #46824, #62233, .T. ) ;
#35456 = CARTESIAN_POINT ( 'NONE',  ( 26.31562500061451715, -6.054752690667223547, -1.112240025338166033E-15 ) ) ;
#35457 = CARTESIAN_POINT ( 'NONE',  ( 21.38437500061451502, -4.541064518000419881, 2.621784821874995952 ) ) ;
#35458 = CARTESIAN_POINT ( 'NONE',  ( 15.44062500061451537, -3.027376345333614438, 5.243569643749998122 ) ) ;
#35459 = CARTESIAN_POINT ( 'NONE',  ( 4.243569643749999010, 17.87187500061451573, 27.54997392385601174 ) ) ;
#35460 = EDGE_CURVE ( 'NONE', #61955, #4995, #68763, .T. ) ;
#35461 = CARTESIAN_POINT ( 'NONE',  ( 22.04062500061451502, 6.054752690667223547, 3.707466751127219781E-16 ) ) ;
#35462 = CARTESIAN_POINT ( 'NONE',  ( 3.375000001229033320, 2.886751345948129099, -4.999999999999998224 ) ) ;
#35463 = VERTEX_POINT ( 'NONE', #40686 ) ;
#35464 = CARTESIAN_POINT ( 'NONE',  ( 25.68750000000000000, -2.886751345948125991, -5.000000000000000000 ) ) ;
#35465 = CARTESIAN_POINT ( 'NONE',  ( 4.000000000000000000, 13.88750000000000107, -27.69059892324149530 ) ) ;
#35466 = CARTESIAN_POINT ( 'NONE',  ( 3.756430356249998770, 19.46562499938548285, 32.16877607737302469 ) ) ;
#35467 = CARTESIAN_POINT ( 'NONE',  ( 28.97812500061451502, -4.541064518000419881, 2.621784821874995952 ) ) ;
#35468 = CARTESIAN_POINT ( 'NONE',  ( 6.928125000614516082, -4.541064518000419881, 2.621784821874995952 ) ) ;
#35469 = CARTESIAN_POINT ( 'NONE',  ( 21.41250000122903074, 4.330127018922192761, -2.499999999999997780 ) ) ;
#35470 =( BOUNDED_SURFACE ( )  B_SPLINE_SURFACE ( 1, 2, ( 
 ( #58419, #21373, #24810, #15460, #65716, #2295, #9934, #60899, #52896, #43560, #38005, #60527, #32472, #43927, #32835, #7831, #32103, #66453, #4766, #31740, #55005, #4411, #47356, #30368, #27299, #41453, #49833, #69888, #54636, #48735, #26940, #4041, #19253, #41808, #65345, #63971, #14735, #49465, #15102, #13354, #71998, #35895, #54278, #59799, #37277, #9205, #26196, #26566, #18891, #3672, #71258, #20638, #37638, #43196, #60161, #9571, #49106, #71635, #21008, #15830, #66082, #38375, #10302, #33195, #61626, #57168, #10665, #5849, #55734, #33551, #45019, #39845, #45743, #39110, #17284, #56458, #682, #5128, #27662, #67197, #68278, #11028, #5492, #56101, #39472, #28031, #50560, #22110, #66828, #40200, #56805, #28380, #23189, #17640, #50201, #72726, #62722, #33915, #50918, #6580, #51279, #44667, #16200, #16559, #29111, #316, #12115, #73087, #45377, #67554, #22825, #61272, #22468, #16917, #61995, #11395, #67913, #34639, #62359, #11755, #72357, #21738, #44299, #34273, #6211, #28739, #38751, #35730, #57538, #69369, #8388, #46465, #52006, #7657, #52726, #30196, #58251, #47549, #12481, #42013, #57891, #46831, #69002, #52365, #18726, #35008, #58981, #13927, #36465, #63448, #24644, #7300, #58618, #41290, #12834, #30561, #64533, #51645, #23554, #53088, #47189, #1769, #6939, #69720, #29470, #1046, #46102, #23916, #18364, #1407, #29830, #40934, #63801, #41644, #19089, #24283, #35368, #68639, #13191, #2132, #18002, #2482, #64163, #13551, #36098, #40560, #8025, #63079, #25007, #70078, #19453, #20926, #60443, #14651, #49022, #26854, #36829, #3958, #54194, #59716, #15746, #15383, #37925, #70451, #59343, #71552, #43478, #20550, #3591, #49386, #2848, #32382, #42379, #26113, #26481, #43107, #64901, #53458, #66003, #38285, #54556, #9853, #25377, #54922, #60080, #4330, #71917, #21292, #43844, #66371, #60813, #48288, #65633, #47922, #15020, #30917, #19827, #65262, #3222, #9123, #37558, #14291, #8754, #31287, #20187, #53829, #25751, #37192, #70812, #42742, #31660, #48652, #71177, #9491, #32020, #66746, #238, #51198, #44214, #33838, #28303, #5772, #50838, #11676, #23106, #49751, #22389, #34192, #45663, #22027, #22746, #45296, #16116, #21656, #68196, #32755, #17559, #61192, #44938, #39031, #67830, #67476, #38668, #10586, #72279, #55292, #16473, #11317, #56016, #56726, #17203, #16839, #4686, #39764, #27216, #44584, #50115, #33113, #55651, #61545, #39393, #40120, #10221, #5047, #67116, #27946, #10947, #27583, #72644, #33469, #5409, #50479, #6128, #73005, #61912, #56380, #62281, #28659, #601, #962, #69277, #23472, #23827, #35281, #30103, #36004, #29387, #7567, #46743, #64074, #46018, #17913, #57449, #58523, #51921, #68912, #1318, #29741, #46378, #18270, #12386, #57083, #30471, #47101, #18639, #13456, #7933, #68555, #40476, #53000, #24189, #41203, #47458, #41557, #62991, #6491, #34922, #19361, #63711, #2395, #40843, #35641, #57803, #13103, #51562, #63361, #12745, #6853, #52278, #7212, #24916, #1680, #58163, #69991, #62635, #12030, #52638, #2044, #24555, #69633, #18995, #34555, #29026, #71830, #36735, #42285, #71088, #43016, #20462, #48562, #37833, #2760, #32296, #48195, #37098, #59256, #42650, #59623, #25282, #49297, #4238, #26765, #53737, #14932, #70718, #48932, #9037, #3130, #20837, #54831, #41918, #13835, #43390, #37472, #65174, #70358, #59992, #47828, #31932, #14565, #20093, #14199, #64443, #8300, #65914, #19735, #9402, #31567, #64809, #54469, #9762, #8664, #65545, #3867, #26390, #71461, #15294, #36374, #30830, #54106, #60353, #58890, #25659, #53363, #31195, #3504, #26023, #6040, #43753, #28574, #72190, #33388, #50026, #56294, #5320, #55205, #4598, #10132, #66278, #27492, #22300, #67027, #45208, #11225, #27862, #21569, #15656, #38195, #66650, #16027, #27128, #72551, #38575, #10854, #33749, #39307, #44494, #61099, #51111, #33025, #4959, #21201, #152, #55924, #61460, #21938, #56645, #10497, #11589, #55563, #50393, #50749, #5684, #22658, #16387, #61820, #17114, #49662, #67388, #38942, #72918, #60722, #28220, #67741, #32664, #44123, #39673, #62193, #44852, #16750, #34106, #45576, #1960, #11943, #23738, #69191, #12660, #34468, #23018, #18551, #7849, #24103, #58074, #68107, #30011, #29654, #24467, #7483, #63626, #13016, #41470, #47015, #17823, #35195, #17473, #63268, #35554, #52554, #34833, #45930, #51829, #57719, #41116, #46651, #874, #62903, #69550, #18909, #63990, #13372, #40033, #7124, #35913, #58438, #12298, #30385, #508, #56996, #6403, #62546, #28935, #51471, #23381, #52191, #29299, #68461, #1593, #40384, #57359, #6765, #1233, #46286, #68827, #18184, #40753, #42928, #37012, #30742, #2312, #47374, #25189, #47733, #58803, #8577, #70272, #42560, #65452, #71001, #3038, #19643, #37746, #64723, #36647, #52914, #31847, #65087, #20007, #31105, #15206, #42199, #43304, #14108, #14478, #9314, #14844, #54383, #59169, #20377, #48840, #8213, #25937, #25569, #53645, #60264, #37385, #59908, #19272, #53274, #3778, #26303, #59535, #48109, #71371, #24827, #20746, #64357, #70632, #48477, #8947, #13748, #69905, #65824, #9678, #3417, #41826, #36289, #2672, #31480, #54022, #39220, #22215, #44769, #67, #5598, #49575, #44409, #54745, #21846, #67304, #16662, #66556, #4515, #10408, #66935, #50310, #5229, #32578, #21482, #11133, #55841, #38485, #27044, #17022, #71745, #33661, #38111, #27770, #4870, #15569, #61732, #22573, #66191, #72832, #56205, #28135, #50663, #26679, #72097, #44034, #60632, #61009, #15936, #16304, #45121, #67656, #55478, #32940, #39581, #27406, #49937, #32211, #62105, #38858, #72461, #61373, #4147, #10770, #49211, #33303, #21115, #43668, #10044, #55116, #68378, #29569, #7399, #17389, #57633, #34741, #40298, #69466, #69105, #18467, #51021, #39946, #52105, #24014, #1147, #57271, #29927, #56557 ),
 ( #28843, #23656, #34020, #46200, #46563, #41030, #45842, #56909, #62820, #68741, #1510, #7039, #11857, #784, #63546, #35109, #17739, #6314, #18824, #417, #12932, #62459, #35467, #6682, #68016, #57989, #52467, #45484, #1874, #24380, #46928, #41387, #11498, #5951, #22926, #18099, #28484, #34376, #23293, #51382, #12212, #29210, #51746, #40660, #63180, #12575, #41740, #2952, #19558, #25854, #48026, #24743, #47287, #52828, #35826, #70180, #65004, #36564, #14754, #53933, #70552, #64268, #13289, #2230, #19927, #69821, #25104, #59084, #31393, #37298, #30656, #8857, #42481, #65365, #19187, #13657, #58717, #59821, #53188, #42114, #2585, #31021, #47648, #64638, #36199, #58349, #31763, #48391, #14392, #9226, #54300, #8129, #14024, #3692, #25480, #36929, #48756, #42844, #8488, #7760, #53555, #20657, #59450, #26217, #3328, #70919, #20289, #71280, #63899, #30296, #32489, #66101, #10319, #26585, #33569, #32122, #38768, #5509, #28047, #50576, #21754, #32851, #72374, #10680, #27316, #49125, #60916, #73103, #38023, #43580, #44315, #66845, #16215, #49848, #39126, #4059, #56117, #49483, #38392, #60546, #43946, #55388, #71654, #43216, #65736, #15121, #55024, #61287, #72014, #50216, #4782, #4427, #22127, #37658, #60181, #9590, #44682, #33210, #66469, #21027, #55749, #15479, #5143, #15846, #54656, #72741, #9953, #26956, #21390, #27678, #67213, #16574, #61641, #11043, #30842, #68925, #57815, #41215, #7225, #46390, #18281, #63374, #40857, #12399, #24928, #29754, #53376, #22485, #57461, #12758, #8313, #67570, #53013, #52650, #47471, #30484, #13469, #36017, #64456, #70003, #35294, #35655, #45035, #13115, #58535, #7947, #52291, #1692, #24202, #58175, #41569, #69645, #23842, #46755, #2407, #47113, #69290, #18653, #16935, #62012, #19373, #29399, #19007, #63723, #6867, #41930, #13847, #51933, #64087, #36388, #58901, #39490, #34935, #1330, #7580, #30115, #2056, #24568, #14577, #43402, #37845, #36748, #14211, #60736, #25295, #10145, #53748, #14946, #31580, #60366, #60005, #59268, #8676, #64822, #47841, #9049, #3881, #48574, #26777, #65927, #9415, #3145, #70370, #19748, #48208, #70730, #31208, #54119, #20107, #65556, #15307, #20850, #26036, #42662, #32678, #37110, #59636, #2772, #54843, #37484, #43028, #3515, #38208, #65187, #66291, #71102, #31945, #32309, #9775, #4252, #20475, #49309, #71843, #25671, #48945, #54481, #26402, #42297, #21214, #43767, #71473, #15671, #166, #67754, #44866, #5334, #521, #27142, #56658, #66663, #27874, #50761, #67402, #16040, #4612, #22670, #62560, #5695, #39686, #16763, #45221, #17126, #50407, #21950, #40048, #67041, #38955, #55217, #34118, #39321, #22313, #33401, #17486, #50038, #45587, #72564, #61834, #11601, #62205, #6052, #61473, #28587, #51124, #61114, #28231, #72931, #10868, #11956, #23032, #68121, #21582, #10511, #49676, #72205, #11239, #33761, #44136, #38588, #33038, #55578, #56306, #4971, #27505, #44507, #16401, #55938, #41838, #58087, #18922, #6416, #64002, #63640, #35926, #41482, #24482, #47026, #2323, #7860, #51843, #46665, #57011, #24116, #69561, #13382, #68839, #6780, #12673, #69205, #52566, #7495, #34846, #23751, #58449, #30023, #40767, #29312, #19286, #887, #30397, #40397, #1973, #7138, #17836, #52926, #24838, #68474, #47386, #69916, #64368, #34481, #28948, #51487, #23394, #18564, #45943, #62916, #46300, #12311, #57372, #1246, #18196, #63281, #35210, #57732, #29668, #41130, #52204, #1605, #13029, #35568, #70283, #2684, #58815, #20018, #14856, #59547, #37757, #3792, #71012, #64734, #36301, #8226, #59179, #8588, #19654, #42572, #31118, #20390, #42210, #31492, #43679, #53657, #14122, #42939, #37395, #65464, #59919, #9689, #47747, #4160, #65100, #8959, #3050, #14489, #54033, #36660, #21126, #49223, #71757, #25581, #9325, #37023, #20757, #3428, #48120, #65835, #26690, #13758, #30754, #15218, #31858, #25948, #70643, #54393, #48488, #26314, #48853, #53285, #43315, #25200, #71383, #60275, #32222, #54756, #72472, #27783, #22936, #428, #38497, #27417, #10781, #49948, #15949, #61023, #32951, #10420, #55128, #67667, #21858, #66202, #15580, #27055, #55488, #51032, #4526, #72845, #49585, #44420, #38868, #33674, #39591, #4882, #11144, #50321, #17033, #72109, #21493, #66947, #62114, #16315, #61385, #33314, #55852, #5241, #22226, #44782, #60643, #34029, #50674, #67315, #11507, #56566, #44046, #66569, #5962, #16673, #39231, #38122, #45132, #61743, #10058, #56217, #32590, #5610, #28496, #28146, #78, #22583, #24024, #34388, #51757, #34750, #68387, #12586, #28853, #35836, #56920, #41042, #7772, #30307, #52840, #46573, #35120, #1520, #12943, #39956, #17748, #40307, #51392, #1157, #62829, #57644, #35479, #63556, #68751, #12222, #2239, #57284, #29221, #45496, #24391, #7050, #29580, #23666, #68027, #6691, #58359, #46211, #52117, #1885, #58001, #46941, #18109, #7409, #41398, #794, #18477, #40671, #63191, #17399, #29937, #52477, #11867, #23303, #69477, #18834, #69117, #63912, #13299, #62470, #6324, #45852, #48036, #20299, #36939, #58728, #47297, #42853, #32132, #48402, #9237, #69834, #54309, #53943, #26228, #31773, #14763, #37308, #65746, #71289, #42123, #59459, #19197, #14401, #59830, #3701, #59094, #70190, #2961, #8867, #65375, #70928, #25115, #14033, #48766, #20668, #31030, #19568, #9600, #64279, #43226, #30666, #15130, #70561, #8140, #37668, #60190, #53199, #54665, #24754, #41752, #13667, #36211, #2595, #47657, #31403, #64649, #36574, #8499, #53566, #25491, #19937, #42490, #65014, #3339, #25863, #55034, #16226, #32862, #39134, #61296, #38033, #60555, #66111, #49135, #10328, #5153, #49859, #28056, #67222, #10690, #4437, #26594, #62021, #71663, #11421, #26965, #38777, #55397, #61651, #33220, #9962, #32499, #15490, #21038, #4792, #27688, #72383, #50584, #16583, #55759 ) ),
 .UNSPECIFIED., .F., .F., .F. ) 
 B_SPLINE_SURFACE_WITH_KNOTS ( ( 2, 2 ),
 ( 3, 2, 2, 2, 2, 2, 2, 2, 2, 2, 2, 2, 2, 2, 2, 2, 2, 2, 2, 2, 2, 2, 2, 2, 2, 2, 2, 2, 2, 2, 2, 2, 2, 2, 2, 2, 2, 2, 2, 2, 2, 2, 2, 2, 2, 2, 2, 2, 2, 2, 2, 2, 2, 2, 2, 2, 2, 2, 2, 2, 2, 2, 2, 2, 2, 2, 2, 2, 2, 2, 2, 2, 2, 2, 2, 2, 2, 2, 2, 2, 2, 2, 2, 2, 2, 2, 2, 2, 2, 2, 2, 2, 2, 2, 2, 2, 2, 2, 2, 2, 2, 2, 2, 2, 2, 2, 2, 2, 2, 2, 2, 2, 2, 2, 2, 2, 2, 2, 2, 2, 2, 2, 2, 2, 2, 2, 2, 2, 2, 2, 2, 2, 2, 2, 2, 2, 2, 2, 2, 2, 2, 2, 2, 2, 2, 2, 2, 2, 2, 2, 2, 2, 2, 2, 2, 2, 2, 2, 2, 2, 2, 2, 2, 2, 2, 2, 2, 2, 2, 2, 2, 2, 2, 2, 2, 2, 2, 2, 2, 2, 2, 2, 2, 2, 2, 2, 2, 2, 2, 2, 2, 2, 2, 2, 2, 2, 2, 2, 2, 2, 2, 2, 2, 2, 2, 2, 2, 2, 2, 2, 2, 2, 2, 2, 2, 2, 2, 2, 2, 2, 2, 2, 2, 2, 2, 2, 2, 2, 2, 2, 2, 2, 2, 2, 2, 2, 2, 2, 2, 2, 2, 2, 2, 2, 2, 2, 2, 2, 2, 2, 2, 2, 2, 2, 2, 2, 2, 2, 2, 2, 2, 2, 2, 2, 2, 2, 2, 2, 2, 2, 2, 2, 2, 2, 2, 2, 2, 2, 2, 2, 2, 2, 2, 2, 2, 2, 2, 2, 2, 2, 2, 2, 2, 2, 2, 2, 2, 2, 2, 2, 2, 2, 2, 2, 2, 2, 2, 2, 2, 2, 2, 2, 2, 2, 2, 2, 2, 2, 2, 2, 2, 2, 2, 2, 2, 2, 2, 2, 2, 2, 2, 2, 2, 2, 2, 2, 2, 2, 2, 2, 2, 2, 2, 2, 2, 2, 2, 2, 2, 2, 2, 2, 2, 2, 2, 2, 2, 2, 2, 2, 3 ),
 ( 0.000000000000000000, 1.000000000000000000 ),
 ( 0.000000000000000000, 0.002777777777777777884, 0.005555555555555555768, 0.008333333333333333218, 0.01111111111111111154, 0.01388888888888888812, 0.01666666666666666644, 0.01944444444444444475, 0.02222222222222222307, 0.02500000000000000139, 0.02777777777777777624, 0.03055555555555555455, 0.03333333333333333287, 0.03611111111111110772, 0.03888888888888888951, 0.04166666666666666435, 0.04444444444444444614, 0.04722222222222222099, 0.05000000000000000278, 0.05277777777777777762, 0.05555555555555555247, 0.05833333333333333426, 0.06111111111111110911, 0.06388888888888888395, 0.06666666666666666574, 0.06944444444444444753, 0.07222222222222221544, 0.07499999999999999722, 0.07777777777777777901, 0.08055555555555556080, 0.08333333333333332871, 0.08611111111111111049, 0.08888888888888889228, 0.09166666666666666019, 0.09444444444444444198, 0.09722222222222222376, 0.1000000000000000056, 0.1027777777777777735, 0.1055555555555555552, 0.1083333333333333370, 0.1111111111111111049, 0.1138888888888888867, 0.1166666666666666685, 0.1194444444444444503, 0.1222222222222222182, 0.1250000000000000000, 0.1277777777777777679, 0.1305555555555555636, 0.1333333333333333315, 0.1361111111111110994, 0.1388888888888888951, 0.1416666666666666630, 0.1444444444444444309, 0.1472222222222222265, 0.1499999999999999944, 0.1527777777777777901, 0.1555555555555555580, 0.1583333333333333259, 0.1611111111111111216, 0.1638888888888888895, 0.1666666666666666574, 0.1694444444444444531, 0.1722222222222222210, 0.1749999999999999889, 0.1777777777777777846, 0.1805555555555555525, 0.1833333333333333204, 0.1861111111111111160, 0.1888888888888888840, 0.1916666666666666796, 0.1944444444444444475, 0.1972222222222222154, 0.2000000000000000111, 0.2027777777777777790, 0.2055555555555555469, 0.2083333333333333426, 0.2111111111111111105, 0.2138888888888888784, 0.2166666666666666741, 0.2194444444444444420, 0.2222222222222222099, 0.2250000000000000056, 0.2277777777777777735, 0.2305555555555555691, 0.2333333333333333370, 0.2361111111111111049, 0.2388888888888889006, 0.2416666666666666685, 0.2444444444444444364, 0.2472222222222222321, 0.2500000000000000000, 0.2527777777777777679, 0.2555555555555555358, 0.2583333333333333592, 0.2611111111111111271, 0.2638888888888888951, 0.2666666666666666630, 0.2694444444444444309, 0.2722222222222221988, 0.2750000000000000222, 0.2777777777777777901, 0.2805555555555555580, 0.2833333333333333259, 0.2861111111111110938, 0.2888888888888888618, 0.2916666666666666852, 0.2944444444444444531, 0.2972222222222222210, 0.2999999999999999889, 0.3027777777777777568, 0.3055555555555555802, 0.3083333333333333481, 0.3111111111111111160, 0.3138888888888888840, 0.3166666666666666519, 0.3194444444444444198, 0.3222222222222222432, 0.3250000000000000111, 0.3277777777777777790, 0.3305555555555555469, 0.3333333333333333148, 0.3361111111111111382, 0.3388888888888889062, 0.3416666666666666741, 0.3444444444444444420, 0.3472222222222222099, 0.3499999999999999778, 0.3527777777777778012, 0.3555555555555555691, 0.3583333333333333370, 0.3611111111111111049, 0.3638888888888888729, 0.3666666666666666408, 0.3694444444444444642, 0.3722222222222222321, 0.3750000000000000000, 0.3777777777777777679, 0.3805555555555555358, 0.3833333333333333592, 0.3861111111111111271, 0.3888888888888888951, 0.3916666666666666630, 0.3944444444444444309, 0.3972222222222221988, 0.4000000000000000222, 0.4027777777777777901, 0.4055555555555555580, 0.4083333333333333259, 0.4111111111111110938, 0.4138888888888888618, 0.4166666666666666852, 0.4194444444444444531, 0.4222222222222222210, 0.4249999999999999889, 0.4277777777777777568, 0.4305555555555555802, 0.4333333333333333481, 0.4361111111111111160, 0.4388888888888888840, 0.4416666666666666519, 0.4444444444444444198, 0.4472222222222222432, 0.4500000000000000111, 0.4527777777777777790, 0.4555555555555555469, 0.4583333333333333148, 0.4611111111111111382, 0.4638888888888889062, 0.4666666666666666741, 0.4694444444444444420, 0.4722222222222222099, 0.4749999999999999778, 0.4777777777777778012, 0.4805555555555555691, 0.4833333333333333370, 0.4861111111111111049, 0.4888888888888888729, 0.4916666666666666408, 0.4944444444444444642, 0.4972222222222222321, 0.5000000000000000000, 0.5027777777777777679, 0.5055555555555555358, 0.5083333333333333037, 0.5111111111111110716, 0.5138888888888888395, 0.5166666666666667185, 0.5194444444444444864, 0.5222222222222222543, 0.5250000000000000222, 0.5277777777777777901, 0.5305555555555555580, 0.5333333333333333259, 0.5361111111111110938, 0.5388888888888888618, 0.5416666666666666297, 0.5444444444444443976, 0.5472222222222222765, 0.5500000000000000444, 0.5527777777777778123, 0.5555555555555555802, 0.5583333333333333481, 0.5611111111111111160, 0.5638888888888888840, 0.5666666666666666519, 0.5694444444444444198, 0.5722222222222221877, 0.5749999999999999556, 0.5777777777777777235, 0.5805555555555556024, 0.5833333333333333703, 0.5861111111111111382, 0.5888888888888889062, 0.5916666666666666741, 0.5944444444444444420, 0.5972222222222222099, 0.5999999999999999778, 0.6027777777777777457, 0.6055555555555555136, 0.6083333333333332815, 0.6111111111111111605, 0.6138888888888889284, 0.6166666666666666963, 0.6194444444444444642, 0.6222222222222222321, 0.6250000000000000000, 0.6277777777777777679, 0.6305555555555555358, 0.6333333333333333037, 0.6361111111111110716, 0.6388888888888888395, 0.6416666666666667185, 0.6444444444444444864, 0.6472222222222222543, 0.6500000000000000222, 0.6527777777777777901, 0.6555555555555555580, 0.6583333333333333259, 0.6611111111111110938, 0.6638888888888888618, 0.6666666666666666297, 0.6694444444444443976, 0.6722222222222222765, 0.6750000000000000444, 0.6777777777777778123, 0.6805555555555555802, 0.6833333333333333481, 0.6861111111111111160, 0.6888888888888888840, 0.6916666666666666519, 0.6944444444444444198, 0.6972222222222221877, 0.6999999999999999556, 0.7027777777777777235, 0.7055555555555556024, 0.7083333333333333703, 0.7111111111111111382, 0.7138888888888889062, 0.7166666666666666741, 0.7194444444444444420, 0.7222222222222222099, 0.7249999999999999778, 0.7277777777777777457, 0.7305555555555555136, 0.7333333333333332815, 0.7361111111111111605, 0.7388888888888889284, 0.7416666666666666963, 0.7444444444444444642, 0.7472222222222222321, 0.7500000000000000000, 0.7527777777777777679, 0.7555555555555555358, 0.7583333333333333037, 0.7611111111111110716, 0.7638888888888888395, 0.7666666666666667185, 0.7694444444444444864, 0.7722222222222222543, 0.7750000000000000222, 0.7777777777777777901, 0.7805555555555555580, 0.7833333333333333259, 0.7861111111111110938, 0.7888888888888888618, 0.7916666666666666297, 0.7944444444444443976, 0.7972222222222222765, 0.8000000000000000444, 0.8027777777777778123, 0.8055555555555555802, 0.8083333333333333481, 0.8111111111111111160, 0.8138888888888888840, 0.8166666666666666519, 0.8194444444444444198, 0.8222222222222221877, 0.8249999999999999556, 0.8277777777777777235, 0.8305555555555556024, 0.8333333333333333703, 0.8361111111111111382, 0.8388888888888889062, 0.8416666666666666741, 0.8444444444444444420, 0.8472222222222222099, 0.8499999999999999778, 0.8527777777777777457, 0.8555555555555555136, 0.8583333333333332815, 0.8611111111111111605, 0.8638888888888889284, 0.8666666666666666963, 0.8694444444444444642, 0.8722222222222222321, 0.8750000000000000000, 0.8777777777777777679, 0.8805555555555555358, 0.8833333333333333037, 0.8861111111111110716, 0.8888888888888888395, 0.8916666666666667185, 0.8944444444444444864, 0.8972222222222222543, 0.9000000000000000222, 0.9027777777777777901, 0.9055555555555555580, 0.9083333333333333259, 0.9111111111111110938, 0.9138888888888888618, 0.9166666666666666297, 0.9194444444444443976, 0.9222222222222222765, 0.9250000000000000444, 0.9277777777777778123, 0.9305555555555555802, 0.9333333333333333481, 0.9361111111111111160, 0.9388888888888888840, 0.9416666666666666519, 0.9444444444444444198, 0.9472222222222221877, 0.9499999999999999556, 0.9527777777777777235, 0.9555555555555556024, 0.9583333333333333703, 0.9611111111111111382, 0.9638888888888889062, 0.9666666666666666741, 0.9694444444444444420, 0.9722222222222222099, 0.9749999999999999778, 0.9777777777777777457, 0.9805555555555555136, 0.9833333333333332815, 0.9861111111111111605, 0.9888888888888889284, 0.9916666666666666963, 0.9944444444444444642, 0.9972222222222222321, 1.000000000000000000 ),
 .UNSPECIFIED. ) 
 GEOMETRIC_REPRESENTATION_ITEM ( )  RATIONAL_B_SPLINE_SURFACE ( (
 ( 1.000000000000000000, 0.8660254037844387076, 1.000000000000000000, 0.8660254037844387076, 1.000000000000000000, 0.8660254037844387076, 1.000000000000000000, 0.8660254037844387076, 1.000000000000000000, 0.8660254037844387076, 1.000000000000000000, 0.8660254037844387076, 1.000000000000000000, 0.8660254037844387076, 1.000000000000000000, 0.8660254037844387076, 1.000000000000000000, 0.8660254037844387076, 1.000000000000000000, 0.8660254037844387076, 1.000000000000000000, 0.8660254037844387076, 1.000000000000000000, 0.8660254037844387076, 1.000000000000000000, 0.8660254037844387076, 1.000000000000000000, 0.8660254037844387076, 1.000000000000000000, 0.8660254037844387076, 1.000000000000000000, 0.8660254037844387076, 1.000000000000000000, 0.8660254037844387076, 1.000000000000000000, 0.8660254037844387076, 1.000000000000000000, 0.8660254037844387076, 1.000000000000000000, 0.8660254037844387076, 1.000000000000000000, 0.8660254037844387076, 1.000000000000000000, 0.8660254037844387076, 1.000000000000000000, 0.8660254037844387076, 1.000000000000000000, 0.8660254037844387076, 1.000000000000000000, 0.8660254037844387076, 1.000000000000000000, 0.8660254037844387076, 1.000000000000000000, 0.8660254037844387076, 1.000000000000000000, 0.8660254037844387076, 1.000000000000000000, 0.8660254037844387076, 1.000000000000000000, 0.8660254037844387076, 1.000000000000000000, 0.8660254037844387076, 1.000000000000000000, 0.8660254037844387076, 1.000000000000000000, 0.8660254037844387076, 1.000000000000000000, 0.8660254037844387076, 1.000000000000000000, 0.8660254037844387076, 1.000000000000000000, 0.8660254037844387076, 1.000000000000000000, 0.8660254037844387076, 1.000000000000000000, 0.8660254037844387076, 1.000000000000000000, 0.8660254037844387076, 1.000000000000000000, 0.8660254037844387076, 1.000000000000000000, 0.8660254037844387076, 1.000000000000000000, 0.8660254037844387076, 1.000000000000000000, 0.8660254037844387076, 1.000000000000000000, 0.8660254037844387076, 1.000000000000000000, 0.8660254037844387076, 1.000000000000000000, 0.8660254037844387076, 1.000000000000000000, 0.8660254037844387076, 1.000000000000000000, 0.8660254037844387076, 1.000000000000000000, 0.8660254037844387076, 1.000000000000000000, 0.8660254037844387076, 1.000000000000000000, 0.8660254037844387076, 1.000000000000000000, 0.8660254037844387076, 1.000000000000000000, 0.8660254037844387076, 1.000000000000000000, 0.8660254037844387076, 1.000000000000000000, 0.8660254037844387076, 1.000000000000000000, 0.8660254037844387076, 1.000000000000000000, 0.8660254037844387076, 1.000000000000000000, 0.8660254037844387076, 1.000000000000000000, 0.8660254037844387076, 1.000000000000000000, 0.8660254037844387076, 1.000000000000000000, 0.8660254037844387076, 1.000000000000000000, 0.8660254037844387076, 1.000000000000000000, 0.8660254037844387076, 1.000000000000000000, 0.8660254037844387076, 1.000000000000000000, 0.8660254037844387076, 1.000000000000000000, 0.8660254037844387076, 1.000000000000000000, 0.8660254037844387076, 1.000000000000000000, 0.8660254037844387076, 1.000000000000000000, 0.8660254037844387076, 1.000000000000000000, 0.8660254037844387076, 1.000000000000000000, 0.8660254037844387076, 1.000000000000000000, 0.8660254037844387076, 1.000000000000000000, 0.8660254037844387076, 1.000000000000000000, 0.8660254037844387076, 1.000000000000000000, 0.8660254037844387076, 1.000000000000000000, 0.8660254037844387076, 1.000000000000000000, 0.8660254037844387076, 1.000000000000000000, 0.8660254037844387076, 1.000000000000000000, 0.8660254037844387076, 1.000000000000000000, 0.8660254037844387076, 1.000000000000000000, 0.8660254037844387076, 1.000000000000000000, 0.8660254037844387076, 1.000000000000000000, 0.8660254037844387076, 1.000000000000000000, 0.8660254037844387076, 1.000000000000000000, 0.8660254037844387076, 1.000000000000000000, 0.8660254037844387076, 1.000000000000000000, 0.8660254037844387076, 1.000000000000000000, 0.8660254037844387076, 1.000000000000000000, 0.8660254037844387076, 1.000000000000000000, 0.8660254037844387076, 1.000000000000000000, 0.8660254037844387076, 1.000000000000000000, 0.8660254037844387076, 1.000000000000000000, 0.8660254037844387076, 1.000000000000000000, 0.8660254037844387076, 1.000000000000000000, 0.8660254037844387076, 1.000000000000000000, 0.8660254037844387076, 1.000000000000000000, 0.8660254037844387076, 1.000000000000000000, 0.8660254037844387076, 1.000000000000000000, 0.8660254037844387076, 1.000000000000000000, 0.8660254037844387076, 1.000000000000000000, 0.8660254037844387076, 1.000000000000000000, 0.8660254037844387076, 1.000000000000000000, 0.8660254037844387076, 1.000000000000000000, 0.8660254037844387076, 1.000000000000000000, 0.8660254037844387076, 1.000000000000000000, 0.8660254037844387076, 1.000000000000000000, 0.8660254037844387076, 1.000000000000000000, 0.8660254037844387076, 1.000000000000000000, 0.8660254037844387076, 1.000000000000000000, 0.8660254037844387076, 1.000000000000000000, 0.8660254037844387076, 1.000000000000000000, 0.8660254037844387076, 1.000000000000000000, 0.8660254037844387076, 1.000000000000000000, 0.8660254037844387076, 1.000000000000000000, 0.8660254037844387076, 1.000000000000000000, 0.8660254037844387076, 1.000000000000000000, 0.8660254037844387076, 1.000000000000000000, 0.8660254037844387076, 1.000000000000000000, 0.8660254037844387076, 1.000000000000000000, 0.8660254037844387076, 1.000000000000000000, 0.8660254037844387076, 1.000000000000000000, 0.8660254037844387076, 1.000000000000000000, 0.8660254037844387076, 1.000000000000000000, 0.8660254037844387076, 1.000000000000000000, 0.8660254037844387076, 1.000000000000000000, 0.8660254037844387076, 1.000000000000000000, 0.8660254037844387076, 1.000000000000000000, 0.8660254037844387076, 1.000000000000000000, 0.8660254037844387076, 1.000000000000000000, 0.8660254037844387076, 1.000000000000000000, 0.8660254037844387076, 1.000000000000000000, 0.8660254037844387076, 1.000000000000000000, 0.8660254037844387076, 1.000000000000000000, 0.8660254037844387076, 1.000000000000000000, 0.8660254037844387076, 1.000000000000000000, 0.8660254037844387076, 1.000000000000000000, 0.8660254037844387076, 1.000000000000000000, 0.8660254037844387076, 1.000000000000000000, 0.8660254037844387076, 1.000000000000000000, 0.8660254037844387076, 1.000000000000000000, 0.8660254037844387076, 1.000000000000000000, 0.8660254037844387076, 1.000000000000000000, 0.8660254037844387076, 1.000000000000000000, 0.8660254037844387076, 1.000000000000000000, 0.8660254037844387076, 1.000000000000000000, 0.8660254037844387076, 1.000000000000000000, 0.8660254037844387076, 1.000000000000000000, 0.8660254037844387076, 1.000000000000000000, 0.8660254037844387076, 1.000000000000000000, 0.8660254037844387076, 1.000000000000000000, 0.8660254037844387076, 1.000000000000000000, 0.8660254037844387076, 1.000000000000000000, 0.8660254037844387076, 1.000000000000000000, 0.8660254037844387076, 1.000000000000000000, 0.8660254037844387076, 1.000000000000000000, 0.8660254037844387076, 1.000000000000000000, 0.8660254037844387076, 1.000000000000000000, 0.8660254037844387076, 1.000000000000000000, 0.8660254037844387076, 1.000000000000000000, 0.8660254037844387076, 1.000000000000000000, 0.8660254037844387076, 1.000000000000000000, 0.8660254037844387076, 1.000000000000000000, 0.8660254037844387076, 1.000000000000000000, 0.8660254037844387076, 1.000000000000000000, 0.8660254037844387076, 1.000000000000000000, 0.8660254037844387076, 1.000000000000000000, 0.8660254037844387076, 1.000000000000000000, 0.8660254037844387076, 1.000000000000000000, 0.8660254037844387076, 1.000000000000000000, 0.8660254037844387076, 1.000000000000000000, 0.8660254037844387076, 1.000000000000000000, 0.8660254037844387076, 1.000000000000000000, 0.8660254037844387076, 1.000000000000000000, 0.8660254037844387076, 1.000000000000000000, 0.8660254037844387076, 1.000000000000000000, 0.8660254037844387076, 1.000000000000000000, 0.8660254037844387076, 1.000000000000000000, 0.8660254037844387076, 1.000000000000000000, 0.8660254037844387076, 1.000000000000000000, 0.8660254037844387076, 1.000000000000000000, 0.8660254037844387076, 1.000000000000000000, 0.8660254037844387076, 1.000000000000000000, 0.8660254037844387076, 1.000000000000000000, 0.8660254037844387076, 1.000000000000000000, 0.8660254037844387076, 1.000000000000000000, 0.8660254037844387076, 1.000000000000000000, 0.8660254037844387076, 1.000000000000000000, 0.8660254037844387076, 1.000000000000000000, 0.8660254037844387076, 1.000000000000000000, 0.8660254037844387076, 1.000000000000000000, 0.8660254037844387076, 1.000000000000000000, 0.8660254037844387076, 1.000000000000000000, 0.8660254037844387076, 1.000000000000000000, 0.8660254037844387076, 1.000000000000000000, 0.8660254037844387076, 1.000000000000000000, 0.8660254037844387076, 1.000000000000000000, 0.8660254037844387076, 1.000000000000000000, 0.8660254037844387076, 1.000000000000000000, 0.8660254037844387076, 1.000000000000000000, 0.8660254037844387076, 1.000000000000000000, 0.8660254037844387076, 1.000000000000000000, 0.8660254037844387076, 1.000000000000000000, 0.8660254037844387076, 1.000000000000000000, 0.8660254037844387076, 1.000000000000000000, 0.8660254037844387076, 1.000000000000000000, 0.8660254037844387076, 1.000000000000000000, 0.8660254037844387076, 1.000000000000000000, 0.8660254037844387076, 1.000000000000000000, 0.8660254037844387076, 1.000000000000000000, 0.8660254037844387076, 1.000000000000000000, 0.8660254037844387076, 1.000000000000000000, 0.8660254037844387076, 1.000000000000000000, 0.8660254037844387076, 1.000000000000000000, 0.8660254037844387076, 1.000000000000000000, 0.8660254037844387076, 1.000000000000000000, 0.8660254037844387076, 1.000000000000000000, 0.8660254037844387076, 1.000000000000000000, 0.8660254037844387076, 1.000000000000000000, 0.8660254037844387076, 1.000000000000000000, 0.8660254037844387076, 1.000000000000000000, 0.8660254037844387076, 1.000000000000000000, 0.8660254037844387076, 1.000000000000000000, 0.8660254037844387076, 1.000000000000000000, 0.8660254037844387076, 1.000000000000000000, 0.8660254037844387076, 1.000000000000000000, 0.8660254037844387076, 1.000000000000000000, 0.8660254037844387076, 1.000000000000000000, 0.8660254037844387076, 1.000000000000000000, 0.8660254037844387076, 1.000000000000000000, 0.8660254037844387076, 1.000000000000000000, 0.8660254037844387076, 1.000000000000000000, 0.8660254037844387076, 1.000000000000000000, 0.8660254037844387076, 1.000000000000000000, 0.8660254037844387076, 1.000000000000000000, 0.8660254037844387076, 1.000000000000000000, 0.8660254037844387076, 1.000000000000000000, 0.8660254037844387076, 1.000000000000000000, 0.8660254037844387076, 1.000000000000000000, 0.8660254037844387076, 1.000000000000000000, 0.8660254037844387076, 1.000000000000000000, 0.8660254037844387076, 1.000000000000000000, 0.8660254037844387076, 1.000000000000000000, 0.8660254037844387076, 1.000000000000000000, 0.8660254037844387076, 1.000000000000000000, 0.8660254037844387076, 1.000000000000000000, 0.8660254037844387076, 1.000000000000000000, 0.8660254037844387076, 1.000000000000000000, 0.8660254037844387076, 1.000000000000000000, 0.8660254037844387076, 1.000000000000000000, 0.8660254037844387076, 1.000000000000000000, 0.8660254037844387076, 1.000000000000000000, 0.8660254037844387076, 1.000000000000000000, 0.8660254037844387076, 1.000000000000000000, 0.8660254037844387076, 1.000000000000000000, 0.8660254037844387076, 1.000000000000000000, 0.8660254037844387076, 1.000000000000000000, 0.8660254037844387076, 1.000000000000000000, 0.8660254037844387076, 1.000000000000000000, 0.8660254037844387076, 1.000000000000000000, 0.8660254037844387076, 1.000000000000000000, 0.8660254037844387076, 1.000000000000000000, 0.8660254037844387076, 1.000000000000000000, 0.8660254037844387076, 1.000000000000000000, 0.8660254037844387076, 1.000000000000000000, 0.8660254037844387076, 1.000000000000000000, 0.8660254037844387076, 1.000000000000000000, 0.8660254037844387076, 1.000000000000000000, 0.8660254037844387076, 1.000000000000000000, 0.8660254037844387076, 1.000000000000000000, 0.8660254037844387076, 1.000000000000000000, 0.8660254037844387076, 1.000000000000000000, 0.8660254037844387076, 1.000000000000000000, 0.8660254037844387076, 1.000000000000000000, 0.8660254037844387076, 1.000000000000000000, 0.8660254037844387076, 1.000000000000000000, 0.8660254037844387076, 1.000000000000000000, 0.8660254037844387076, 1.000000000000000000, 0.8660254037844387076, 1.000000000000000000, 0.8660254037844387076, 1.000000000000000000, 0.8660254037844387076, 1.000000000000000000, 0.8660254037844387076, 1.000000000000000000, 0.8660254037844387076, 1.000000000000000000, 0.8660254037844387076, 1.000000000000000000, 0.8660254037844387076, 1.000000000000000000, 0.8660254037844387076, 1.000000000000000000, 0.8660254037844387076, 1.000000000000000000, 0.8660254037844387076, 1.000000000000000000, 0.8660254037844387076, 1.000000000000000000, 0.8660254037844387076, 1.000000000000000000, 0.8660254037844387076, 1.000000000000000000, 0.8660254037844387076, 1.000000000000000000, 0.8660254037844387076, 1.000000000000000000, 0.8660254037844387076, 1.000000000000000000, 0.8660254037844387076, 1.000000000000000000, 0.8660254037844387076, 1.000000000000000000, 0.8660254037844387076, 1.000000000000000000, 0.8660254037844387076, 1.000000000000000000, 0.8660254037844387076, 1.000000000000000000, 0.8660254037844387076, 1.000000000000000000, 0.8660254037844387076, 1.000000000000000000, 0.8660254037844387076, 1.000000000000000000, 0.8660254037844387076, 1.000000000000000000, 0.8660254037844387076, 1.000000000000000000, 0.8660254037844387076, 1.000000000000000000, 0.8660254037844387076, 1.000000000000000000, 0.8660254037844387076, 1.000000000000000000, 0.8660254037844387076, 1.000000000000000000, 0.8660254037844387076, 1.000000000000000000, 0.8660254037844387076, 1.000000000000000000, 0.8660254037844387076, 1.000000000000000000, 0.8660254037844387076, 1.000000000000000000, 0.8660254037844387076, 1.000000000000000000, 0.8660254037844387076, 1.000000000000000000, 0.8660254037844387076, 1.000000000000000000, 0.8660254037844387076, 1.000000000000000000, 0.8660254037844387076, 1.000000000000000000, 0.8660254037844387076, 1.000000000000000000, 0.8660254037844387076, 1.000000000000000000, 0.8660254037844387076, 1.000000000000000000, 0.8660254037844387076, 1.000000000000000000, 0.8660254037844387076, 1.000000000000000000, 0.8660254037844387076, 1.000000000000000000, 0.8660254037844387076, 1.000000000000000000, 0.8660254037844387076, 1.000000000000000000, 0.8660254037844387076, 1.000000000000000000, 0.8660254037844387076, 1.000000000000000000, 0.8660254037844387076, 1.000000000000000000, 0.8660254037844387076, 1.000000000000000000, 0.8660254037844387076, 1.000000000000000000, 0.8660254037844387076, 1.000000000000000000, 0.8660254037844387076, 1.000000000000000000, 0.8660254037844387076, 1.000000000000000000, 0.8660254037844387076, 1.000000000000000000, 0.8660254037844387076, 1.000000000000000000, 0.8660254037844387076, 1.000000000000000000, 0.8660254037844387076, 1.000000000000000000, 0.8660254037844387076, 1.000000000000000000, 0.8660254037844387076, 1.000000000000000000, 0.8660254037844387076, 1.000000000000000000, 0.8660254037844387076, 1.000000000000000000, 0.8660254037844387076, 1.000000000000000000, 0.8660254037844387076, 1.000000000000000000, 0.8660254037844387076, 1.000000000000000000, 0.8660254037844387076, 1.000000000000000000, 0.8660254037844387076, 1.000000000000000000, 0.8660254037844387076, 1.000000000000000000, 0.8660254037844387076, 1.000000000000000000, 0.8660254037844387076, 1.000000000000000000, 0.8660254037844387076, 1.000000000000000000, 0.8660254037844387076, 1.000000000000000000, 0.8660254037844387076, 1.000000000000000000, 0.8660254037844387076, 1.000000000000000000, 0.8660254037844387076, 1.000000000000000000, 0.8660254037844387076, 1.000000000000000000, 0.8660254037844387076, 1.000000000000000000, 0.8660254037844387076, 1.000000000000000000, 0.8660254037844387076, 1.000000000000000000, 0.8660254037844387076, 1.000000000000000000, 0.8660254037844387076, 1.000000000000000000, 0.8660254037844387076, 1.000000000000000000),
 ( 1.000000000000000000, 0.8660254037844387076, 1.000000000000000000, 0.8660254037844387076, 1.000000000000000000, 0.8660254037844387076, 1.000000000000000000, 0.8660254037844387076, 1.000000000000000000, 0.8660254037844387076, 1.000000000000000000, 0.8660254037844387076, 1.000000000000000000, 0.8660254037844387076, 1.000000000000000000, 0.8660254037844387076, 1.000000000000000000, 0.8660254037844387076, 1.000000000000000000, 0.8660254037844387076, 1.000000000000000000, 0.8660254037844387076, 1.000000000000000000, 0.8660254037844387076, 1.000000000000000000, 0.8660254037844387076, 1.000000000000000000, 0.8660254037844387076, 1.000000000000000000, 0.8660254037844387076, 1.000000000000000000, 0.8660254037844387076, 1.000000000000000000, 0.8660254037844387076, 1.000000000000000000, 0.8660254037844387076, 1.000000000000000000, 0.8660254037844387076, 1.000000000000000000, 0.8660254037844387076, 1.000000000000000000, 0.8660254037844387076, 1.000000000000000000, 0.8660254037844387076, 1.000000000000000000, 0.8660254037844387076, 1.000000000000000000, 0.8660254037844387076, 1.000000000000000000, 0.8660254037844387076, 1.000000000000000000, 0.8660254037844387076, 1.000000000000000000, 0.8660254037844387076, 1.000000000000000000, 0.8660254037844387076, 1.000000000000000000, 0.8660254037844387076, 1.000000000000000000, 0.8660254037844387076, 1.000000000000000000, 0.8660254037844387076, 1.000000000000000000, 0.8660254037844387076, 1.000000000000000000, 0.8660254037844387076, 1.000000000000000000, 0.8660254037844387076, 1.000000000000000000, 0.8660254037844387076, 1.000000000000000000, 0.8660254037844387076, 1.000000000000000000, 0.8660254037844387076, 1.000000000000000000, 0.8660254037844387076, 1.000000000000000000, 0.8660254037844387076, 1.000000000000000000, 0.8660254037844387076, 1.000000000000000000, 0.8660254037844387076, 1.000000000000000000, 0.8660254037844387076, 1.000000000000000000, 0.8660254037844387076, 1.000000000000000000, 0.8660254037844387076, 1.000000000000000000, 0.8660254037844387076, 1.000000000000000000, 0.8660254037844387076, 1.000000000000000000, 0.8660254037844387076, 1.000000000000000000, 0.8660254037844387076, 1.000000000000000000, 0.8660254037844387076, 1.000000000000000000, 0.8660254037844387076, 1.000000000000000000, 0.8660254037844387076, 1.000000000000000000, 0.8660254037844387076, 1.000000000000000000, 0.8660254037844387076, 1.000000000000000000, 0.8660254037844387076, 1.000000000000000000, 0.8660254037844387076, 1.000000000000000000, 0.8660254037844387076, 1.000000000000000000, 0.8660254037844387076, 1.000000000000000000, 0.8660254037844387076, 1.000000000000000000, 0.8660254037844387076, 1.000000000000000000, 0.8660254037844387076, 1.000000000000000000, 0.8660254037844387076, 1.000000000000000000, 0.8660254037844387076, 1.000000000000000000, 0.8660254037844387076, 1.000000000000000000, 0.8660254037844387076, 1.000000000000000000, 0.8660254037844387076, 1.000000000000000000, 0.8660254037844387076, 1.000000000000000000, 0.8660254037844387076, 1.000000000000000000, 0.8660254037844387076, 1.000000000000000000, 0.8660254037844387076, 1.000000000000000000, 0.8660254037844387076, 1.000000000000000000, 0.8660254037844387076, 1.000000000000000000, 0.8660254037844387076, 1.000000000000000000, 0.8660254037844387076, 1.000000000000000000, 0.8660254037844387076, 1.000000000000000000, 0.8660254037844387076, 1.000000000000000000, 0.8660254037844387076, 1.000000000000000000, 0.8660254037844387076, 1.000000000000000000, 0.8660254037844387076, 1.000000000000000000, 0.8660254037844387076, 1.000000000000000000, 0.8660254037844387076, 1.000000000000000000, 0.8660254037844387076, 1.000000000000000000, 0.8660254037844387076, 1.000000000000000000, 0.8660254037844387076, 1.000000000000000000, 0.8660254037844387076, 1.000000000000000000, 0.8660254037844387076, 1.000000000000000000, 0.8660254037844387076, 1.000000000000000000, 0.8660254037844387076, 1.000000000000000000, 0.8660254037844387076, 1.000000000000000000, 0.8660254037844387076, 1.000000000000000000, 0.8660254037844387076, 1.000000000000000000, 0.8660254037844387076, 1.000000000000000000, 0.8660254037844387076, 1.000000000000000000, 0.8660254037844387076, 1.000000000000000000, 0.8660254037844387076, 1.000000000000000000, 0.8660254037844387076, 1.000000000000000000, 0.8660254037844387076, 1.000000000000000000, 0.8660254037844387076, 1.000000000000000000, 0.8660254037844387076, 1.000000000000000000, 0.8660254037844387076, 1.000000000000000000, 0.8660254037844387076, 1.000000000000000000, 0.8660254037844387076, 1.000000000000000000, 0.8660254037844387076, 1.000000000000000000, 0.8660254037844387076, 1.000000000000000000, 0.8660254037844387076, 1.000000000000000000, 0.8660254037844387076, 1.000000000000000000, 0.8660254037844387076, 1.000000000000000000, 0.8660254037844387076, 1.000000000000000000, 0.8660254037844387076, 1.000000000000000000, 0.8660254037844387076, 1.000000000000000000, 0.8660254037844387076, 1.000000000000000000, 0.8660254037844387076, 1.000000000000000000, 0.8660254037844387076, 1.000000000000000000, 0.8660254037844387076, 1.000000000000000000, 0.8660254037844387076, 1.000000000000000000, 0.8660254037844387076, 1.000000000000000000, 0.8660254037844387076, 1.000000000000000000, 0.8660254037844387076, 1.000000000000000000, 0.8660254037844387076, 1.000000000000000000, 0.8660254037844387076, 1.000000000000000000, 0.8660254037844387076, 1.000000000000000000, 0.8660254037844387076, 1.000000000000000000, 0.8660254037844387076, 1.000000000000000000, 0.8660254037844387076, 1.000000000000000000, 0.8660254037844387076, 1.000000000000000000, 0.8660254037844387076, 1.000000000000000000, 0.8660254037844387076, 1.000000000000000000, 0.8660254037844387076, 1.000000000000000000, 0.8660254037844387076, 1.000000000000000000, 0.8660254037844387076, 1.000000000000000000, 0.8660254037844387076, 1.000000000000000000, 0.8660254037844387076, 1.000000000000000000, 0.8660254037844387076, 1.000000000000000000, 0.8660254037844387076, 1.000000000000000000, 0.8660254037844387076, 1.000000000000000000, 0.8660254037844387076, 1.000000000000000000, 0.8660254037844387076, 1.000000000000000000, 0.8660254037844387076, 1.000000000000000000, 0.8660254037844387076, 1.000000000000000000, 0.8660254037844387076, 1.000000000000000000, 0.8660254037844387076, 1.000000000000000000, 0.8660254037844387076, 1.000000000000000000, 0.8660254037844387076, 1.000000000000000000, 0.8660254037844387076, 1.000000000000000000, 0.8660254037844387076, 1.000000000000000000, 0.8660254037844387076, 1.000000000000000000, 0.8660254037844387076, 1.000000000000000000, 0.8660254037844387076, 1.000000000000000000, 0.8660254037844387076, 1.000000000000000000, 0.8660254037844387076, 1.000000000000000000, 0.8660254037844387076, 1.000000000000000000, 0.8660254037844387076, 1.000000000000000000, 0.8660254037844387076, 1.000000000000000000, 0.8660254037844387076, 1.000000000000000000, 0.8660254037844387076, 1.000000000000000000, 0.8660254037844387076, 1.000000000000000000, 0.8660254037844387076, 1.000000000000000000, 0.8660254037844387076, 1.000000000000000000, 0.8660254037844387076, 1.000000000000000000, 0.8660254037844387076, 1.000000000000000000, 0.8660254037844387076, 1.000000000000000000, 0.8660254037844387076, 1.000000000000000000, 0.8660254037844387076, 1.000000000000000000, 0.8660254037844387076, 1.000000000000000000, 0.8660254037844387076, 1.000000000000000000, 0.8660254037844387076, 1.000000000000000000, 0.8660254037844387076, 1.000000000000000000, 0.8660254037844387076, 1.000000000000000000, 0.8660254037844387076, 1.000000000000000000, 0.8660254037844387076, 1.000000000000000000, 0.8660254037844387076, 1.000000000000000000, 0.8660254037844387076, 1.000000000000000000, 0.8660254037844387076, 1.000000000000000000, 0.8660254037844387076, 1.000000000000000000, 0.8660254037844387076, 1.000000000000000000, 0.8660254037844387076, 1.000000000000000000, 0.8660254037844387076, 1.000000000000000000, 0.8660254037844387076, 1.000000000000000000, 0.8660254037844387076, 1.000000000000000000, 0.8660254037844387076, 1.000000000000000000, 0.8660254037844387076, 1.000000000000000000, 0.8660254037844387076, 1.000000000000000000, 0.8660254037844387076, 1.000000000000000000, 0.8660254037844387076, 1.000000000000000000, 0.8660254037844387076, 1.000000000000000000, 0.8660254037844387076, 1.000000000000000000, 0.8660254037844387076, 1.000000000000000000, 0.8660254037844387076, 1.000000000000000000, 0.8660254037844387076, 1.000000000000000000, 0.8660254037844387076, 1.000000000000000000, 0.8660254037844387076, 1.000000000000000000, 0.8660254037844387076, 1.000000000000000000, 0.8660254037844387076, 1.000000000000000000, 0.8660254037844387076, 1.000000000000000000, 0.8660254037844387076, 1.000000000000000000, 0.8660254037844387076, 1.000000000000000000, 0.8660254037844387076, 1.000000000000000000, 0.8660254037844387076, 1.000000000000000000, 0.8660254037844387076, 1.000000000000000000, 0.8660254037844387076, 1.000000000000000000, 0.8660254037844387076, 1.000000000000000000, 0.8660254037844387076, 1.000000000000000000, 0.8660254037844387076, 1.000000000000000000, 0.8660254037844387076, 1.000000000000000000, 0.8660254037844387076, 1.000000000000000000, 0.8660254037844387076, 1.000000000000000000, 0.8660254037844387076, 1.000000000000000000, 0.8660254037844387076, 1.000000000000000000, 0.8660254037844387076, 1.000000000000000000, 0.8660254037844387076, 1.000000000000000000, 0.8660254037844387076, 1.000000000000000000, 0.8660254037844387076, 1.000000000000000000, 0.8660254037844387076, 1.000000000000000000, 0.8660254037844387076, 1.000000000000000000, 0.8660254037844387076, 1.000000000000000000, 0.8660254037844387076, 1.000000000000000000, 0.8660254037844387076, 1.000000000000000000, 0.8660254037844387076, 1.000000000000000000, 0.8660254037844387076, 1.000000000000000000, 0.8660254037844387076, 1.000000000000000000, 0.8660254037844387076, 1.000000000000000000, 0.8660254037844387076, 1.000000000000000000, 0.8660254037844387076, 1.000000000000000000, 0.8660254037844387076, 1.000000000000000000, 0.8660254037844387076, 1.000000000000000000, 0.8660254037844387076, 1.000000000000000000, 0.8660254037844387076, 1.000000000000000000, 0.8660254037844387076, 1.000000000000000000, 0.8660254037844387076, 1.000000000000000000, 0.8660254037844387076, 1.000000000000000000, 0.8660254037844387076, 1.000000000000000000, 0.8660254037844387076, 1.000000000000000000, 0.8660254037844387076, 1.000000000000000000, 0.8660254037844387076, 1.000000000000000000, 0.8660254037844387076, 1.000000000000000000, 0.8660254037844387076, 1.000000000000000000, 0.8660254037844387076, 1.000000000000000000, 0.8660254037844387076, 1.000000000000000000, 0.8660254037844387076, 1.000000000000000000, 0.8660254037844387076, 1.000000000000000000, 0.8660254037844387076, 1.000000000000000000, 0.8660254037844387076, 1.000000000000000000, 0.8660254037844387076, 1.000000000000000000, 0.8660254037844387076, 1.000000000000000000, 0.8660254037844387076, 1.000000000000000000, 0.8660254037844387076, 1.000000000000000000, 0.8660254037844387076, 1.000000000000000000, 0.8660254037844387076, 1.000000000000000000, 0.8660254037844387076, 1.000000000000000000, 0.8660254037844387076, 1.000000000000000000, 0.8660254037844387076, 1.000000000000000000, 0.8660254037844387076, 1.000000000000000000, 0.8660254037844387076, 1.000000000000000000, 0.8660254037844387076, 1.000000000000000000, 0.8660254037844387076, 1.000000000000000000, 0.8660254037844387076, 1.000000000000000000, 0.8660254037844387076, 1.000000000000000000, 0.8660254037844387076, 1.000000000000000000, 0.8660254037844387076, 1.000000000000000000, 0.8660254037844387076, 1.000000000000000000, 0.8660254037844387076, 1.000000000000000000, 0.8660254037844387076, 1.000000000000000000, 0.8660254037844387076, 1.000000000000000000, 0.8660254037844387076, 1.000000000000000000, 0.8660254037844387076, 1.000000000000000000, 0.8660254037844387076, 1.000000000000000000, 0.8660254037844387076, 1.000000000000000000, 0.8660254037844387076, 1.000000000000000000, 0.8660254037844387076, 1.000000000000000000, 0.8660254037844387076, 1.000000000000000000, 0.8660254037844387076, 1.000000000000000000, 0.8660254037844387076, 1.000000000000000000, 0.8660254037844387076, 1.000000000000000000, 0.8660254037844387076, 1.000000000000000000, 0.8660254037844387076, 1.000000000000000000, 0.8660254037844387076, 1.000000000000000000, 0.8660254037844387076, 1.000000000000000000, 0.8660254037844387076, 1.000000000000000000, 0.8660254037844387076, 1.000000000000000000, 0.8660254037844387076, 1.000000000000000000, 0.8660254037844387076, 1.000000000000000000, 0.8660254037844387076, 1.000000000000000000, 0.8660254037844387076, 1.000000000000000000, 0.8660254037844387076, 1.000000000000000000, 0.8660254037844387076, 1.000000000000000000, 0.8660254037844387076, 1.000000000000000000, 0.8660254037844387076, 1.000000000000000000, 0.8660254037844387076, 1.000000000000000000, 0.8660254037844387076, 1.000000000000000000, 0.8660254037844387076, 1.000000000000000000, 0.8660254037844387076, 1.000000000000000000, 0.8660254037844387076, 1.000000000000000000, 0.8660254037844387076, 1.000000000000000000, 0.8660254037844387076, 1.000000000000000000, 0.8660254037844387076, 1.000000000000000000, 0.8660254037844387076, 1.000000000000000000, 0.8660254037844387076, 1.000000000000000000, 0.8660254037844387076, 1.000000000000000000, 0.8660254037844387076, 1.000000000000000000, 0.8660254037844387076, 1.000000000000000000, 0.8660254037844387076, 1.000000000000000000, 0.8660254037844387076, 1.000000000000000000, 0.8660254037844387076, 1.000000000000000000, 0.8660254037844387076, 1.000000000000000000, 0.8660254037844387076, 1.000000000000000000, 0.8660254037844387076, 1.000000000000000000, 0.8660254037844387076, 1.000000000000000000, 0.8660254037844387076, 1.000000000000000000, 0.8660254037844387076, 1.000000000000000000, 0.8660254037844387076, 1.000000000000000000, 0.8660254037844387076, 1.000000000000000000, 0.8660254037844387076, 1.000000000000000000, 0.8660254037844387076, 1.000000000000000000, 0.8660254037844387076, 1.000000000000000000, 0.8660254037844387076, 1.000000000000000000, 0.8660254037844387076, 1.000000000000000000, 0.8660254037844387076, 1.000000000000000000, 0.8660254037844387076, 1.000000000000000000, 0.8660254037844387076, 1.000000000000000000, 0.8660254037844387076, 1.000000000000000000, 0.8660254037844387076, 1.000000000000000000, 0.8660254037844387076, 1.000000000000000000, 0.8660254037844387076, 1.000000000000000000, 0.8660254037844387076, 1.000000000000000000, 0.8660254037844387076, 1.000000000000000000, 0.8660254037844387076, 1.000000000000000000, 0.8660254037844387076, 1.000000000000000000, 0.8660254037844387076, 1.000000000000000000, 0.8660254037844387076, 1.000000000000000000, 0.8660254037844387076, 1.000000000000000000, 0.8660254037844387076, 1.000000000000000000, 0.8660254037844387076, 1.000000000000000000, 0.8660254037844387076, 1.000000000000000000, 0.8660254037844387076, 1.000000000000000000, 0.8660254037844387076, 1.000000000000000000, 0.8660254037844387076, 1.000000000000000000, 0.8660254037844387076, 1.000000000000000000, 0.8660254037844387076, 1.000000000000000000, 0.8660254037844387076, 1.000000000000000000, 0.8660254037844387076, 1.000000000000000000, 0.8660254037844387076, 1.000000000000000000, 0.8660254037844387076, 1.000000000000000000, 0.8660254037844387076, 1.000000000000000000, 0.8660254037844387076, 1.000000000000000000, 0.8660254037844387076, 1.000000000000000000, 0.8660254037844387076, 1.000000000000000000, 0.8660254037844387076, 1.000000000000000000, 0.8660254037844387076, 1.000000000000000000, 0.8660254037844387076, 1.000000000000000000, 0.8660254037844387076, 1.000000000000000000, 0.8660254037844387076, 1.000000000000000000, 0.8660254037844387076, 1.000000000000000000, 0.8660254037844387076, 1.000000000000000000, 0.8660254037844387076, 1.000000000000000000, 0.8660254037844387076, 1.000000000000000000, 0.8660254037844387076, 1.000000000000000000, 0.8660254037844387076, 1.000000000000000000, 0.8660254037844387076, 1.000000000000000000, 0.8660254037844387076, 1.000000000000000000, 0.8660254037844387076, 1.000000000000000000, 0.8660254037844387076, 1.000000000000000000) ) ) 
 REPRESENTATION_ITEM ( '' )  SURFACE ( )  );
#35471 = CARTESIAN_POINT ( 'NONE',  ( 26.31562500061451715, -6.054752690667223547, -1.112240025338166033E-15 ) ) ;
#35472 = CARTESIAN_POINT ( 'NONE',  ( 24.82499999999999929, 6.123233995736764310E-16, -4.999999999999998224 ) ) ;
#35473 = CARTESIAN_POINT ( 'NONE',  ( -3.999999999999999112, 15.16250000122903252, -30.00000000000000000 ) ) ;
#35474 = EDGE_CURVE ( 'NONE', #58564, #37474, #48927, .T. ) ;
#35475 = CARTESIAN_POINT ( 'NONE',  ( 29.09062500061451573, -3.027376345333610441, -5.243569643749999898 ) ) ;
#35476 = CARTESIAN_POINT ( 'NONE',  ( 11.20312500061451644, 4.541064518000418104, -2.621784821874998173 ) ) ;
#35477 = EDGE_LOOP ( 'NONE', ( #2959, #13324, #66476, #26123 ) ) ;
#35478 = CARTESIAN_POINT ( 'NONE',  ( 25.04062500061451502, -3.027376345333610441, -5.243569643749999898 ) ) ;
#35479 = CARTESIAN_POINT ( 'NONE',  ( 7.978125000614517681, 6.421520780324663323E-16, -5.243569643749999010 ) ) ;
#35480 = CARTESIAN_POINT ( 'NONE',  ( 4.040625000614517681, 6.054752690667223547, 3.707466751127219781E-16 ) ) ;
#35481 = CARTESIAN_POINT ( 'NONE',  ( 17.40937500061451715, -4.119189519843965641, -2.378215178125001383 ) ) ;
#35482 = ADVANCED_FACE ( 'NONE', ( #28506 ), #68398, .F. ) ;
#35483 = CARTESIAN_POINT ( 'NONE',  ( 30.00000000000000000, 0.000000000000000000, 0.000000000000000000 ) ) ;
#35484 = CARTESIAN_POINT ( 'NONE',  ( 12.71250000000000036, 2.886751345948129099, -4.999999999999998224 ) ) ;
#35485 =( BOUNDED_CURVE ( )  B_SPLINE_CURVE ( 2, ( #36563, #59820, #55023, #59083, #8487, #9225, #15120 ),
 .UNSPECIFIED., .F., .F. ) 
 B_SPLINE_CURVE_WITH_KNOTS ( ( 3, 2, 2, 3 ),
 ( 0.6500000000000000222, 0.6533333333333333215, 0.6566666666666666208, 0.6600000000000000311 ),
 .UNSPECIFIED. ) 
 CURVE ( )  GEOMETRIC_REPRESENTATION_ITEM ( )  RATIONAL_B_SPLINE_CURVE ( ( 1.000000000000000000, 0.8660254037844387076, 1.000000000000000000, 0.8660254037844387076, 1.000000000000000000, 0.8660254037844387076, 1.000000000000000000 ) ) 
 REPRESENTATION_ITEM ( '' )  );
#35486 = CARTESIAN_POINT ( 'NONE',  ( 13.17187500061451999, 3.027376345333611329, 5.243569643749999010 ) ) ;
#35487 = CARTESIAN_POINT ( 'NONE',  ( 10.38750000122903572, -4.330127018922194537, 2.499999999999995559 ) ) ;
#35488 = CARTESIAN_POINT ( 'NONE',  ( 16.62187500061451573, 3.027376345333613106, -5.243569643749998122 ) ) ;
#35489 = CARTESIAN_POINT ( 'NONE',  ( 16.68750000000000000, -2.886751345948125991, -5.000000000000000000 ) ) ;
#35490 = CARTESIAN_POINT ( 'NONE',  ( 9.271875000614516082, -6.054752690667223547, -1.112240025338166033E-15 ) ) ;
#35491 = CARTESIAN_POINT ( 'NONE',  ( -2.121784821874999949, 12.52812500061451573, -33.67503911421598417 ) ) ;
#35492 = DIRECTION ( 'NONE',  ( -0.000000000000000000, -1.000000000000000000, -0.000000000000000000 ) ) ;
#35493 = CARTESIAN_POINT ( 'NONE',  ( 22.69687500061451502, -4.119189519843965641, -2.378215178125001383 ) ) ;
#35494 = DIRECTION ( 'NONE',  ( -1.000000000000000000, -0.000000000000000000, -0.000000000000000000 ) ) ;
#35495 = CARTESIAN_POINT ( 'NONE',  ( 24.66562500061451502, 3.027376345333613106, -5.243569643749998122 ) ) ;
#35496 = CARTESIAN_POINT ( 'NONE',  ( 11.17500000000000071, -4.330127018922194537, 2.499999999999995559 ) ) ;
#35497 = CARTESIAN_POINT ( 'NONE',  ( 27.68437500061451573, -4.541064518000419881, 2.621784821874995952 ) ) ;
#35498 = CARTESIAN_POINT ( 'NONE',  ( 23.28750000000000142, -2.886751345948129988, 4.999999999999997335 ) ) ;
#35499 = CARTESIAN_POINT ( 'NONE',  ( 6.778125000614518392, 4.541064518000418104, 2.621784821874999949 ) ) ;
#35500 = CARTESIAN_POINT ( 'NONE',  ( 25.58437500061451431, 5.492252693125287522, 3.363034840372157021E-16 ) ) ;
#35501 =( BOUNDED_CURVE ( )  B_SPLINE_CURVE ( 2, ( #71089, #14200, #8665, #53738, #26766, #59993, #54470 ),
 .UNSPECIFIED., .F., .F. ) 
 B_SPLINE_CURVE_WITH_KNOTS ( ( 3, 2, 2, 3 ),
 ( 0.8250000000000000666, 0.8277777777777778345, 0.8305555555555557135, 0.8333333333333334814 ),
 .UNSPECIFIED. ) 
 CURVE ( )  GEOMETRIC_REPRESENTATION_ITEM ( )  RATIONAL_B_SPLINE_CURVE ( ( 0.9999999999999946709, 0.8660254037844440367, 1.000000000000000000, 0.8660254037844387076, 1.000000000000000000, 0.8660254037844333785, 1.000000000000005329 ) ) 
 REPRESENTATION_ITEM ( '' )  );
#35502 = CARTESIAN_POINT ( 'NONE',  ( 15.98437500061451821, -4.541064518000419881, 2.621784821874995952 ) ) ;
#35503 = CARTESIAN_POINT ( 'NONE',  ( 12.12187500061451573, 4.119189519843966529, 2.378215178124999607 ) ) ;
#35504 = CARTESIAN_POINT ( 'NONE',  ( 3.065625000614517592, 3.027376345333613106, -5.243569643749998122 ) ) ;
#35505 = CARTESIAN_POINT ( 'NONE',  ( 8.109375000614518214, 4.541064518000418104, -2.621784821874998173 ) ) ;
#35506 = ORIENTED_EDGE ( 'NONE', *, *, #1706, .T. ) ;
#35507 = CARTESIAN_POINT ( 'NONE',  ( 19.32187500061451857, 3.027376345333613106, -5.243569643749998122 ) ) ;
#35508 = CARTESIAN_POINT ( 'NONE',  ( 21.48750000000000071, -2.886751345948130876, 4.999999999999996447 ) ) ;
#35509 = CARTESIAN_POINT ( 'NONE',  ( 26.84999999999999787, 0.000000000000000000, 4.999999999999998224 ) ) ;
#35510 = CARTESIAN_POINT ( 'NONE',  ( 3.300000000000000711, 4.330127018922192761, -2.499999999999997780 ) ) ;
#35511 = LINE ( 'NONE', #69861, #27835 ) ;
#35512 = CARTESIAN_POINT ( 'NONE',  ( 27.89999999999999858, -4.330127018922190985, -2.500000000000001332 ) ) ;
#35513 = EDGE_LOOP ( 'NONE', ( #17174, #41361, #34016, #44889 ) ) ;
#35514 = CARTESIAN_POINT ( 'NONE',  ( 11.13750000000000284, -2.886751345948129988, 4.999999999999997335 ) ) ;
#35515 = CARTESIAN_POINT ( 'NONE',  ( 11.93437500061451750, -2.746126346562642428, -4.756430356249999214 ) ) ;
#35516 = CARTESIAN_POINT ( 'NONE',  ( 25.19062500061451715, 6.054752690667223547, 3.707466751127219781E-16 ) ) ;
#35517 = CARTESIAN_POINT ( 'NONE',  ( 14.69999999999999929, 0.000000000000000000, 4.999999999999998224 ) ) ;
#35518 = CARTESIAN_POINT ( 'NONE',  ( 8.475000001229034297, 2.886751345948126879, 4.999999999999999112 ) ) ;
#35519 = CARTESIAN_POINT ( 'NONE',  ( 7.190625000614518036, 6.054752690667223547, 3.707466751127219781E-16 ) ) ;
#35520 = CARTESIAN_POINT ( 'NONE',  ( 22.76249999999999574, 2.886751345948126879, 4.999999999999999112 ) ) ;
#35521 = CARTESIAN_POINT ( 'NONE',  ( 20.65312500061451573, 4.541064518000418104, -2.621784821874998173 ) ) ;
#35522 = CARTESIAN_POINT ( 'NONE',  ( 4.072484567436527314, -2.900952432071136400, 4.105854893343868994 ) ) ;
#35523 = CARTESIAN_POINT ( 'NONE',  ( 24.78750000122903074, -4.330127018922194537, 2.499999999999995559 ) ) ;
#35524 = CARTESIAN_POINT ( 'NONE',  ( -1.878215178125001827, 17.44062499938548072, 33.25316411605952283 ) ) ;
#35525 = CARTESIAN_POINT ( 'NONE',  ( 5.850000000000001421, -4.330127018922190985, -2.500000000000001332 ) ) ;
#35526 = EDGE_LOOP ( 'NONE', ( #67566, #25619, #33217, #67516 ) ) ;
#35527 = CARTESIAN_POINT ( 'NONE',  ( 21.29062500061451502, -3.027376345333614438, 5.243569643749998122 ) ) ;
#35528 = CARTESIAN_POINT ( 'NONE',  ( 27.85312500061451502, 4.541064518000418104, -2.621784821874998173 ) ) ;
#35529 = CARTESIAN_POINT ( 'NONE',  ( 27.27187500061451431, -6.054752690667223547, -1.112240025338166033E-15 ) ) ;
#35530 = CARTESIAN_POINT ( 'NONE',  ( 14.35312500061451679, 4.541064518000418104, -2.621784821874998173 ) ) ;
#35531 = CARTESIAN_POINT ( 'NONE',  ( -4.243569643749999898, 9.865625000614594242, -32.45002607614398471 ) ) ;
#35532 = CARTESIAN_POINT ( 'NONE',  ( 25.01250000122903216, 4.330127018922192761, -2.499999999999997780 ) ) ;
#35533 = CARTESIAN_POINT ( 'NONE',  ( 21.15937500061451715, 4.119189519843966529, -2.378215178124998275 ) ) ;
#35534 = CARTESIAN_POINT ( 'NONE',  ( 17.61562500061451786, 3.027376345333611329, 5.243569643749999010 ) ) ;
#35535 = CARTESIAN_POINT ( 'NONE',  ( 1.071796769724489895, 14.57990381179669903, -34.00000000000000000 ) ) ;
#35536 = VECTOR ( 'NONE', #47917, 1000.000000000000000 ) ;
#35537 = CARTESIAN_POINT ( 'NONE',  ( 2.887500001229035274, 6.123233995736764310E-16, -4.999999999999998224 ) ) ;
#35538 = CARTESIAN_POINT ( 'NONE',  ( 10.39687500061451786, 6.054752690667223547, 3.707466751127219781E-16 ) ) ;
#35539 = CARTESIAN_POINT ( 'NONE',  ( 9.721875000614517148, -6.054752690667223547, -1.112240025338166033E-15 ) ) ;
#35540 = CARTESIAN_POINT ( 'NONE',  ( 18.87187500061451573, 3.027376345333613106, -5.243569643749998122 ) ) ;
#35541 = ORIENTED_EDGE ( 'NONE', *, *, #9144, .F. ) ;
#35542 = CARTESIAN_POINT ( 'NONE',  ( 9.862499999999997158, -5.773502691896255534, -1.060575238724906372E-15 ) ) ;
#35543 = CARTESIAN_POINT ( 'NONE',  ( 23.69062500061451004, -3.027376345333610441, -5.243569643749999898 ) ) ;
#35544 = CARTESIAN_POINT ( 'NONE',  ( 18.94687500061451502, 6.054752690667223547, 3.707466751127219781E-16 ) ) ;
#35545 = CARTESIAN_POINT ( 'NONE',  ( 25.56562500061452070, 3.027376345333613106, -5.243569643749998122 ) ) ;
#35546 = CARTESIAN_POINT ( 'NONE',  ( 7.556250001229035007, 0.000000000000000000, 4.999999999999998224 ) ) ;
#35547 = CARTESIAN_POINT ( 'NONE',  ( -3.999999999999999112, 14.60000000000000142, 30.00000000000000000 ) ) ;
#35548 = CARTESIAN_POINT ( 'NONE',  ( 29.57812500061451644, 6.421520780324663323E-16, -5.243569643749999010 ) ) ;
#35549 = CARTESIAN_POINT ( 'NONE',  ( 10.61250000122903536, 4.330127018922192761, -2.499999999999997780 ) ) ;
#35550 = CARTESIAN_POINT ( 'NONE',  ( 4.162500001229033408, -4.330127018922190985, -2.500000000000001332 ) ) ;
#35551 = CARTESIAN_POINT ( 'NONE',  ( -3.999999999999999112, 20.00000000000000000, -30.00000000000000000 ) ) ;
#35552 = CARTESIAN_POINT ( 'NONE',  ( 27.97500000122903074, -5.773502691896255534, -1.060575238724906372E-15 ) ) ;
#35553 = CARTESIAN_POINT ( 'NONE',  ( -3.756430356250000102, 13.42812499938548321, 30.00000000000000000 ) ) ;
#35554 = CARTESIAN_POINT ( 'NONE',  ( 9.759375000614516793, -4.541064518000417216, -2.621784821875001281 ) ) ;
#35555 = CARTESIAN_POINT ( 'NONE',  ( 9.375000000000001776, -4.330127018922194537, 2.499999999999995559 ) ) ;
#35556 = CARTESIAN_POINT ( 'NONE',  ( 17.42812500061451786, 6.421520780324663323E-16, -5.243569643749999010 ) ) ;
#35557 = CARTESIAN_POINT ( 'NONE',  ( 11.74687500061451573, 6.054752690667223547, 3.707466751127219781E-16 ) ) ;
#35558 = CARTESIAN_POINT ( 'NONE',  ( 29.43750000122903288, 6.123233995736764310E-16, -4.999999999999998224 ) ) ;
#35559 = CARTESIAN_POINT ( 'NONE',  ( 20.85937500061451644, 0.000000000000000000, 5.243569643749999010 ) ) ;
#35560 = CARTESIAN_POINT ( 'NONE',  ( 6.946875000614517681, -3.027376345333614438, 5.243569643749998122 ) ) ;
#35561 = CARTESIAN_POINT ( 'NONE',  ( 3.115864988711636752, -3.910524711353453142, -3.240904574695108842 ) ) ;
#35562 = CARTESIAN_POINT ( 'NONE',  ( -5.810221930991193690E-16, 14.03750000000000142, 26.00000000000000355 ) ) ;
#35563 = ADVANCED_FACE ( 'NONE', ( #12600 ), #57657, .T. ) ;
#35564 = CARTESIAN_POINT ( 'NONE',  ( 8.240625000614516082, -3.027376345333614438, 5.243569643749998122 ) ) ;
#35565 = CARTESIAN_POINT ( 'NONE',  ( 18.17812500061451786, -4.541064518000419881, 2.621784821874995952 ) ) ;
#35566 = VERTEX_POINT ( 'NONE', #34403 ) ;
#35567 = CARTESIAN_POINT ( 'NONE',  ( 6.075000001229034829, 2.886751345948129099, -4.999999999999998224 ) ) ;
#35568 = CARTESIAN_POINT ( 'NONE',  ( 13.71562500061451750, -6.054752690667223547, -1.112240025338166033E-15 ) ) ;
#35569 = CARTESIAN_POINT ( 'NONE',  ( 11.05312500061451608, -4.541064518000417216, -2.621784821875001281 ) ) ;
#35570 = CARTESIAN_POINT ( 'NONE',  ( 23.44687500061451502, 5.492252693125287522, 3.363034840372157021E-16 ) ) ;
#35571 = CARTESIAN_POINT ( 'NONE',  ( 13.79999999999999893, 0.000000000000000000, 4.999999999999998224 ) ) ;
#35572 = CARTESIAN_POINT ( 'NONE',  ( 7.500000001229034652, 5.773502691896255534, 3.535250795749688894E-16 ) ) ;
#35573 = CARTESIAN_POINT ( 'NONE',  ( 15.42187500061451821, 3.027376345333611329, 5.243569643749999010 ) ) ;
#35574 = CARTESIAN_POINT ( 'NONE',  ( 18.37500000122903288, 2.886751345948126879, 4.999999999999999112 ) ) ;
#35575 = CARTESIAN_POINT ( 'NONE',  ( 24.33749999999999858, -2.886751345948125991, -5.000000000000000000 ) ) ;
#35576 = CARTESIAN_POINT ( 'NONE',  ( -4.243569643749999898, 17.96562500061451573, -32.45002607614398471 ) ) ;
#35577 = CARTESIAN_POINT ( 'NONE',  ( 4.080569135018654592, -2.889455923578380769, -4.080569135022440896 ) ) ;
#35578 = CARTESIAN_POINT ( 'NONE',  ( 6.712500001229034119, 0.000000000000000000, 4.999999999999998224 ) ) ;
#35579 = EDGE_CURVE ( 'NONE', #44223, #25148, #29591, .T. ) ;
#35580 = CARTESIAN_POINT ( 'NONE',  ( 4.866467007518584076, 1.159079983394287972, 4.866467007518584076 ) ) ;
#35581 = CARTESIAN_POINT ( 'NONE',  ( 30.00000000000000000, 0.000000000000000000, 0.000000000000000000 ) ) ;
#35582 = CARTESIAN_POINT ( 'NONE',  ( 17.37187500061451573, -6.054752690667223547, -1.112240025338166033E-15 ) ) ;
#35583 =( GEOMETRIC_REPRESENTATION_CONTEXT ( 3 ) GLOBAL_UNCERTAINTY_ASSIGNED_CONTEXT ( ( #46212 ) ) GLOBAL_UNIT_ASSIGNED_CONTEXT ( ( #53730, #48556, #43747 ) ) REPRESENTATION_CONTEXT ( 'NONE', 'WORKASPACE' ) );
#35584 = CARTESIAN_POINT ( 'NONE',  ( 15.15000000000000036, 0.000000000000000000, 4.999999999999998224 ) ) ;
#35585 = CARTESIAN_POINT ( 'NONE',  ( 14.99062500061451786, -3.027376345333614438, 5.243569643749998122 ) ) ;
#35586 = CARTESIAN_POINT ( 'NONE',  ( 9.843750001229032875, -2.886751345948129988, 4.999999999999997335 ) ) ;
#35587 = DIRECTION ( 'NONE',  ( -1.000000000000000000, -0.000000000000000000, -0.000000000000000000 ) ) ;
#35588 = CARTESIAN_POINT ( 'NONE',  ( 26.33437500061451431, -4.541064518000419881, 2.621784821874995952 ) ) ;
#35589 = CARTESIAN_POINT ( 'NONE',  ( 17.93437500061451928, 5.492252693125287522, 3.363034840372157021E-16 ) ) ;
#35590 = CARTESIAN_POINT ( 'NONE',  ( 10.30312500061451431, 4.541064518000418104, -2.621784821874998173 ) ) ;
#35591 = CARTESIAN_POINT ( 'NONE',  ( 16.62187500061451573, 3.027376345333613106, -5.243569643749998122 ) ) ;
#35592 = EDGE_LOOP ( 'NONE', ( #68093, #64811, #46064, #52243 ) ) ;
#35593 = CARTESIAN_POINT ( 'NONE',  ( 26.61562500061451786, 3.027376345333611329, 5.243569643749999010 ) ) ;
#35594 = CARTESIAN_POINT ( 'NONE',  ( 19.56562500061451715, -6.054752690667223547, -1.112240025338166033E-15 ) ) ;
#35595 = CARTESIAN_POINT ( 'NONE',  ( 1.071796769724476572, 12.59509619066136921, -25.99999999999999289 ) ) ;
#35596 = ADVANCED_FACE ( 'NONE', ( #45510 ), #63203, .T. ) ;
#35597 = CARTESIAN_POINT ( 'NONE',  ( 9.262499999999999289, 2.886751345948126879, 4.999999999999999112 ) ) ;
#35598 = CARTESIAN_POINT ( 'NONE',  ( 20.10000000122903074, 5.773502691896255534, 3.535250795749688894E-16 ) ) ;
#35599 = CARTESIAN_POINT ( 'NONE',  ( -1.071796769724488563, 10.19240381056766687, 34.00000000000000000 ) ) ;
#35600 = CARTESIAN_POINT ( 'NONE',  ( 9.684375000614517504, -2.746126346562642428, -4.756430356249999214 ) ) ;
#35601 = ORIENTED_EDGE ( 'NONE', *, *, #35886, .F. ) ;
#35602 = CARTESIAN_POINT ( 'NONE',  ( 16.68750000000000000, -2.886751345948125991, -5.000000000000000000 ) ) ;
#35603 = CARTESIAN_POINT ( 'NONE',  ( 21.52499999999999858, -4.330127018922194537, 2.499999999999995559 ) ) ;
#35604 = CARTESIAN_POINT ( 'NONE',  ( 18.68437500061451928, -4.541064518000419881, 2.621784821874995952 ) ) ;
#35605 = CARTESIAN_POINT ( 'NONE',  ( 14.27812500061451573, 6.421520780324663323E-16, -5.243569643749999010 ) ) ;
#35606 = ORIENTED_EDGE ( 'NONE', *, *, #20857, .F. ) ;
#35607 = CYLINDRICAL_SURFACE ( 'NONE', #27774, 4.000000000000000000 ) ;
#35608 = CARTESIAN_POINT ( 'NONE',  ( 7.078125000614516438, 6.421520780324663323E-16, -5.243569643749999010 ) ) ;
#35609 = LINE ( 'NONE', #51529, #563 ) ;
#35610 = CARTESIAN_POINT ( 'NONE',  ( 12.59999999999999964, -4.330127018922190985, -2.500000000000001332 ) ) ;
#35611 = CARTESIAN_POINT ( 'NONE',  ( 28.84687500061451360, 0.000000000000000000, 4.756430356249998326 ) ) ;
#35612 = CARTESIAN_POINT ( 'NONE',  ( 4.243569643749999898, 18.64062500061451644, 32.45002607614398471 ) ) ;
#35613 = CARTESIAN_POINT ( 'NONE',  ( 3.009375000614516793, -4.541064518000417216, -2.621784821875001281 ) ) ;
#35614 = CARTESIAN_POINT ( 'NONE',  ( 7.762500000000001954, 2.886751345948129099, -4.999999999999998224 ) ) ;
#35615 = CARTESIAN_POINT ( 'NONE',  ( -7.967954043666661671E-16, 16.57812499938548356, 34.33755215474603517 ) ) ;
#35616 = CARTESIAN_POINT ( 'NONE',  ( 26.55937500061451573, 4.541064518000418104, -2.621784821874998173 ) ) ;
#35617 = ORIENTED_EDGE ( 'NONE', *, *, #60470, .F. ) ;
#35618 = CARTESIAN_POINT ( 'NONE',  ( 21.10312500061451502, 4.541064518000418104, -2.621784821874998173 ) ) ;
#35619 = CARTESIAN_POINT ( 'NONE',  ( 22.24687500061451217, -3.027376345333614438, 5.243569643749998122 ) ) ;
#35620 = CARTESIAN_POINT ( 'NONE',  ( 9.001249775931846008E-16, 15.41562500061459495, -25.09994784771203058 ) ) ;
#35621 = CARTESIAN_POINT ( 'NONE',  ( 5.765625000614519102, 3.027376345333613106, -5.243569643749998122 ) ) ;
#35622 = CARTESIAN_POINT ( 'NONE',  ( 28.28437500061451715, 5.824947211148865298E-16, -4.756430356249998326 ) ) ;
#35623 = CARTESIAN_POINT ( 'NONE',  ( 23.69062500061451004, -3.027376345333610441, -5.243569643749999898 ) ) ;
#35624 = CARTESIAN_POINT ( 'NONE',  ( 27.04687500061451289, 0.000000000000000000, 4.756430356249998326 ) ) ;
#35625 = CARTESIAN_POINT ( 'NONE',  ( 11.10937500061451644, -4.119189519843965641, -2.378215178125001383 ) ) ;
#35626 = CARTESIAN_POINT ( 'NONE',  ( 16.69687500061451502, 6.054752690667223547, 3.707466751127219781E-16 ) ) ;
#35627 = CARTESIAN_POINT ( 'NONE',  ( 18.45937500061451431, 4.541064518000418104, -2.621784821874998173 ) ) ;
#35628 = CARTESIAN_POINT ( 'NONE',  ( 28.02187500061451431, 3.027376345333611329, 5.243569643749999010 ) ) ;
#35629 = CARTESIAN_POINT ( 'NONE',  ( -4.243569643749998122, 15.84687500061451892, 32.45002607614398471 ) ) ;
#35630 = CARTESIAN_POINT ( 'NONE',  ( 6.515625000614516438, -6.054752690667223547, -1.112240025338166033E-15 ) ) ;
#35631 = CARTESIAN_POINT ( 'NONE',  ( 1.592000809091587073E-14, 16.28750000000000142, 26.00000000000000000 ) ) ;
#35632 = CARTESIAN_POINT ( 'NONE',  ( 4.696875000614518569, -3.027376345333614438, 5.243569643749998122 ) ) ;
#35633 = CARTESIAN_POINT ( 'NONE',  ( 1.999999999999997335, 17.37500000000000000, 33.46410161513775705 ) ) ;
#35634 = CARTESIAN_POINT ( 'NONE',  ( 4.678125000614516971, -4.541064518000419881, 2.621784821874995952 ) ) ;
#35635 = CARTESIAN_POINT ( 'NONE',  ( 9.796875000614519990, -3.027376345333610441, -5.243569643749999898 ) ) ;
#35636 = CARTESIAN_POINT ( 'NONE',  ( 17.32500000122903216, 2.886751345948129099, -4.999999999999998224 ) ) ;
#35637 = CARTESIAN_POINT ( 'NONE',  ( 4.959375000614516971, 4.541064518000418104, -2.621784821874998173 ) ) ;
#35638 = CARTESIAN_POINT ( 'NONE',  ( 8.203125000614518214, 0.000000000000000000, 5.243569643749999010 ) ) ;
#35639 = CARTESIAN_POINT ( 'NONE',  ( 4.000000000000000000, 13.38124999877096677, 27.69059892324149530 ) ) ;
#35640 = CARTESIAN_POINT ( 'NONE',  ( 24.28125000122903288, -4.330127018922194537, 2.499999999999995559 ) ) ;
#35641 = CARTESIAN_POINT ( 'NONE',  ( 16.32187500061451502, 3.027376345333611329, 5.243569643749999010 ) ) ;
#35642 = DIRECTION ( 'NONE',  ( -0.000000000000000000, -1.000000000000000000, -0.000000000000000000 ) ) ;
#35643 = ORIENTED_EDGE ( 'NONE', *, *, #22404, .T. ) ;
#35644 = CARTESIAN_POINT ( 'NONE',  ( 25.79062500061451502, -3.027376345333614438, 5.243569643749998122 ) ) ;
#35645 = CARTESIAN_POINT ( 'NONE',  ( 10.52812500061451750, -4.541064518000419881, 2.621784821874995952 ) ) ;
#35646 = CARTESIAN_POINT ( 'NONE',  ( 26.97187500061451004, 3.027376345333612662, -5.243569643749998122 ) ) ;
#35647 = CARTESIAN_POINT ( 'NONE',  ( 9.515625000614518214, 3.027376345333611329, 5.243569643749999010 ) ) ;
#35648 = CARTESIAN_POINT ( 'NONE',  ( 26.28750000122903430, 6.123233995736764310E-16, -4.999999999999998224 ) ) ;
#35649 =( BOUNDED_CURVE ( )  B_SPLINE_CURVE ( 2, ( #54138, #31601, #60022, #9434, #71493, #13868, #26422 ),
 .UNSPECIFIED., .F., .F. ) 
 B_SPLINE_CURVE_WITH_KNOTS ( ( 3, 2, 2, 3 ),
 ( 0.6333333333333333037, 0.6361111111111110716, 0.6388888888888889506, 0.6416666666666668295 ),
 .UNSPECIFIED. ) 
 CURVE ( )  GEOMETRIC_REPRESENTATION_ITEM ( )  RATIONAL_B_SPLINE_CURVE ( ( 1.000000000000000000, 0.8660254037844387076, 1.000000000000000000, 0.8660254037844387076, 1.000000000000000000, 0.8660254037844333785, 1.000000000000005329 ) ) 
 REPRESENTATION_ITEM ( '' )  );
#35650 = CARTESIAN_POINT ( 'NONE',  ( 10.35000000122903074, -2.886751345948129988, 4.999999999999997335 ) ) ;
#35651 = EDGE_CURVE ( 'NONE', #46824, #22963, #11335, .T. ) ;
#35652 = CARTESIAN_POINT ( 'NONE',  ( 24.44062500061451715, -3.027376345333614438, 5.243569643749998122 ) ) ;
#35653 = CARTESIAN_POINT ( 'NONE',  ( 4.243569643749999010, 13.31562500061451537, -32.45002607614398471 ) ) ;
#35654 = CARTESIAN_POINT ( 'NONE',  ( 11.58750000122903501, 4.330127018922191873, 2.499999999999999556 ) ) ;
#35655 = CARTESIAN_POINT ( 'NONE',  ( 22.26562500061451644, -6.054752690667223547, -1.112240025338166033E-15 ) ) ;
#35656 = CARTESIAN_POINT ( 'NONE',  ( 12.11250000000000249, -5.773502691896255534, -1.060575238724906372E-15 ) ) ;
#35657 = CARTESIAN_POINT ( 'NONE',  ( 20.35312500061451502, 0.000000000000000000, 5.243569643749999010 ) ) ;
#35658 = CARTESIAN_POINT ( 'NONE',  ( 29.85937500061451644, 0.000000000000000000, 4.756430356249998326 ) ) ;
#35659 = CARTESIAN_POINT ( 'NONE',  ( 20.10000000000000142, 0.000000000000000000, 4.999999999999998224 ) ) ;
#35660 = CARTESIAN_POINT ( 'NONE',  ( 13.80000000122903181, 5.773502691896255534, 3.535250795749688894E-16 ) ) ;
#35661 = CARTESIAN_POINT ( 'NONE',  ( 11.42812500061451608, -4.541064518000419881, 2.621784821874995952 ) ) ;
#35662 = CARTESIAN_POINT ( 'NONE',  ( 14.05312500061451431, 0.000000000000000000, 5.243569643749999010 ) ) ;
#35663 = CARTESIAN_POINT ( 'NONE',  ( 25.61250000122903359, 0.000000000000000000, 4.999999999999998224 ) ) ;
#35664 = CARTESIAN_POINT ( 'NONE',  ( 21.12187500061451573, 3.027376345333613106, -5.243569643749998122 ) ) ;
#35665 = CARTESIAN_POINT ( 'NONE',  ( 3.507483327083503521, -3.563363679198468859, 3.507483327083555924 ) ) ;
#35666 = CARTESIAN_POINT ( 'NONE',  ( 8.625000001229034652, -5.773502691896255534, -1.060575238724906372E-15 ) ) ;
#35667 = CARTESIAN_POINT ( 'NONE',  ( 8.784375000614518925, -4.541064518000419881, 2.621784821874995952 ) ) ;
#35668 = CARTESIAN_POINT ( 'NONE',  ( 26.03437500061451715, 6.421520780324663323E-16, -5.243569643749999010 ) ) ;
#35669 = CARTESIAN_POINT ( 'NONE',  ( 30.00000000000000000, 0.000000000000000000, 0.000000000000000000 ) ) ;
#35670 = CARTESIAN_POINT ( 'NONE',  ( 20.35312500061451502, 0.000000000000000000, 5.243569643749999010 ) ) ;
#35671 = CARTESIAN_POINT ( 'NONE',  ( 26.44687500061451502, -3.027376345333610441, -5.243569643749999898 ) ) ;
#35672 = CARTESIAN_POINT ( 'NONE',  ( 3.756430356249998770, 17.66562499938548214, 32.16877607737301759 ) ) ;
#35673 = CARTESIAN_POINT ( 'NONE',  ( 18.59999999999999787, 4.330127018922192761, -2.499999999999997780 ) ) ;
#35674 = CARTESIAN_POINT ( 'NONE',  ( 8.184375000614515727, 4.541064518000418104, 2.621784821874999949 ) ) ;
#35675 = CARTESIAN_POINT ( 'NONE',  ( 17.76562500061451644, -6.054752690667223547, -1.112240025338166033E-15 ) ) ;
#35676 = ORIENTED_EDGE ( 'NONE', *, *, #49591, .F. ) ;
#35677 = CARTESIAN_POINT ( 'NONE',  ( -3.999999999999999112, 12.80000000000000071, -30.00000000000000000 ) ) ;
#35678 = CARTESIAN_POINT ( 'NONE',  ( 28.56562500061451715, -6.054752690667223547, -1.112240025338166033E-15 ) ) ;
#35679 = CARTESIAN_POINT ( 'NONE',  ( 3.984375000614517326, 6.421520780324663323E-16, -5.243569643749999010 ) ) ;
#35680 = CARTESIAN_POINT ( 'NONE',  ( 12.28125000122903110, 6.123233995736764310E-16, -4.999999999999998224 ) ) ;
#35681 = EDGE_CURVE ( 'NONE', #66787, #37790, #65813, .T. ) ;
#35682 = LINE ( 'NONE', #58204, #12347 ) ;
#35683 = CARTESIAN_POINT ( 'NONE',  ( 17.84999999999999787, 0.000000000000000000, 4.999999999999998224 ) ) ;
#35684 = CARTESIAN_POINT ( 'NONE',  ( 21.47812500061451502, 6.421520780324663323E-16, -5.243569643749999010 ) ) ;
#35685 = ORIENTED_EDGE ( 'NONE', *, *, #41825, .T. ) ;
#35686 = CARTESIAN_POINT ( 'NONE',  ( 25.34999999999999787, 4.330127018922192761, -2.499999999999997780 ) ) ;
#35687 =( BOUNDED_CURVE ( )  B_SPLINE_CURVE ( 2, ( #22354, #21990, #50077, #44549, #67080, #16439, #33435 ),
 .UNSPECIFIED., .F., .F. ) 
 B_SPLINE_CURVE_WITH_KNOTS ( ( 3, 2, 2, 3 ),
 ( 0.8750000000000000000, 0.8777777777777777679, 0.8805555555555555358, 0.8833333333333333037 ),
 .UNSPECIFIED. ) 
 CURVE ( )  GEOMETRIC_REPRESENTATION_ITEM ( )  RATIONAL_B_SPLINE_CURVE ( ( 1.000000000000000000, 0.8660254037844387076, 1.000000000000000000, 0.8660254037844387076, 1.000000000000000000, 0.8660254037844387076, 1.000000000000000000 ) ) 
 REPRESENTATION_ITEM ( '' )  );
#35688 = CARTESIAN_POINT ( 'NONE',  ( 26.48437500061451644, 6.421520780324663323E-16, -5.243569643749999010 ) ) ;
#35689 = ORIENTED_EDGE ( 'NONE', *, *, #531, .F. ) ;
#35690 = VECTOR ( 'NONE', #41509, 1000.000000000000000 ) ;
#35691 = CARTESIAN_POINT ( 'NONE',  ( 13.56562500061451892, 3.027376345333611329, 5.243569643749999010 ) ) ;
#35692 = CARTESIAN_POINT ( 'NONE',  ( 5.840625000614516615, 6.054752690667223547, 3.707466751127219781E-16 ) ) ;
#35693 = CARTESIAN_POINT ( 'NONE',  ( 16.92187500061451644, 5.824947211148865298E-16, -4.756430356249998326 ) ) ;
#35694 = CARTESIAN_POINT ( 'NONE',  ( 3.234375000614516438, 4.541064518000418104, 2.621784821874999949 ) ) ;
#35695 = CARTESIAN_POINT ( 'NONE',  ( 16.08750000122903501, 4.330127018922191873, 2.499999999999999556 ) ) ;
#35696 = CARTESIAN_POINT ( 'NONE',  ( 20.40000000000000213, 4.330127018922192761, -2.499999999999997780 ) ) ;
#35697 = CARTESIAN_POINT ( 'NONE',  ( 28.98750000000000071, 5.773502691896255534, 3.535250795749688894E-16 ) ) ;
#35698 = CARTESIAN_POINT ( 'NONE',  ( 3.834375000614519635, -4.541064518000419881, 2.621784821874995952 ) ) ;
#35699 = CARTESIAN_POINT ( 'NONE',  ( 10.05937500061451750, 0.000000000000000000, 5.243569643749999010 ) ) ;
#35700 = CARTESIAN_POINT ( 'NONE',  ( 18.57187500061451857, 3.027376345333611329, 5.243569643749999010 ) ) ;
#35701 = ORIENTED_EDGE ( 'NONE', *, *, #30976, .T. ) ;
#35702 = CARTESIAN_POINT ( 'NONE',  ( 2.896875000614518747, -3.027376345333614438, 5.243569643749998122 ) ) ;
#35703 = CARTESIAN_POINT ( 'NONE',  ( 4.349999999999999645, 0.000000000000000000, 4.999999999999998224 ) ) ;
#35704 = CARTESIAN_POINT ( 'NONE',  ( 4.359375000614517326, -4.541064518000417216, -2.621784821875001281 ) ) ;
#35705 = CARTESIAN_POINT ( 'NONE',  ( 15.18750000000000000, -2.886751345948129988, 4.999999999999997335 ) ) ;
#35706 = CARTESIAN_POINT ( 'NONE',  ( 13.00312500061451537, 4.541064518000418104, -2.621784821874998173 ) ) ;
#35707 = CARTESIAN_POINT ( 'NONE',  ( -4.000000000000000000, 19.02499999999999858, 30.00000000000000000 ) ) ;
#35708 = CARTESIAN_POINT ( 'NONE',  ( 8.456250001229033586, 0.000000000000000000, 4.999999999999998224 ) ) ;
#35709 = CARTESIAN_POINT ( 'NONE',  ( 18.60000000122903430, -2.886751345948125991, -5.000000000000000000 ) ) ;
#35710 = CARTESIAN_POINT ( 'NONE',  ( -3.999999999999999112, 19.38124999877096144, 27.69059892324149530 ) ) ;
#35711 = CARTESIAN_POINT ( 'NONE',  ( 19.58437500061451786, -4.119189519843968306, 2.378215178124996054 ) ) ;
#35712 = CARTESIAN_POINT ( 'NONE',  ( 8.503125000614515372, 4.541064518000418104, -2.621784821874998173 ) ) ;
#35713 = CARTESIAN_POINT ( 'NONE',  ( 24.42187500061451999, 3.027376345333611329, 5.243569643749999010 ) ) ;
#35714 = CARTESIAN_POINT ( 'NONE',  ( 19.57500000122903216, 2.886751345948129099, -4.999999999999997335 ) ) ;
#35715 = CARTESIAN_POINT ( 'NONE',  ( 25.65937500061451715, 4.541064518000418104, -2.621784821874998173 ) ) ;
#35716 = CARTESIAN_POINT ( 'NONE',  ( 8.025000000000000355, -4.330127018922194537, 2.499999999999995559 ) ) ;
#35717 = CARTESIAN_POINT ( 'NONE',  ( -2.000000000000000000, 12.38750000122903394, 26.53589838486224650 ) ) ;
#35718 = CARTESIAN_POINT ( 'NONE',  ( 14.24062500061451608, -3.027376345333610441, -5.243569643749999898 ) ) ;
#35719 = CARTESIAN_POINT ( 'NONE',  ( 5.850000001229035185, -2.886751345948129988, 4.999999999999997335 ) ) ;
#35720 = CARTESIAN_POINT ( 'NONE',  ( 17.78437500061451715, -4.541064518000419881, 2.621784821874995952 ) ) ;
#35721 = CARTESIAN_POINT ( 'NONE',  ( 10.92187500061451644, 3.027376345333611329, 5.243569643749999010 ) ) ;
#35722 = FACE_OUTER_BOUND ( 'NONE', #71628, .T. ) ;
#35723 = EDGE_LOOP ( 'NONE', ( #42695, #780, #56798, #32030 ) ) ;
#35724 = CARTESIAN_POINT ( 'NONE',  ( 11.35312500061451679, 0.000000000000000000, 5.243569643749999010 ) ) ;
#35725 = CARTESIAN_POINT ( 'NONE',  ( 29.02500000122903145, 2.886751345948160630, -4.999999999999943157 ) ) ;
#35726 = CARTESIAN_POINT ( 'NONE',  ( 23.02500000122903145, -5.773502691896255534, -1.060575238724906372E-15 ) ) ;
#35727 = CARTESIAN_POINT ( 'NONE',  ( 13.50937500061451679, 4.541064518000418104, -2.621784821874998173 ) ) ;
#35728 = CARTESIAN_POINT ( 'NONE',  ( 15.14062500061451644, -3.027376345333610441, -5.243569643749999898 ) ) ;
#35729 = CARTESIAN_POINT ( 'NONE',  ( 11.66250000122903430, 0.000000000000000000, 4.999999999999998224 ) ) ;
#35730 = CARTESIAN_POINT ( 'NONE',  ( 25.09687500061451715, -3.027376345333610441, -5.243569643749999898 ) ) ;
#35731 = DIRECTION ( 'NONE',  ( 0.000000000000000000, 0.000000000000000000, 1.000000000000000000 ) ) ;
#35732 = EDGE_CURVE ( 'NONE', #8380, #47360, #56931, .T. ) ;
#35733 = CARTESIAN_POINT ( 'NONE',  ( 7.650000000000000355, -4.330127018922190985, -2.500000000000001332 ) ) ;
#35734 = FACE_OUTER_BOUND ( 'NONE', #61060, .T. ) ;
#35735 = CARTESIAN_POINT ( 'NONE',  ( 2.121784821874999061, 16.10937500061451644, -33.67503911421598417 ) ) ;
#35736 = CARTESIAN_POINT ( 'NONE',  ( 16.09687500061452070, -3.027376345333610441, -5.243569643749999898 ) ) ;
#35737 = CARTESIAN_POINT ( 'NONE',  ( 18.41250000122903430, 0.000000000000000000, 4.999999999999998224 ) ) ;
#35738 = EDGE_CURVE ( 'NONE', #37161, #58014, #41946, .T. ) ;
#35739 = CARTESIAN_POINT ( 'NONE',  ( 12.98437500061451821, 6.421520780324663323E-16, -5.243569643749999010 ) ) ;
#35740 = CARTESIAN_POINT ( 'NONE',  ( 4.243569643749999010, 19.16562500061451857, -32.45002607614398471 ) ) ;
#35741 = CARTESIAN_POINT ( 'NONE',  ( 20.73750000122903359, -4.330127018922194537, 2.499999999999995559 ) ) ;
#35742 = CARTESIAN_POINT ( 'NONE',  ( 13.67812500061451786, -4.541064518000419881, 2.621784821874995952 ) ) ;
#35743 = VERTEX_POINT ( 'NONE', #12955 ) ;
#35744 = EDGE_LOOP ( 'NONE', ( #65011, #48077, #40572, #66160 ) ) ;
#35745 = CARTESIAN_POINT ( 'NONE',  ( 18.89999999999999858, -4.330127018922190985, -2.500000000000001332 ) ) ;
#35746 = CARTESIAN_POINT ( 'NONE',  ( 13.54687500061451821, 6.054752690667223547, 3.707466751127219781E-16 ) ) ;
#35747 = DIRECTION ( 'NONE',  ( 0.000000000000000000, 0.000000000000000000, 1.000000000000000000 ) ) ;
#35748 = CARTESIAN_POINT ( 'NONE',  ( 11.66250000122903430, 0.000000000000000000, 4.999999999999998224 ) ) ;
#35749 = CARTESIAN_POINT ( 'NONE',  ( 21.93750000122903288, 4.330127018922191873, 2.499999999999999556 ) ) ;
#35750 = CARTESIAN_POINT ( 'NONE',  ( 17.31562500061451715, -6.054752690667223547, -1.112240025338166033E-15 ) ) ;
#35751 = CARTESIAN_POINT ( 'NONE',  ( 23.46562500061451573, 3.027376345333611329, 5.243569643749999010 ) ) ;
#35752 = CARTESIAN_POINT ( 'NONE',  ( 4.153125000614515727, 0.000000000000000000, 5.243569643749999010 ) ) ;
#35753 = CARTESIAN_POINT ( 'NONE',  ( 27.15000000000000213, 4.330127018922192761, -2.499999999999997780 ) ) ;
#35754 = CARTESIAN_POINT ( 'NONE',  ( 5.000000000001367795, -0.3826438005438348444, -5.034765704839666789 ) ) ;
#35755 = CARTESIAN_POINT ( 'NONE',  ( 28.76249999999999929, -5.773502691896255534, -1.060575238724906372E-15 ) ) ;
#35756 = FACE_OUTER_BOUND ( 'NONE', #34924, .T. ) ;
#35757 = CARTESIAN_POINT ( 'NONE',  ( -5.810221930991193690E-16, 14.48749999999999893, -34.00000000000000000 ) ) ;
#35758 = CARTESIAN_POINT ( 'NONE',  ( 2.121784821874999061, 17.00937500061451857, -33.67503911421598417 ) ) ;
#35759 = CARTESIAN_POINT ( 'NONE',  ( 4.312500001229034652, 4.330127018922192761, -2.499999999999997780 ) ) ;
#35760 = CARTESIAN_POINT ( 'NONE',  ( 5.175000000000002487, 4.330127018922191873, 2.499999999999999556 ) ) ;
#35761 = CARTESIAN_POINT ( 'NONE',  ( 3.695974187897780983, 4.072863115247815635, 3.432733439617522642 ) ) ;
#35762 = CARTESIAN_POINT ( 'NONE',  ( 10.47187500061451715, 3.027376345333611329, 5.243569643749999010 ) ) ;
#35763 = CARTESIAN_POINT ( 'NONE',  ( 29.46562500061451573, -6.054752690667223547, -1.112240025338166033E-15 ) ) ;
#35764 = DIRECTION ( 'NONE',  ( -0.000000000000000000, -1.000000000000000000, -0.000000000000000000 ) ) ;
#35765 = DIRECTION ( 'NONE',  ( 0.000000000000000000, 0.000000000000000000, 1.000000000000000000 ) ) ;
#35766 = CYLINDRICAL_SURFACE ( 'NONE', #64242, 4.999999999999998224 ) ;
#35767 = CARTESIAN_POINT ( 'NONE',  ( 6.834375000614518747, 4.541064518000418104, 2.621784821874999949 ) ) ;
#35768 = CARTESIAN_POINT ( 'NONE',  ( 10.09687500061451715, -3.027376345333614438, 5.243569643749998122 ) ) ;
#35769 = CARTESIAN_POINT ( 'NONE',  ( 5.850000000000001421, -4.330127018922190985, -2.500000000000001332 ) ) ;
#35770 = CARTESIAN_POINT ( 'NONE',  ( 2.121784821875001281, 15.90312500061459211, 33.67503911421598417 ) ) ;
#35771 = CARTESIAN_POINT ( 'NONE',  ( 1.292354794015584840, 25.48750161887817711, 33.79447915781519640 ) ) ;
#35772 = CARTESIAN_POINT ( 'NONE',  ( 7.650000000000000355, -4.330127018922190985, -2.500000000000001332 ) ) ;
#35773 = CARTESIAN_POINT ( 'NONE',  ( 16.20937500061451431, 2.746126346562643317, 4.756430356249998326 ) ) ;
#35774 = CARTESIAN_POINT ( 'NONE',  ( 19.22812500061451502, 6.421520780324663323E-16, -5.243569643749999010 ) ) ;
#35775 = CARTESIAN_POINT ( 'NONE',  ( 12.55312500061451786, 4.541064518000418104, -2.621784821874998173 ) ) ;
#35776 = CARTESIAN_POINT ( 'NONE',  ( 24.83437500061451075, -2.746126346562646425, 4.756430356249996549 ) ) ;
#35777 = CARTESIAN_POINT ( 'NONE',  ( 10.47187500061451715, 3.027376345333611329, 5.243569643749999010 ) ) ;
#35778 = CARTESIAN_POINT ( 'NONE',  ( 26.69999999999999929, 4.330127018922192761, -2.499999999999997780 ) ) ;
#35779 = CARTESIAN_POINT ( 'NONE',  ( 23.13750000122903216, 6.123233995736764310E-16, -4.999999999999998224 ) ) ;
#35780 = CARTESIAN_POINT ( 'NONE',  ( 11.82187500061451679, 3.027376345333611329, 5.243569643749999010 ) ) ;
#35781 = CARTESIAN_POINT ( 'NONE',  ( 25.62187500061451573, 3.027376345333613106, -5.243569643749998122 ) ) ;
#35782 = CARTESIAN_POINT ( 'NONE',  ( 21.76875000122904069, 2.886751345948073588, -5.000000000000094147 ) ) ;
#35783 = CARTESIAN_POINT ( 'NONE',  ( 24.48750000122903359, 6.123233995736764310E-16, -4.999999999999998224 ) ) ;
#35784 = CARTESIAN_POINT ( 'NONE',  ( 18.79687500061451644, -3.027376345333610441, -5.243569643749999898 ) ) ;
#35785 = CARTESIAN_POINT ( 'NONE',  ( 11.78437500061451892, 4.541064518000418104, 2.621784821874999949 ) ) ;
#35786 = CARTESIAN_POINT ( 'NONE',  ( 1.878215178124997609, 18.52812499938548285, 33.25316411605952993 ) ) ;
#35787 = CARTESIAN_POINT ( 'NONE',  ( 23.92499999999999716, 6.123233995736764310E-16, -4.999999999999998224 ) ) ;
#35788 = CARTESIAN_POINT ( 'NONE',  ( 3.756430356250000546, 19.87812499938548427, 27.83122392262697886 ) ) ;
#35789 = CARTESIAN_POINT ( 'NONE',  ( 2.121784821874999061, 11.15937500061451715, -33.67503911421598417 ) ) ;
#35790 = CARTESIAN_POINT ( 'NONE',  ( 26.33437500061451431, -4.119189519843968306, 2.378215178124996054 ) ) ;
#35791 = CARTESIAN_POINT ( 'NONE',  ( 15.66562500061451857, 3.027376345333613106, -5.243569643749998122 ) ) ;
#35792 = CARTESIAN_POINT ( 'NONE',  ( 4.275000000000001243, 4.330127018922191873, 2.499999999999999556 ) ) ;
#35793 = LINE ( 'NONE', #40998, #33723 ) ;
#35794 = CARTESIAN_POINT ( 'NONE',  ( 1.626862140677534273E-15, 14.26250000000000107, -26.00000000000000355 ) ) ;
#35795 = CARTESIAN_POINT ( 'NONE',  ( 14.66249999999999964, 2.886751345948126879, 4.999999999999999112 ) ) ;
#35796 = CARTESIAN_POINT ( 'NONE',  ( -3.999999999999999556, 19.17500000122903359, 27.69059892324149530 ) ) ;
#35797 = CARTESIAN_POINT ( 'NONE',  ( 14.66250000122903252, 4.330127018922192761, -2.499999999999997780 ) ) ;
#35798 = EDGE_CURVE ( 'NONE', #23511, #50673, #67677, .T. ) ;
#35799 = CARTESIAN_POINT ( 'NONE',  ( 25.17187500061451644, 3.027376345333613106, -5.243569643749998122 ) ) ;
#35800 = ORIENTED_EDGE ( 'NONE', *, *, #4284, .F. ) ;
#35801 = CARTESIAN_POINT ( 'NONE',  ( 19.26562500061451644, 3.027376345333613106, -5.243569643749998122 ) ) ;
#35802 = CARTESIAN_POINT ( 'NONE',  ( 4.040625000614517681, 6.054752690667223547, 3.707466751127219781E-16 ) ) ;
#35803 = CARTESIAN_POINT ( 'NONE',  ( 19.24687500061452283, -3.027376345333610441, -5.243569643749999898 ) ) ;
#35804 = CARTESIAN_POINT ( 'NONE',  ( 3.825000000000001954, 4.330127018922191873, 2.499999999999999556 ) ) ;
#35805 = CARTESIAN_POINT ( 'NONE',  ( 6.590625000614518392, -3.027376345333610441, -5.243569643749999898 ) ) ;
#35806 = CARTESIAN_POINT ( 'NONE',  ( 20.95312500061451999, -4.541064518000417216, -2.621784821875001281 ) ) ;
#35807 = CARTESIAN_POINT ( 'NONE',  ( 4.243569643749999010, 16.01562500061451644, 27.54997392385601174 ) ) ;
#35808 = CARTESIAN_POINT ( 'NONE',  ( 18.33750000122903501, 4.330127018922191873, 2.499999999999999556 ) ) ;
#35809 = CARTESIAN_POINT ( 'NONE',  ( 11.29687500061451644, 5.492252693125287522, 3.363034840372157021E-16 ) ) ;
#35810 = CARTESIAN_POINT ( 'NONE',  ( 10.00312500061451715, 0.000000000000000000, 5.243569643749999010 ) ) ;
#35811 = CARTESIAN_POINT ( 'NONE',  ( 2.934375000614518392, -4.541064518000419881, 2.621784821874995952 ) ) ;
#35812 = CARTESIAN_POINT ( 'NONE',  ( 29.27812500061451573, 4.541064518000418104, 2.621784821874999949 ) ) ;
#35813 = CARTESIAN_POINT ( 'NONE',  ( 22.09687500061451715, 6.054752690667223547, 3.707466751127219781E-16 ) ) ;
#35814 = CARTESIAN_POINT ( 'NONE',  ( 15.70312500061451644, 4.541064518000418104, -2.621784821874998173 ) ) ;
#35815 = CARTESIAN_POINT ( 'NONE',  ( 24.11250000122903359, 4.330127018922192761, -2.499999999999997780 ) ) ;
#35816 = EDGE_CURVE ( 'NONE', #72158, #14259, #18839, .T. ) ;
#35817 = CARTESIAN_POINT ( 'NONE',  ( 24.62812500061451715, 6.421520780324663323E-16, -5.243569643749999010 ) ) ;
#35818 = CARTESIAN_POINT ( 'NONE',  ( 19.39687500061451786, 6.054752690667223547, 3.707466751127219781E-16 ) ) ;
#35819 = CARTESIAN_POINT ( 'NONE',  ( 14.80312500061451608, 4.541064518000418104, -2.621784821874998173 ) ) ;
#35820 = CARTESIAN_POINT ( 'NONE',  ( 2.121784821874999061, 17.00937500061451857, 26.32496088578401583 ) ) ;
#35821 = CARTESIAN_POINT ( 'NONE',  ( 21.06562500061451715, 3.027376345333613106, -5.243569643749998122 ) ) ;
#35822 = ORIENTED_EDGE ( 'NONE', *, *, #69064, .F. ) ;
#35823 = CARTESIAN_POINT ( 'NONE',  ( 24.93750000000000355, 5.773502691896255534, 3.535250795749688894E-16 ) ) ;
#35824 = CARTESIAN_POINT ( 'NONE',  ( 2.000000000000001332, 10.25000000000000000, -26.53589838486224650 ) ) ;
#35825 = CARTESIAN_POINT ( 'NONE',  ( 3.756430356250000102, 19.95312499938548356, 30.00000000000000000 ) ) ;
#35826 = CARTESIAN_POINT ( 'NONE',  ( 27.77812500061451573, 6.421520780324663323E-16, -5.243569643749999010 ) ) ;
#35827 = CARTESIAN_POINT ( 'NONE',  ( 7.453125000614516438, -4.541064518000417216, -2.621784821875001281 ) ) ;
#35828 = CARTESIAN_POINT ( 'NONE',  ( 18.71250000122903145, 4.330127018922192761, -2.499999999999997780 ) ) ;
#35829 = CARTESIAN_POINT ( 'NONE',  ( 28.30312500061451431, 4.541064518000418104, -2.621784821874998173 ) ) ;
#35830 = CARTESIAN_POINT ( 'NONE',  ( 24.22500000000000142, -4.330127018922194537, 2.499999999999995559 ) ) ;
#35831 = CARTESIAN_POINT ( 'NONE',  ( -2.000000000000000000, 15.53750000122903430, -33.46410161513775705 ) ) ;
#35832 = CARTESIAN_POINT ( 'NONE',  ( 29.27812500061451573, 4.541064518000418104, 2.621784821874999949 ) ) ;
#35833 = CARTESIAN_POINT ( 'NONE',  ( 10.64062500061451644, -3.027376345333610441, -5.243569643749999898 ) ) ;
#35834 = ORIENTED_EDGE ( 'NONE', *, *, #10973, .T. ) ;
#35835 = CARTESIAN_POINT ( 'NONE',  ( 24.74062500061451786, 6.054752690667223547, 3.707466751127219781E-16 ) ) ;
#35836 = CARTESIAN_POINT ( 'NONE',  ( 8.615625000614517859, 3.027376345333611329, 5.243569643749999010 ) ) ;
#35837 = CARTESIAN_POINT ( 'NONE',  ( 3.553125000614516082, 4.541064518000418104, -2.621784821874998173 ) ) ;
#35838 = CARTESIAN_POINT ( 'NONE',  ( 17.07187500061451502, 2.746126346562645981, -4.756430356249997438 ) ) ;
#35839 = CARTESIAN_POINT ( 'NONE',  ( 0.000000000000000000, 20.00000000000000000, -30.00000000000000000 ) ) ;
#35840 = CARTESIAN_POINT ( 'NONE',  ( 12.52500000000000213, -4.330127018922194537, 2.499999999999995559 ) ) ;
#35841 =( BOUNDED_CURVE ( )  B_SPLINE_CURVE ( 2, ( #21629, #48261, #26827, #31995, #65607, #31259, #44187, #37532, #49361 ),
 .UNSPECIFIED., .F., .F. ) 
 B_SPLINE_CURVE_WITH_KNOTS ( ( 3, 2, 2, 2, 3 ),
 ( 0.2361111111111111049, 0.2407407407407407274, 0.2500000000000000000, 0.2592592592592592449, 0.2638888888888888951 ),
 .UNSPECIFIED. ) 
 CURVE ( )  GEOMETRIC_REPRESENTATION_ITEM ( )  RATIONAL_B_SPLINE_CURVE ( ( 0.9330127018922194093, 0.9330127018922194093, 1.000000000000000000, 0.8660254037844387076, 1.000000000000000000, 0.8660254037844387076, 1.000000000000000000, 0.9330127018922194093, 0.9330127018922194093 ) ) 
 REPRESENTATION_ITEM ( '' )  );
#35842 = CARTESIAN_POINT ( 'NONE',  ( 12.49687500061451573, -3.027376345333610441, -5.243569643749999898 ) ) ;
#35843 = CARTESIAN_POINT ( 'NONE',  ( 9.937500001229032875, -4.330127018922194537, 2.499999999999995559 ) ) ;
#35844 = CARTESIAN_POINT ( 'NONE',  ( 16.80937500061451573, 0.000000000000000000, 5.243569643749999010 ) ) ;
#35845 = CARTESIAN_POINT ( 'NONE',  ( 17.73750000000000071, 5.773502691896255534, 3.535250795749688894E-16 ) ) ;
#35846 = CARTESIAN_POINT ( 'NONE',  ( 7.434375000614519280, -4.541064518000419881, 2.621784821874995952 ) ) ;
#35847 = CARTESIAN_POINT ( 'NONE',  ( -4.243569643749999898, 12.56562500061451715, -32.45002607614398471 ) ) ;
#35848 = CIRCLE ( 'NONE', #15823, 1.500000000000000888 ) ;
#35849 = CARTESIAN_POINT ( 'NONE',  ( 24.48750000122903359, 6.123233995736764310E-16, -4.999999999999998224 ) ) ;
#35850 = CARTESIAN_POINT ( 'NONE',  ( 22.43437500061451573, 5.492252693125287522, 3.363034840372157021E-16 ) ) ;
#35851 = EDGE_LOOP ( 'NONE', ( #10083, #51658, #29577, #45454 ) ) ;
#35852 = CARTESIAN_POINT ( 'NONE',  ( 23.50312500061451360, 0.000000000000000000, 5.243569643749999010 ) ) ;
#35853 = CARTESIAN_POINT ( 'NONE',  ( 21.18750000122903288, -4.330127018922194537, 2.499999999999995559 ) ) ;
#35854 = CARTESIAN_POINT ( 'NONE',  ( 26.67187500061451644, 3.027376345333611329, 5.243569643749999010 ) ) ;
#35855 = CARTESIAN_POINT ( 'NONE',  ( 29.07187500061451502, -6.054752690667223547, -1.112240025338166033E-15 ) ) ;
#35856 = CARTESIAN_POINT ( 'NONE',  ( 21.97500000000000142, -4.330127018922194537, 2.499999999999995559 ) ) ;
#35857 = CARTESIAN_POINT ( 'NONE',  ( 6.478125000614516793, -4.541064518000419881, 2.621784821874995952 ) ) ;
#35858 = CARTESIAN_POINT ( 'NONE',  ( 22.43437500061451217, 5.492252693125287522, 3.363034840372157021E-16 ) ) ;
#35859 = CARTESIAN_POINT ( 'NONE',  ( 17.25937500061451502, 0.000000000000000000, 5.243569643749999010 ) ) ;
#35860 = CARTESIAN_POINT ( 'NONE',  ( 9.759375000614516793, 2.746126346562645981, -4.756430356249997438 ) ) ;
#35861 = CARTESIAN_POINT ( 'NONE',  ( 3.590625000614518836, 6.054752690667223547, 3.707466751127219781E-16 ) ) ;
#35862 = CARTESIAN_POINT ( 'NONE',  ( 7.396875000614519635, -3.027376345333614438, 5.243569643749998122 ) ) ;
#35863 = EDGE_LOOP ( 'NONE', ( #21842, #49247, #47521, #6225, #66606, #21997, #47369, #32198, #72877, #41302, #792, #28495, #53034, #24952, #68652, #59674, #48835, #13145, #10297, #36840, #8918, #27810, #58631, #63600, #46421, #42334, #33929, #61987, #34417, #32589, #64759, #42348, #52524, #32354, #11542, #68386, #37894, #53098, #4276, #34737, #32982, #41600, #47701, #18614, #72591, #62558, #10230, #43436 ) ) ;
#35864 = CARTESIAN_POINT ( 'NONE',  ( 19.65937500061451360, -4.541064518000417216, -2.621784821875001281 ) ) ;
#35865 = CARTESIAN_POINT ( 'NONE',  ( -3.974286678381309112, 25.00691767267703725, 29.47675606540910209 ) ) ;
#35866 = CARTESIAN_POINT ( 'NONE',  ( 27.67499999999999716, 4.330127018922191873, 2.499999999999999556 ) ) ;
#35867 = CARTESIAN_POINT ( 'NONE',  ( 27.49687500061451217, 6.054752690667223547, 3.707466751127219781E-16 ) ) ;
#35868 = CARTESIAN_POINT ( 'NONE',  ( 12.50625000122903430, 0.000000000000000000, 4.999999999999998224 ) ) ;
#35869 = ORIENTED_EDGE ( 'NONE', *, *, #43284, .F. ) ;
#35870 = CARTESIAN_POINT ( 'NONE',  ( 10.23750000000000071, -2.886751345948129988, 4.999999999999997335 ) ) ;
#35871 = CARTESIAN_POINT ( 'NONE',  ( 11.52187500061451608, 5.824947211148865298E-16, -4.756430356249998326 ) ) ;
#35872 = CARTESIAN_POINT ( 'NONE',  ( 22.26562500061451644, -6.054752690667223547, -1.112240025338166033E-15 ) ) ;
#35873 = CARTESIAN_POINT ( 'NONE',  ( 12.82499999999999929, 4.330127018922191873, 2.499999999999999556 ) ) ;
#35874 = CARTESIAN_POINT ( 'NONE',  ( 9.225000001229034297, 2.886751345948129099, -4.999999999999998224 ) ) ;
#35875 = CARTESIAN_POINT ( 'NONE',  ( 5.465625000614517504, 3.027376345333611329, 5.243569643749999010 ) ) ;
#35876 = CARTESIAN_POINT ( 'NONE',  ( 22.83749999999999858, -2.886751345948129988, 4.999999999999997335 ) ) ;
#35877 = CARTESIAN_POINT ( 'NONE',  ( 20.39062500061451644, -3.027376345333614438, 5.243569643749998122 ) ) ;
#35878 = CARTESIAN_POINT ( 'NONE',  ( 23.51249999999999929, 2.886751345948112668, -5.000000000000024869 ) ) ;
#35879 = CARTESIAN_POINT ( 'NONE',  ( 24.48750000122903359, 6.123233995736764310E-16, -4.999999999999998224 ) ) ;
#35880 = CARTESIAN_POINT ( 'NONE',  ( 2.655984681222220721E-16, 19.95312499938548356, 25.66244784525396483 ) ) ;
#35881 = CARTESIAN_POINT ( 'NONE',  ( 5.362500000000003375, -5.773502691896255534, -1.060575238724906372E-15 ) ) ;
#35882 = ORIENTED_EDGE ( 'NONE', *, *, #19281, .F. ) ;
#35883 = CARTESIAN_POINT ( 'NONE',  ( 19.60312500061451502, -4.541064518000417216, -2.621784821875001281 ) ) ;
#35884 = CARTESIAN_POINT ( 'NONE',  ( 26.09062500061451573, 6.054752690667223547, 3.707466751127219781E-16 ) ) ;
#35885 = CARTESIAN_POINT ( 'NONE',  ( 26.67187500061451644, 3.027376345333611329, 5.243569643749999010 ) ) ;
#35886 = EDGE_CURVE ( 'NONE', #58433, #44258, #9379, .T. ) ;
#35887 = CARTESIAN_POINT ( 'NONE',  ( 14.46562500061451750, 3.027376345333611329, 5.243569643749999010 ) ) ;
#35888 = CARTESIAN_POINT ( 'NONE',  ( 9.515625000614518214, 3.027376345333611329, 5.243569643749999010 ) ) ;
#35889 = CARTESIAN_POINT ( 'NONE',  ( 12.13125000122903430, -4.330127018922194537, 2.499999999999995559 ) ) ;
#35890 =( BOUNDED_SURFACE ( )  B_SPLINE_SURFACE ( 1, 2, ( 
 ( #14187, #53351, #2749, #70345, #25268, #19350, #54458, #36722, #60342, #30460, #64432, #19721, #15283, #41907, #37088, #13824, #64796, #3116, #71078, #3857, #42273, #48551, #14552, #26379, #36364, #58878, #47815, #71449, #59243, #8652, #25646, #70707, #48183, #42638, #65162, #24903, #20824, #14920, #59612, #43379, #65903, #8288, #30818, #37823, #9026, #31557, #52989, #9391, #54097, #47448, #3494, #69980, #26012, #65534, #37462, #59981, #55553, #61450, #71819, #16016, #72178, #32652, #50016, #66267, #141, #21191, #5307, #45197, #67728, #17102, #10844, #72540, #38931, #50383, #67015, #15644, #27483, #39662, #4588, #10122, #33378, #55914, #27852, #16376, #5674, #43742, #22647, #38564, #4949, #27117, #10485, #21928, #38185, #60709, #55193, #72908, #66638, #22290, #61087, #16740, #44484, #44112, #61809, #9751, #32285, #44842, #67377, #49651, #33014, #21558, #39295, #11212, #33739, #56285, #28210, #50739, #54819, #4225, #26753, #49286, #1948, #40739, #51817, #11931, #12285, #17461, #7113, #45564, #52180, #34818, #56633, #69180, #34093, #23369, #28921, #40020, #28563, #68449, #23726, #18897, #69538, #34456, #45917, #6754, #17811, #56984, #6388, #51459, #862, #51098, #63615, #40372, #62181, #11578, #23004, #62890, #47003, #495, #68815, #68095, #57348, #29287, #29642, #35543, #1220, #1582, #46276, #13005, #62534, #18171, #63256, #58063, #12648, #35183, #57708, #24091, #46638, #18541, #41105, #6029, #29998, #7472, #52539, #24454, #14831, #47362, #19259, #65440, #3024, #19996, #26292, #20366, #41814, #58425, #13736, #71359, #25557, #37373, #70259, #14467, #14096, #42549, #30374, #47720, #30731, #64344, #8566, #24816, #31834, #52903, #37000, #3767, #48829, #41459, #65076, #31094, #70621, #8936, #48098, #69894, #59158, #63977, #36278, #58792, #59523, #31466, #54010, #3405, #59896, #2301, #54372, #19631, #36636, #8202, #42187, #53633, #53263, #2661, #25178, #64712, #25926, #48466, #70990, #42917, #9302, #13360, #35901, #7837, #66178, #5586, #60252, #22203, #26666, #16291, #43292, #9667, #54734, #15554, #4136, #44397, #38846, #61361, #10758, #44757, #33648, #32200, #21833, #49200, #5216, #39206, #33290, #55828, #71733, #21103, #28123, #65812, #50651, #43655, #32928, #49563, #27757, #4858, #38098, #60620, #10030, #15194, #27032, #66923, #66544, #67292, #50298, #27392, #32565, #37733, #55103, #4503, #72084, #21467, #44021, #15923, #10396, #72820, #16650, #38473, #60997, #20733, #55466, #49924, #72448, #61720, #11119, #56192, #51369, #35453, #68003, #63533, #17376, #62807, #29556, #63168, #52092, #56896, #18087, #69092, #5938, #46188, #23279, #28830, #57977, #57622, #7025, #39567, #28472, #40648, #12563, #12200, #45829, #18454, #45108, #1497, #11485, #68365, #68727, #34728, #34008, #22561, #35097, #7385, #23642, #24003, #67644, #46551, #29198, #41018, #12920, #29915, #55, #17010, #62092, #39933, #57257, #56545, #6670, #51008, #405, #22914, #45471, #62447, #11845, #34364, #6302, #51732, #771, #17727, #1133, #40286, #35814, #41375, #24368, #58705, #53542, #25092, #3314, #42468, #36551, #30283, #1861, #46916, #24731, #47274, #58336, #8116, #69808, #42103, #64991, #70539, #2572, #19173, #37285, #64255, #36187, #52455, #31380, #64625, #19545, #30644, #14743, #41728, #42830, #13643, #14012, #8844, #14381, #53920, #53175, #19914, #48378, #7747, #25467, #47635, #70169, #59808, #36916, #59436, #18811, #52816, #25841, #70905, #59071, #8475, #20277, #69454, #65353, #63885, #31009, #48011, #2938, #13276, #2218, #9213, #40124, #56382, #17207, #3680, #62285, #61915, #34196, #39768, #22750, #45300, #604, #6132, #50118, #44941, #54286, #22392, #67834, #11680, #67119, #5049, #10950, #67479, #50841, #5775, #33116, #22030, #56730, #28306, #39034, #27585, #17563, #71267, #28663, #38670, #241, #26204, #21658, #66748, #72648, #16118, #51202, #23110, #45667, #68200, #62639, #31749, #44216, #33841, #61193, #48743, #10588, #55653, #44587, #61548, #16476, #33471, #56019, #5411, #27950, #50482, #73008, #16842, #39396, #11320, #57087, #13460, #23476, #35285, #7571, #24193, #46022, #34559, #30107, #19364, #35645, #69637, #6495, #41560, #41207, #36008, #18999, #2048, #24559, #53004, #58527, #29391, #46747, #29030, #1684, #47105, #64078, #46382, #57453, #63365, #69281, #52641, #58167, #12390, #1322, #7937, #30475, #18273, #6857, #69995, #51566, #2399, #17917, #24920, #966, #68558, #40480, #51925, #62995, #47462, #41922, #12034, #34926, #23831, #68916, #40847, #13107, #12749, #57807, #7216, #29745, #52282, #18643, #63715, #49301, #13839, #71835, #42289, #3508, #20097, #26394, #48566, #25286, #47832, #53367, #36378, #70722, #65548, #37102, #15298, #54473, #71092, #64813, #58894, #8304, #36739, #59259, #70362, #42654, #8668, #54110, #3871, #9406, #14569, #31199, #21205, #3134, #48199, #64447, #43395, #26027, #31571, #65178, #26769, #53741, #54835, #25663, #20466, #20841, #48936, #65917, #59628, #31936, #60357, #19739, #37476, #9041, #4242, #30834, #43020, #14937, #14203, #59996, #71465, #37837, #9766, #32300, #2764, #38200, #50753, #15661, #4964, #10502, #21574, #10137, #50031, #5325, #512, #51115, #16032, #27497, #61465, #72556, #66655, #38580, #33030, #61104, #32669, #45212, #21944, #43758, #66283, #4603, #55569, #28578, #55210, #50398, #27134, #44499, #16391, #11230, #17118, #67032, #61825, #27866, #67746, #49667, #72195, #38947, #39677, #10860, #33393, #55929, #72923, #22305, #44857, #67393, #60726, #11593, #28223, #16755, #62197, #34110, #44128, #39313, #56649, #33753, #56298, #5688, #22662, #156, #6044, #68465, #52918, #57723, #69554, #51833, #69195, #68831, #1596, #11947, #29303, #12301, #45934, #63272, #6407, #13375, #34472, #18555, #58442, #7853, #30389, #24107, #12664, #52195, #63631, #7128 ),
 ( #57000, #17827, #28939, #46655, #41120, #13020, #35558, #24472, #46290, #41474, #68111, #47019, #51476, #18187, #58078, #35200, #878, #45579, #7486, #23023, #30015, #52558, #17477, #1964, #18914, #63994, #35917, #40037, #62551, #23385, #40388, #62907, #29658, #34837, #57363, #6770, #1237, #23742, #40757, #53649, #65092, #20381, #48481, #2677, #64727, #54387, #25941, #8581, #47737, #60268, #41830, #3782, #8218, #71005, #24831, #64361, #36293, #70276, #58807, #42932, #65456, #14849, #37388, #26307, #15210, #13751, #3421, #30746, #59912, #20750, #9318, #31851, #53278, #25193, #9682, #47379, #32215, #19647, #14482, #31110, #48845, #59540, #42203, #14112, #36652, #69909, #3042, #71375, #48113, #43308, #65828, #8950, #59173, #19276, #25573, #70636, #20011, #42564, #37016, #31484, #54026, #37750, #2316, #4873, #21486, #39583, #66560, #38489, #54749, #33664, #44412, #21849, #32943, #17025, #49579, #45124, #72101, #66938, #11136, #44772, #56208, #61013, #72835, #50666, #60636, #27773, #27409, #10411, #62107, #39223, #61735, #21119, #10048, #22218, #67307, #16307, #38861, #44038, #55481, #4519, #49216, #22576, #5601, #61376, #28138, #70, #32582, #55120, #67659, #10773, #33306, #11500, #4151, #27048, #71749, #15940, #26683, #55844, #43672, #49940, #50313, #72464, #5232, #66195, #16665, #15573, #38115, #1149, #17391, #24382, #22928, #29571, #69468, #18826, #41389, #12577, #23658, #63182, #1512, #18101, #39948, #51748, #63901, #28845, #34379, #35111, #57635, #7041, #40662, #29929, #68018, #46930, #40300, #29212, #51384, #34743, #46202, #62461, #11859, #56911, #52107, #17741, #24016, #62822, #41032, #68743, #68380, #12934, #34022, #56559, #46565, #69107, #6316, #57273, #786, #18469, #23295, #63548, #6684, #28486, #35469, #5954, #12214, #45844, #57991, #419, #7401, #52469, #51023, #45486, #1876, #47650, #31023, #70182, #36201, #58719, #53190, #8131, #2232, #14756, #19560, #43218, #13291, #47289, #2587, #71282, #24745, #19929, #69823, #42116, #59086, #53935, #59823, #25106, #31395, #70554, #37300, #19189, #41742, #30658, #9228, #64640, #14026, #36566, #53557, #64270, #13659, #8490, #65006, #2954, #59452, #25482, #20291, #48028, #42483, #65367, #3694, #26219, #14394, #36931, #8859, #3330, #25856, #48393, #70921, #42846, #31765, #7762, #54302, #58351, #48758, #20660, #35828, #52830, #30298, #27318, #22487, #73105, #38025, #26958, #10321, #49485, #15482, #60548, #32491, #9955, #54658, #67215, #72016, #65738, #15123, #26587, #55026, #50578, #4061, #72376, #49127, #21392, #38394, #33212, #39128, #4429, #10682, #49850, #16576, #71656, #21029, #43948, #61643, #66471, #15848, #60918, #32853, #55390, #4784, #21756, #60183, #33571, #50218, #44317, #11045, #56119, #43582, #66103, #5511, #66847, #16217, #37660, #44684, #38770, #9592, #61289, #32124, #55751, #28050, #5145, #27680, #72744, #22129, #33933, #51298, #34291, #67931, #12131, #28399, #35385, #56476, #40577, #7317, #29848, #52384, #23575, #34658, #1065, #12498, #29130, #50937, #62739, #1790, #39865, #45395, #46120, #68657, #18021, #51663, #40950, #5867, #57908, #699, #40218, #62377, #45761, #63097, #35026, #63465, #333, #45037, #23208, #57187, #11776, #68297, #6600, #22843, #17657, #17304, #57554, #12852, #56823, #6956, #29487, #52024, #1426, #46482, #67572, #11416, #23933, #6230, #69020, #16937, #18383, #39492, #28758, #62014, #9139, #46848, #31676, #2149, #36479, #53104, #59359, #8404, #58269, #7676, #13209, #69388, #30578, #25396, #70096, #48304, #14308, #30933, #24660, #18743, #41307, #69737, #19106, #30212, #2501, #41661, #13943, #36844, #42395, #47566, #64183, #54209, #36116, #8043, #24300, #3239, #58998, #64552, #25024, #59731, #13571, #14666, #58636, #53474, #53845, #8771, #25767, #19472, #64917, #20203, #52744, #70468, #42030, #2866, #63817, #31305, #70829, #35748, #47206, #42758, #65278, #47939, #19844, #37209, #48667, #5061, #15036, #26870, #72293, #15763, #37573, #26128, #21671, #10961, #27231, #61205, #71193, #33128, #32770, #27598, #10600, #66761, #16133, #44601, #50130, #20942, #38302, #20566, #66386, #38685, #55665, #37940, #49039, #54940, #60831, #44229, #71568, #4345, #10237, #72662, #49768, #3974, #66018, #22041, #67132, #9868, #43493, #61559, #43124, #16488, #9506, #39045, #49401, #60097, #33482, #3606, #32036, #65647, #54571, #26497, #15398, #60459, #32400, #71932, #4701, #21307, #43861, #55307, #23488, #17930, #16853, #67490, #41839, #5424, #64369, #33851, #68213, #11692, #40493, #40136, #39409, #61927, #44952, #27963, #62296, #57100, #28675, #6872, #46035, #62651, #56395, #50494, #73020, #28316, #50853, #11333, #34208, #252, #45677, #68571, #978, #6145, #22760, #13760, #67847, #39780, #56032, #34940, #17574, #23123, #56742, #18288, #45312, #46395, #17219, #12048, #12405, #63009, #57466, #51215, #29404, #51938, #5785, #29044, #615, #34572, #22405, #1335, #23847, #6509, #51579, #68930, #37396, #59548, #42573, #71384, #8227, #54394, #2685, #65101, #20391, #8960, #25201, #58816, #42940, #37758, #71013, #59920, #30755, #31859, #3429, #3793, #9326, #14857, #26315, #20758, #48854, #59180, #31494, #36302, #25949, #43316, #65836, #20019, #48121, #15219, #65465, #14490, #31119, #53286, #64735, #60276, #8589, #47748, #48489, #53658, #70284, #19656, #3051, #42211, #14123, #36661, #25582, #70644, #37024, #54034, #41099, #12642, #62884, #68089, #57702, #22998, #29636, #12279, #34087, #46632, #11572, #856, #6382, #17456, #6022, #45911, #1214, #69532, #46997, #11925, #23363, #57342, #68442, #62528, #34450, #28915, #56978, #28557, #63609, #17805, #39656, #62175, #488, #51453, #24448, #51092, #46270, #45558, #40365, #34812, #7107, #13000, #6748, #52174, #23720, #35537, #40014, #29281, #51811, #58057, #68809, #18165 ) ),
 .UNSPECIFIED., .F., .F., .F. ) 
 B_SPLINE_SURFACE_WITH_KNOTS ( ( 2, 2 ),
 ( 3, 2, 2, 2, 2, 2, 2, 2, 2, 2, 2, 2, 2, 2, 2, 2, 2, 2, 2, 2, 2, 2, 2, 2, 2, 2, 2, 2, 2, 2, 2, 2, 2, 2, 2, 2, 2, 2, 2, 2, 2, 2, 2, 2, 2, 2, 2, 2, 2, 2, 2, 2, 2, 2, 2, 2, 2, 2, 2, 2, 2, 2, 2, 2, 2, 2, 2, 2, 2, 2, 2, 2, 2, 2, 2, 2, 2, 2, 2, 2, 2, 2, 2, 2, 2, 2, 2, 2, 2, 2, 2, 2, 2, 2, 2, 2, 2, 2, 2, 2, 2, 2, 2, 2, 2, 2, 2, 2, 2, 2, 2, 2, 2, 2, 2, 2, 2, 2, 2, 2, 2, 2, 2, 2, 2, 2, 2, 2, 2, 2, 2, 2, 2, 2, 2, 2, 2, 2, 2, 2, 2, 2, 2, 2, 2, 2, 2, 2, 2, 2, 2, 2, 2, 2, 2, 2, 2, 2, 2, 2, 2, 2, 2, 2, 2, 2, 2, 2, 2, 2, 2, 2, 2, 2, 2, 2, 2, 2, 2, 2, 2, 2, 2, 2, 2, 2, 2, 2, 2, 2, 2, 2, 2, 2, 2, 2, 2, 2, 2, 2, 2, 2, 2, 2, 2, 2, 2, 2, 2, 2, 2, 2, 2, 2, 2, 2, 2, 2, 2, 2, 2, 2, 2, 2, 2, 2, 2, 2, 2, 2, 2, 2, 2, 2, 2, 2, 2, 2, 2, 2, 2, 2, 2, 2, 2, 2, 2, 2, 2, 2, 2, 2, 2, 2, 2, 2, 2, 2, 2, 2, 2, 2, 2, 2, 2, 2, 2, 2, 2, 2, 2, 2, 2, 2, 2, 2, 2, 2, 2, 2, 2, 2, 2, 2, 2, 2, 2, 2, 2, 2, 2, 2, 2, 2, 2, 2, 2, 2, 2, 2, 2, 2, 2, 2, 2, 2, 2, 2, 2, 2, 2, 2, 2, 2, 2, 2, 2, 2, 2, 2, 2, 2, 2, 2, 2, 2, 2, 2, 2, 2, 2, 2, 2, 2, 2, 2, 2, 2, 2, 2, 2, 2, 2, 2, 2, 2, 2, 2, 2, 2, 2, 2, 2, 2, 2, 2, 2, 2, 2, 2, 3 ),
 ( 0.000000000000000000, 1.000000000000000000 ),
 ( 0.000000000000000000, 0.002777777777777777884, 0.005555555555555555768, 0.008333333333333333218, 0.01111111111111111154, 0.01388888888888888812, 0.01666666666666666644, 0.01944444444444444475, 0.02222222222222222307, 0.02500000000000000139, 0.02777777777777777624, 0.03055555555555555455, 0.03333333333333333287, 0.03611111111111110772, 0.03888888888888888951, 0.04166666666666666435, 0.04444444444444444614, 0.04722222222222222099, 0.05000000000000000278, 0.05277777777777777762, 0.05555555555555555247, 0.05833333333333333426, 0.06111111111111110911, 0.06388888888888888395, 0.06666666666666666574, 0.06944444444444444753, 0.07222222222222221544, 0.07499999999999999722, 0.07777777777777777901, 0.08055555555555556080, 0.08333333333333332871, 0.08611111111111111049, 0.08888888888888889228, 0.09166666666666666019, 0.09444444444444444198, 0.09722222222222222376, 0.1000000000000000056, 0.1027777777777777735, 0.1055555555555555552, 0.1083333333333333370, 0.1111111111111111049, 0.1138888888888888867, 0.1166666666666666685, 0.1194444444444444503, 0.1222222222222222182, 0.1250000000000000000, 0.1277777777777777679, 0.1305555555555555636, 0.1333333333333333315, 0.1361111111111110994, 0.1388888888888888951, 0.1416666666666666630, 0.1444444444444444309, 0.1472222222222222265, 0.1499999999999999944, 0.1527777777777777901, 0.1555555555555555580, 0.1583333333333333259, 0.1611111111111111216, 0.1638888888888888895, 0.1666666666666666574, 0.1694444444444444531, 0.1722222222222222210, 0.1749999999999999889, 0.1777777777777777846, 0.1805555555555555525, 0.1833333333333333204, 0.1861111111111111160, 0.1888888888888888840, 0.1916666666666666796, 0.1944444444444444475, 0.1972222222222222154, 0.2000000000000000111, 0.2027777777777777790, 0.2055555555555555469, 0.2083333333333333426, 0.2111111111111111105, 0.2138888888888888784, 0.2166666666666666741, 0.2194444444444444420, 0.2222222222222222099, 0.2250000000000000056, 0.2277777777777777735, 0.2305555555555555691, 0.2333333333333333370, 0.2361111111111111049, 0.2388888888888889006, 0.2416666666666666685, 0.2444444444444444364, 0.2472222222222222321, 0.2500000000000000000, 0.2527777777777777679, 0.2555555555555555358, 0.2583333333333333592, 0.2611111111111111271, 0.2638888888888888951, 0.2666666666666666630, 0.2694444444444444309, 0.2722222222222221988, 0.2750000000000000222, 0.2777777777777777901, 0.2805555555555555580, 0.2833333333333333259, 0.2861111111111110938, 0.2888888888888888618, 0.2916666666666666852, 0.2944444444444444531, 0.2972222222222222210, 0.2999999999999999889, 0.3027777777777777568, 0.3055555555555555802, 0.3083333333333333481, 0.3111111111111111160, 0.3138888888888888840, 0.3166666666666666519, 0.3194444444444444198, 0.3222222222222222432, 0.3250000000000000111, 0.3277777777777777790, 0.3305555555555555469, 0.3333333333333333148, 0.3361111111111111382, 0.3388888888888889062, 0.3416666666666666741, 0.3444444444444444420, 0.3472222222222222099, 0.3499999999999999778, 0.3527777777777778012, 0.3555555555555555691, 0.3583333333333333370, 0.3611111111111111049, 0.3638888888888888729, 0.3666666666666666408, 0.3694444444444444642, 0.3722222222222222321, 0.3750000000000000000, 0.3777777777777777679, 0.3805555555555555358, 0.3833333333333333592, 0.3861111111111111271, 0.3888888888888888951, 0.3916666666666666630, 0.3944444444444444309, 0.3972222222222221988, 0.4000000000000000222, 0.4027777777777777901, 0.4055555555555555580, 0.4083333333333333259, 0.4111111111111110938, 0.4138888888888888618, 0.4166666666666666852, 0.4194444444444444531, 0.4222222222222222210, 0.4249999999999999889, 0.4277777777777777568, 0.4305555555555555802, 0.4333333333333333481, 0.4361111111111111160, 0.4388888888888888840, 0.4416666666666666519, 0.4444444444444444198, 0.4472222222222222432, 0.4500000000000000111, 0.4527777777777777790, 0.4555555555555555469, 0.4583333333333333148, 0.4611111111111111382, 0.4638888888888889062, 0.4666666666666666741, 0.4694444444444444420, 0.4722222222222222099, 0.4749999999999999778, 0.4777777777777778012, 0.4805555555555555691, 0.4833333333333333370, 0.4861111111111111049, 0.4888888888888888729, 0.4916666666666666408, 0.4944444444444444642, 0.4972222222222222321, 0.5000000000000000000, 0.5027777777777777679, 0.5055555555555555358, 0.5083333333333333037, 0.5111111111111110716, 0.5138888888888888395, 0.5166666666666667185, 0.5194444444444444864, 0.5222222222222222543, 0.5250000000000000222, 0.5277777777777777901, 0.5305555555555555580, 0.5333333333333333259, 0.5361111111111110938, 0.5388888888888888618, 0.5416666666666666297, 0.5444444444444443976, 0.5472222222222222765, 0.5500000000000000444, 0.5527777777777778123, 0.5555555555555555802, 0.5583333333333333481, 0.5611111111111111160, 0.5638888888888888840, 0.5666666666666666519, 0.5694444444444444198, 0.5722222222222221877, 0.5749999999999999556, 0.5777777777777777235, 0.5805555555555556024, 0.5833333333333333703, 0.5861111111111111382, 0.5888888888888889062, 0.5916666666666666741, 0.5944444444444444420, 0.5972222222222222099, 0.5999999999999999778, 0.6027777777777777457, 0.6055555555555555136, 0.6083333333333332815, 0.6111111111111111605, 0.6138888888888889284, 0.6166666666666666963, 0.6194444444444444642, 0.6222222222222222321, 0.6250000000000000000, 0.6277777777777777679, 0.6305555555555555358, 0.6333333333333333037, 0.6361111111111110716, 0.6388888888888888395, 0.6416666666666667185, 0.6444444444444444864, 0.6472222222222222543, 0.6500000000000000222, 0.6527777777777777901, 0.6555555555555555580, 0.6583333333333333259, 0.6611111111111110938, 0.6638888888888888618, 0.6666666666666666297, 0.6694444444444443976, 0.6722222222222222765, 0.6750000000000000444, 0.6777777777777778123, 0.6805555555555555802, 0.6833333333333333481, 0.6861111111111111160, 0.6888888888888888840, 0.6916666666666666519, 0.6944444444444444198, 0.6972222222222221877, 0.6999999999999999556, 0.7027777777777777235, 0.7055555555555556024, 0.7083333333333333703, 0.7111111111111111382, 0.7138888888888889062, 0.7166666666666666741, 0.7194444444444444420, 0.7222222222222222099, 0.7249999999999999778, 0.7277777777777777457, 0.7305555555555555136, 0.7333333333333332815, 0.7361111111111111605, 0.7388888888888889284, 0.7416666666666666963, 0.7444444444444444642, 0.7472222222222222321, 0.7500000000000000000, 0.7527777777777777679, 0.7555555555555555358, 0.7583333333333333037, 0.7611111111111110716, 0.7638888888888888395, 0.7666666666666667185, 0.7694444444444444864, 0.7722222222222222543, 0.7750000000000000222, 0.7777777777777777901, 0.7805555555555555580, 0.7833333333333333259, 0.7861111111111110938, 0.7888888888888888618, 0.7916666666666666297, 0.7944444444444443976, 0.7972222222222222765, 0.8000000000000000444, 0.8027777777777778123, 0.8055555555555555802, 0.8083333333333333481, 0.8111111111111111160, 0.8138888888888888840, 0.8166666666666666519, 0.8194444444444444198, 0.8222222222222221877, 0.8249999999999999556, 0.8277777777777777235, 0.8305555555555556024, 0.8333333333333333703, 0.8361111111111111382, 0.8388888888888889062, 0.8416666666666666741, 0.8444444444444444420, 0.8472222222222222099, 0.8499999999999999778, 0.8527777777777777457, 0.8555555555555555136, 0.8583333333333332815, 0.8611111111111111605, 0.8638888888888889284, 0.8666666666666666963, 0.8694444444444444642, 0.8722222222222222321, 0.8750000000000000000, 0.8777777777777777679, 0.8805555555555555358, 0.8833333333333333037, 0.8861111111111110716, 0.8888888888888888395, 0.8916666666666667185, 0.8944444444444444864, 0.8972222222222222543, 0.9000000000000000222, 0.9027777777777777901, 0.9055555555555555580, 0.9083333333333333259, 0.9111111111111110938, 0.9138888888888888618, 0.9166666666666666297, 0.9194444444444443976, 0.9222222222222222765, 0.9250000000000000444, 0.9277777777777778123, 0.9305555555555555802, 0.9333333333333333481, 0.9361111111111111160, 0.9388888888888888840, 0.9416666666666666519, 0.9444444444444444198, 0.9472222222222221877, 0.9499999999999999556, 0.9527777777777777235, 0.9555555555555556024, 0.9583333333333333703, 0.9611111111111111382, 0.9638888888888889062, 0.9666666666666666741, 0.9694444444444444420, 0.9722222222222222099, 0.9749999999999999778, 0.9777777777777777457, 0.9805555555555555136, 0.9833333333333332815, 0.9861111111111111605, 0.9888888888888889284, 0.9916666666666666963, 0.9944444444444444642, 0.9972222222222222321, 1.000000000000000000 ),
 .UNSPECIFIED. ) 
 GEOMETRIC_REPRESENTATION_ITEM ( )  RATIONAL_B_SPLINE_SURFACE ( (
 ( 1.000000000000000000, 0.8660254037844387076, 1.000000000000000000, 0.8660254037844387076, 1.000000000000000000, 0.8660254037844387076, 1.000000000000000000, 0.8660254037844387076, 1.000000000000000000, 0.8660254037844387076, 1.000000000000000000, 0.8660254037844387076, 1.000000000000000000, 0.8660254037844387076, 1.000000000000000000, 0.8660254037844387076, 1.000000000000000000, 0.8660254037844387076, 1.000000000000000000, 0.8660254037844387076, 1.000000000000000000, 0.8660254037844387076, 1.000000000000000000, 0.8660254037844387076, 1.000000000000000000, 0.8660254037844387076, 1.000000000000000000, 0.8660254037844387076, 1.000000000000000000, 0.8660254037844387076, 1.000000000000000000, 0.8660254037844387076, 1.000000000000000000, 0.8660254037844387076, 1.000000000000000000, 0.8660254037844387076, 1.000000000000000000, 0.8660254037844387076, 1.000000000000000000, 0.8660254037844387076, 1.000000000000000000, 0.8660254037844387076, 1.000000000000000000, 0.8660254037844387076, 1.000000000000000000, 0.8660254037844387076, 1.000000000000000000, 0.8660254037844387076, 1.000000000000000000, 0.8660254037844387076, 1.000000000000000000, 0.8660254037844387076, 1.000000000000000000, 0.8660254037844387076, 1.000000000000000000, 0.8660254037844387076, 1.000000000000000000, 0.8660254037844387076, 1.000000000000000000, 0.8660254037844387076, 1.000000000000000000, 0.8660254037844387076, 1.000000000000000000, 0.8660254037844387076, 1.000000000000000000, 0.8660254037844387076, 1.000000000000000000, 0.8660254037844387076, 1.000000000000000000, 0.8660254037844387076, 1.000000000000000000, 0.8660254037844387076, 1.000000000000000000, 0.8660254037844387076, 1.000000000000000000, 0.8660254037844387076, 1.000000000000000000, 0.8660254037844387076, 1.000000000000000000, 0.8660254037844387076, 1.000000000000000000, 0.8660254037844387076, 1.000000000000000000, 0.8660254037844387076, 1.000000000000000000, 0.8660254037844387076, 1.000000000000000000, 0.8660254037844387076, 1.000000000000000000, 0.8660254037844387076, 1.000000000000000000, 0.8660254037844387076, 1.000000000000000000, 0.8660254037844387076, 1.000000000000000000, 0.8660254037844387076, 1.000000000000000000, 0.8660254037844387076, 1.000000000000000000, 0.8660254037844387076, 1.000000000000000000, 0.8660254037844387076, 1.000000000000000000, 0.8660254037844387076, 1.000000000000000000, 0.8660254037844387076, 1.000000000000000000, 0.8660254037844387076, 1.000000000000000000, 0.8660254037844387076, 1.000000000000000000, 0.8660254037844387076, 1.000000000000000000, 0.8660254037844387076, 1.000000000000000000, 0.8660254037844387076, 1.000000000000000000, 0.8660254037844387076, 1.000000000000000000, 0.8660254037844387076, 1.000000000000000000, 0.8660254037844387076, 1.000000000000000000, 0.8660254037844387076, 1.000000000000000000, 0.8660254037844387076, 1.000000000000000000, 0.8660254037844387076, 1.000000000000000000, 0.8660254037844387076, 1.000000000000000000, 0.8660254037844387076, 1.000000000000000000, 0.8660254037844387076, 1.000000000000000000, 0.8660254037844387076, 1.000000000000000000, 0.8660254037844387076, 1.000000000000000000, 0.8660254037844387076, 1.000000000000000000, 0.8660254037844387076, 1.000000000000000000, 0.8660254037844387076, 1.000000000000000000, 0.8660254037844387076, 1.000000000000000000, 0.8660254037844387076, 1.000000000000000000, 0.8660254037844387076, 1.000000000000000000, 0.8660254037844387076, 1.000000000000000000, 0.8660254037844387076, 1.000000000000000000, 0.8660254037844387076, 1.000000000000000000, 0.8660254037844387076, 1.000000000000000000, 0.8660254037844387076, 1.000000000000000000, 0.8660254037844387076, 1.000000000000000000, 0.8660254037844387076, 1.000000000000000000, 0.8660254037844387076, 1.000000000000000000, 0.8660254037844387076, 1.000000000000000000, 0.8660254037844387076, 1.000000000000000000, 0.8660254037844387076, 1.000000000000000000, 0.8660254037844387076, 1.000000000000000000, 0.8660254037844387076, 1.000000000000000000, 0.8660254037844387076, 1.000000000000000000, 0.8660254037844387076, 1.000000000000000000, 0.8660254037844387076, 1.000000000000000000, 0.8660254037844387076, 1.000000000000000000, 0.8660254037844387076, 1.000000000000000000, 0.8660254037844387076, 1.000000000000000000, 0.8660254037844387076, 1.000000000000000000, 0.8660254037844387076, 1.000000000000000000, 0.8660254037844387076, 1.000000000000000000, 0.8660254037844387076, 1.000000000000000000, 0.8660254037844387076, 1.000000000000000000, 0.8660254037844387076, 1.000000000000000000, 0.8660254037844387076, 1.000000000000000000, 0.8660254037844387076, 1.000000000000000000, 0.8660254037844387076, 1.000000000000000000, 0.8660254037844387076, 1.000000000000000000, 0.8660254037844387076, 1.000000000000000000, 0.8660254037844387076, 1.000000000000000000, 0.8660254037844387076, 1.000000000000000000, 0.8660254037844387076, 1.000000000000000000, 0.8660254037844387076, 1.000000000000000000, 0.8660254037844387076, 1.000000000000000000, 0.8660254037844387076, 1.000000000000000000, 0.8660254037844387076, 1.000000000000000000, 0.8660254037844387076, 1.000000000000000000, 0.8660254037844387076, 1.000000000000000000, 0.8660254037844387076, 1.000000000000000000, 0.8660254037844387076, 1.000000000000000000, 0.8660254037844387076, 1.000000000000000000, 0.8660254037844387076, 1.000000000000000000, 0.8660254037844387076, 1.000000000000000000, 0.8660254037844387076, 1.000000000000000000, 0.8660254037844387076, 1.000000000000000000, 0.8660254037844387076, 1.000000000000000000, 0.8660254037844387076, 1.000000000000000000, 0.8660254037844387076, 1.000000000000000000, 0.8660254037844387076, 1.000000000000000000, 0.8660254037844387076, 1.000000000000000000, 0.8660254037844387076, 1.000000000000000000, 0.8660254037844387076, 1.000000000000000000, 0.8660254037844387076, 1.000000000000000000, 0.8660254037844387076, 1.000000000000000000, 0.8660254037844387076, 1.000000000000000000, 0.8660254037844387076, 1.000000000000000000, 0.8660254037844387076, 1.000000000000000000, 0.8660254037844387076, 1.000000000000000000, 0.8660254037844387076, 1.000000000000000000, 0.8660254037844387076, 1.000000000000000000, 0.8660254037844387076, 1.000000000000000000, 0.8660254037844387076, 1.000000000000000000, 0.8660254037844387076, 1.000000000000000000, 0.8660254037844387076, 1.000000000000000000, 0.8660254037844387076, 1.000000000000000000, 0.8660254037844387076, 1.000000000000000000, 0.8660254037844387076, 1.000000000000000000, 0.8660254037844387076, 1.000000000000000000, 0.8660254037844387076, 1.000000000000000000, 0.8660254037844387076, 1.000000000000000000, 0.8660254037844387076, 1.000000000000000000, 0.8660254037844387076, 1.000000000000000000, 0.8660254037844387076, 1.000000000000000000, 0.8660254037844387076, 1.000000000000000000, 0.8660254037844387076, 1.000000000000000000, 0.8660254037844387076, 1.000000000000000000, 0.8660254037844387076, 1.000000000000000000, 0.8660254037844387076, 1.000000000000000000, 0.8660254037844387076, 1.000000000000000000, 0.8660254037844387076, 1.000000000000000000, 0.8660254037844387076, 1.000000000000000000, 0.8660254037844387076, 1.000000000000000000, 0.8660254037844387076, 1.000000000000000000, 0.8660254037844387076, 1.000000000000000000, 0.8660254037844387076, 1.000000000000000000, 0.8660254037844387076, 1.000000000000000000, 0.8660254037844387076, 1.000000000000000000, 0.8660254037844387076, 1.000000000000000000, 0.8660254037844387076, 1.000000000000000000, 0.8660254037844387076, 1.000000000000000000, 0.8660254037844387076, 1.000000000000000000, 0.8660254037844387076, 1.000000000000000000, 0.8660254037844387076, 1.000000000000000000, 0.8660254037844387076, 1.000000000000000000, 0.8660254037844387076, 1.000000000000000000, 0.8660254037844387076, 1.000000000000000000, 0.8660254037844387076, 1.000000000000000000, 0.8660254037844387076, 1.000000000000000000, 0.8660254037844387076, 1.000000000000000000, 0.8660254037844387076, 1.000000000000000000, 0.8660254037844387076, 1.000000000000000000, 0.8660254037844387076, 1.000000000000000000, 0.8660254037844387076, 1.000000000000000000, 0.8660254037844387076, 1.000000000000000000, 0.8660254037844387076, 1.000000000000000000, 0.8660254037844387076, 1.000000000000000000, 0.8660254037844387076, 1.000000000000000000, 0.8660254037844387076, 1.000000000000000000, 0.8660254037844387076, 1.000000000000000000, 0.8660254037844387076, 1.000000000000000000, 0.8660254037844387076, 1.000000000000000000, 0.8660254037844387076, 1.000000000000000000, 0.8660254037844387076, 1.000000000000000000, 0.8660254037844387076, 1.000000000000000000, 0.8660254037844387076, 1.000000000000000000, 0.8660254037844387076, 1.000000000000000000, 0.8660254037844387076, 1.000000000000000000, 0.8660254037844387076, 1.000000000000000000, 0.8660254037844387076, 1.000000000000000000, 0.8660254037844387076, 1.000000000000000000, 0.8660254037844387076, 1.000000000000000000, 0.8660254037844387076, 1.000000000000000000, 0.8660254037844387076, 1.000000000000000000, 0.8660254037844387076, 1.000000000000000000, 0.8660254037844387076, 1.000000000000000000, 0.8660254037844387076, 1.000000000000000000, 0.8660254037844387076, 1.000000000000000000, 0.8660254037844387076, 1.000000000000000000, 0.8660254037844387076, 1.000000000000000000, 0.8660254037844387076, 1.000000000000000000, 0.8660254037844387076, 1.000000000000000000, 0.8660254037844387076, 1.000000000000000000, 0.8660254037844387076, 1.000000000000000000, 0.8660254037844387076, 1.000000000000000000, 0.8660254037844387076, 1.000000000000000000, 0.8660254037844387076, 1.000000000000000000, 0.8660254037844387076, 1.000000000000000000, 0.8660254037844387076, 1.000000000000000000, 0.8660254037844387076, 1.000000000000000000, 0.8660254037844387076, 1.000000000000000000, 0.8660254037844387076, 1.000000000000000000, 0.8660254037844387076, 1.000000000000000000, 0.8660254037844387076, 1.000000000000000000, 0.8660254037844387076, 1.000000000000000000, 0.8660254037844387076, 1.000000000000000000, 0.8660254037844387076, 1.000000000000000000, 0.8660254037844387076, 1.000000000000000000, 0.8660254037844387076, 1.000000000000000000, 0.8660254037844387076, 1.000000000000000000, 0.8660254037844387076, 1.000000000000000000, 0.8660254037844387076, 1.000000000000000000, 0.8660254037844387076, 1.000000000000000000, 0.8660254037844387076, 1.000000000000000000, 0.8660254037844387076, 1.000000000000000000, 0.8660254037844387076, 1.000000000000000000, 0.8660254037844387076, 1.000000000000000000, 0.8660254037844387076, 1.000000000000000000, 0.8660254037844387076, 1.000000000000000000, 0.8660254037844387076, 1.000000000000000000, 0.8660254037844387076, 1.000000000000000000, 0.8660254037844387076, 1.000000000000000000, 0.8660254037844387076, 1.000000000000000000, 0.8660254037844387076, 1.000000000000000000, 0.8660254037844387076, 1.000000000000000000, 0.8660254037844387076, 1.000000000000000000, 0.8660254037844387076, 1.000000000000000000, 0.8660254037844387076, 1.000000000000000000, 0.8660254037844387076, 1.000000000000000000, 0.8660254037844387076, 1.000000000000000000, 0.8660254037844387076, 1.000000000000000000, 0.8660254037844387076, 1.000000000000000000, 0.8660254037844387076, 1.000000000000000000, 0.8660254037844387076, 1.000000000000000000, 0.8660254037844387076, 1.000000000000000000, 0.8660254037844387076, 1.000000000000000000, 0.8660254037844387076, 1.000000000000000000, 0.8660254037844387076, 1.000000000000000000, 0.8660254037844387076, 1.000000000000000000, 0.8660254037844387076, 1.000000000000000000, 0.8660254037844387076, 1.000000000000000000, 0.8660254037844387076, 1.000000000000000000, 0.8660254037844387076, 1.000000000000000000, 0.8660254037844387076, 1.000000000000000000, 0.8660254037844387076, 1.000000000000000000, 0.8660254037844387076, 1.000000000000000000, 0.8660254037844387076, 1.000000000000000000, 0.8660254037844387076, 1.000000000000000000, 0.8660254037844387076, 1.000000000000000000, 0.8660254037844387076, 1.000000000000000000, 0.8660254037844387076, 1.000000000000000000, 0.8660254037844387076, 1.000000000000000000, 0.8660254037844387076, 1.000000000000000000, 0.8660254037844387076, 1.000000000000000000, 0.8660254037844387076, 1.000000000000000000, 0.8660254037844387076, 1.000000000000000000, 0.8660254037844387076, 1.000000000000000000, 0.8660254037844387076, 1.000000000000000000, 0.8660254037844387076, 1.000000000000000000, 0.8660254037844387076, 1.000000000000000000, 0.8660254037844387076, 1.000000000000000000, 0.8660254037844387076, 1.000000000000000000, 0.8660254037844387076, 1.000000000000000000, 0.8660254037844387076, 1.000000000000000000, 0.8660254037844387076, 1.000000000000000000, 0.8660254037844387076, 1.000000000000000000, 0.8660254037844387076, 1.000000000000000000, 0.8660254037844387076, 1.000000000000000000, 0.8660254037844387076, 1.000000000000000000, 0.8660254037844387076, 1.000000000000000000, 0.8660254037844387076, 1.000000000000000000, 0.8660254037844387076, 1.000000000000000000, 0.8660254037844387076, 1.000000000000000000, 0.8660254037844387076, 1.000000000000000000, 0.8660254037844387076, 1.000000000000000000, 0.8660254037844387076, 1.000000000000000000, 0.8660254037844387076, 1.000000000000000000, 0.8660254037844387076, 1.000000000000000000, 0.8660254037844387076, 1.000000000000000000, 0.8660254037844387076, 1.000000000000000000, 0.8660254037844387076, 1.000000000000000000, 0.8660254037844387076, 1.000000000000000000, 0.8660254037844387076, 1.000000000000000000, 0.8660254037844387076, 1.000000000000000000, 0.8660254037844387076, 1.000000000000000000, 0.8660254037844387076, 1.000000000000000000, 0.8660254037844387076, 1.000000000000000000, 0.8660254037844387076, 1.000000000000000000, 0.8660254037844387076, 1.000000000000000000, 0.8660254037844387076, 1.000000000000000000, 0.8660254037844387076, 1.000000000000000000, 0.8660254037844387076, 1.000000000000000000, 0.8660254037844387076, 1.000000000000000000, 0.8660254037844387076, 1.000000000000000000, 0.8660254037844387076, 1.000000000000000000, 0.8660254037844387076, 1.000000000000000000, 0.8660254037844387076, 1.000000000000000000, 0.8660254037844387076, 1.000000000000000000, 0.8660254037844387076, 1.000000000000000000, 0.8660254037844387076, 1.000000000000000000, 0.8660254037844387076, 1.000000000000000000, 0.8660254037844387076, 1.000000000000000000, 0.8660254037844387076, 1.000000000000000000, 0.8660254037844387076, 1.000000000000000000, 0.8660254037844387076, 1.000000000000000000, 0.8660254037844387076, 1.000000000000000000, 0.8660254037844387076, 1.000000000000000000, 0.8660254037844387076, 1.000000000000000000, 0.8660254037844387076, 1.000000000000000000, 0.8660254037844387076, 1.000000000000000000, 0.8660254037844387076, 1.000000000000000000, 0.8660254037844387076, 1.000000000000000000, 0.8660254037844387076, 1.000000000000000000, 0.8660254037844387076, 1.000000000000000000, 0.8660254037844387076, 1.000000000000000000, 0.8660254037844387076, 1.000000000000000000, 0.8660254037844387076, 1.000000000000000000, 0.8660254037844387076, 1.000000000000000000, 0.8660254037844387076, 1.000000000000000000, 0.8660254037844387076, 1.000000000000000000, 0.8660254037844387076, 1.000000000000000000, 0.8660254037844387076, 1.000000000000000000, 0.8660254037844387076, 1.000000000000000000, 0.8660254037844387076, 1.000000000000000000, 0.8660254037844387076, 1.000000000000000000, 0.8660254037844387076, 1.000000000000000000, 0.8660254037844387076, 1.000000000000000000, 0.8660254037844387076, 1.000000000000000000, 0.8660254037844387076, 1.000000000000000000, 0.8660254037844387076, 1.000000000000000000, 0.8660254037844387076, 1.000000000000000000, 0.8660254037844387076, 1.000000000000000000, 0.8660254037844387076, 1.000000000000000000, 0.8660254037844387076, 1.000000000000000000, 0.8660254037844387076, 1.000000000000000000, 0.8660254037844387076, 1.000000000000000000, 0.8660254037844387076, 1.000000000000000000, 0.8660254037844387076, 1.000000000000000000, 0.8660254037844387076, 1.000000000000000000, 0.8660254037844387076, 1.000000000000000000, 0.8660254037844387076, 1.000000000000000000, 0.8660254037844387076, 1.000000000000000000, 0.8660254037844387076, 1.000000000000000000, 0.8660254037844387076, 1.000000000000000000, 0.8660254037844387076, 1.000000000000000000),
 ( 1.000000000000000000, 0.8660254037844387076, 1.000000000000000000, 0.8660254037844387076, 1.000000000000000000, 0.8660254037844387076, 1.000000000000000000, 0.8660254037844387076, 1.000000000000000000, 0.8660254037844387076, 1.000000000000000000, 0.8660254037844387076, 1.000000000000000000, 0.8660254037844387076, 1.000000000000000000, 0.8660254037844387076, 1.000000000000000000, 0.8660254037844387076, 1.000000000000000000, 0.8660254037844387076, 1.000000000000000000, 0.8660254037844387076, 1.000000000000000000, 0.8660254037844387076, 1.000000000000000000, 0.8660254037844387076, 1.000000000000000000, 0.8660254037844387076, 1.000000000000000000, 0.8660254037844387076, 1.000000000000000000, 0.8660254037844387076, 1.000000000000000000, 0.8660254037844387076, 1.000000000000000000, 0.8660254037844387076, 1.000000000000000000, 0.8660254037844387076, 1.000000000000000000, 0.8660254037844387076, 1.000000000000000000, 0.8660254037844387076, 1.000000000000000000, 0.8660254037844387076, 1.000000000000000000, 0.8660254037844387076, 1.000000000000000000, 0.8660254037844387076, 1.000000000000000000, 0.8660254037844387076, 1.000000000000000000, 0.8660254037844387076, 1.000000000000000000, 0.8660254037844387076, 1.000000000000000000, 0.8660254037844387076, 1.000000000000000000, 0.8660254037844387076, 1.000000000000000000, 0.8660254037844387076, 1.000000000000000000, 0.8660254037844387076, 1.000000000000000000, 0.8660254037844387076, 1.000000000000000000, 0.8660254037844387076, 1.000000000000000000, 0.8660254037844387076, 1.000000000000000000, 0.8660254037844387076, 1.000000000000000000, 0.8660254037844387076, 1.000000000000000000, 0.8660254037844387076, 1.000000000000000000, 0.8660254037844387076, 1.000000000000000000, 0.8660254037844387076, 1.000000000000000000, 0.8660254037844387076, 1.000000000000000000, 0.8660254037844387076, 1.000000000000000000, 0.8660254037844387076, 1.000000000000000000, 0.8660254037844387076, 1.000000000000000000, 0.8660254037844387076, 1.000000000000000000, 0.8660254037844387076, 1.000000000000000000, 0.8660254037844387076, 1.000000000000000000, 0.8660254037844387076, 1.000000000000000000, 0.8660254037844387076, 1.000000000000000000, 0.8660254037844387076, 1.000000000000000000, 0.8660254037844387076, 1.000000000000000000, 0.8660254037844387076, 1.000000000000000000, 0.8660254037844387076, 1.000000000000000000, 0.8660254037844387076, 1.000000000000000000, 0.8660254037844387076, 1.000000000000000000, 0.8660254037844387076, 1.000000000000000000, 0.8660254037844387076, 1.000000000000000000, 0.8660254037844387076, 1.000000000000000000, 0.8660254037844387076, 1.000000000000000000, 0.8660254037844387076, 1.000000000000000000, 0.8660254037844387076, 1.000000000000000000, 0.8660254037844387076, 1.000000000000000000, 0.8660254037844387076, 1.000000000000000000, 0.8660254037844387076, 1.000000000000000000, 0.8660254037844387076, 1.000000000000000000, 0.8660254037844387076, 1.000000000000000000, 0.8660254037844387076, 1.000000000000000000, 0.8660254037844387076, 1.000000000000000000, 0.8660254037844387076, 1.000000000000000000, 0.8660254037844387076, 1.000000000000000000, 0.8660254037844387076, 1.000000000000000000, 0.8660254037844387076, 1.000000000000000000, 0.8660254037844387076, 1.000000000000000000, 0.8660254037844387076, 1.000000000000000000, 0.8660254037844387076, 1.000000000000000000, 0.8660254037844387076, 1.000000000000000000, 0.8660254037844387076, 1.000000000000000000, 0.8660254037844387076, 1.000000000000000000, 0.8660254037844387076, 1.000000000000000000, 0.8660254037844387076, 1.000000000000000000, 0.8660254037844387076, 1.000000000000000000, 0.8660254037844387076, 1.000000000000000000, 0.8660254037844387076, 1.000000000000000000, 0.8660254037844387076, 1.000000000000000000, 0.8660254037844387076, 1.000000000000000000, 0.8660254037844387076, 1.000000000000000000, 0.8660254037844387076, 1.000000000000000000, 0.8660254037844387076, 1.000000000000000000, 0.8660254037844387076, 1.000000000000000000, 0.8660254037844387076, 1.000000000000000000, 0.8660254037844387076, 1.000000000000000000, 0.8660254037844387076, 1.000000000000000000, 0.8660254037844387076, 1.000000000000000000, 0.8660254037844387076, 1.000000000000000000, 0.8660254037844387076, 1.000000000000000000, 0.8660254037844387076, 1.000000000000000000, 0.8660254037844387076, 1.000000000000000000, 0.8660254037844387076, 1.000000000000000000, 0.8660254037844387076, 1.000000000000000000, 0.8660254037844387076, 1.000000000000000000, 0.8660254037844387076, 1.000000000000000000, 0.8660254037844387076, 1.000000000000000000, 0.8660254037844387076, 1.000000000000000000, 0.8660254037844387076, 1.000000000000000000, 0.8660254037844387076, 1.000000000000000000, 0.8660254037844387076, 1.000000000000000000, 0.8660254037844387076, 1.000000000000000000, 0.8660254037844387076, 1.000000000000000000, 0.8660254037844387076, 1.000000000000000000, 0.8660254037844387076, 1.000000000000000000, 0.8660254037844387076, 1.000000000000000000, 0.8660254037844387076, 1.000000000000000000, 0.8660254037844387076, 1.000000000000000000, 0.8660254037844387076, 1.000000000000000000, 0.8660254037844387076, 1.000000000000000000, 0.8660254037844387076, 1.000000000000000000, 0.8660254037844387076, 1.000000000000000000, 0.8660254037844387076, 1.000000000000000000, 0.8660254037844387076, 1.000000000000000000, 0.8660254037844387076, 1.000000000000000000, 0.8660254037844387076, 1.000000000000000000, 0.8660254037844387076, 1.000000000000000000, 0.8660254037844387076, 1.000000000000000000, 0.8660254037844387076, 1.000000000000000000, 0.8660254037844387076, 1.000000000000000000, 0.8660254037844387076, 1.000000000000000000, 0.8660254037844387076, 1.000000000000000000, 0.8660254037844387076, 1.000000000000000000, 0.8660254037844387076, 1.000000000000000000, 0.8660254037844387076, 1.000000000000000000, 0.8660254037844387076, 1.000000000000000000, 0.8660254037844387076, 1.000000000000000000, 0.8660254037844387076, 1.000000000000000000, 0.8660254037844387076, 1.000000000000000000, 0.8660254037844387076, 1.000000000000000000, 0.8660254037844387076, 1.000000000000000000, 0.8660254037844387076, 1.000000000000000000, 0.8660254037844387076, 1.000000000000000000, 0.8660254037844387076, 1.000000000000000000, 0.8660254037844387076, 1.000000000000000000, 0.8660254037844387076, 1.000000000000000000, 0.8660254037844387076, 1.000000000000000000, 0.8660254037844387076, 1.000000000000000000, 0.8660254037844387076, 1.000000000000000000, 0.8660254037844387076, 1.000000000000000000, 0.8660254037844387076, 1.000000000000000000, 0.8660254037844387076, 1.000000000000000000, 0.8660254037844387076, 1.000000000000000000, 0.8660254037844387076, 1.000000000000000000, 0.8660254037844387076, 1.000000000000000000, 0.8660254037844387076, 1.000000000000000000, 0.8660254037844387076, 1.000000000000000000, 0.8660254037844387076, 1.000000000000000000, 0.8660254037844387076, 1.000000000000000000, 0.8660254037844387076, 1.000000000000000000, 0.8660254037844387076, 1.000000000000000000, 0.8660254037844387076, 1.000000000000000000, 0.8660254037844387076, 1.000000000000000000, 0.8660254037844387076, 1.000000000000000000, 0.8660254037844387076, 1.000000000000000000, 0.8660254037844387076, 1.000000000000000000, 0.8660254037844387076, 1.000000000000000000, 0.8660254037844387076, 1.000000000000000000, 0.8660254037844387076, 1.000000000000000000, 0.8660254037844387076, 1.000000000000000000, 0.8660254037844387076, 1.000000000000000000, 0.8660254037844387076, 1.000000000000000000, 0.8660254037844387076, 1.000000000000000000, 0.8660254037844387076, 1.000000000000000000, 0.8660254037844387076, 1.000000000000000000, 0.8660254037844387076, 1.000000000000000000, 0.8660254037844387076, 1.000000000000000000, 0.8660254037844387076, 1.000000000000000000, 0.8660254037844387076, 1.000000000000000000, 0.8660254037844387076, 1.000000000000000000, 0.8660254037844387076, 1.000000000000000000, 0.8660254037844387076, 1.000000000000000000, 0.8660254037844387076, 1.000000000000000000, 0.8660254037844387076, 1.000000000000000000, 0.8660254037844387076, 1.000000000000000000, 0.8660254037844387076, 1.000000000000000000, 0.8660254037844387076, 1.000000000000000000, 0.8660254037844387076, 1.000000000000000000, 0.8660254037844387076, 1.000000000000000000, 0.8660254037844387076, 1.000000000000000000, 0.8660254037844387076, 1.000000000000000000, 0.8660254037844387076, 1.000000000000000000, 0.8660254037844387076, 1.000000000000000000, 0.8660254037844387076, 1.000000000000000000, 0.8660254037844387076, 1.000000000000000000, 0.8660254037844387076, 1.000000000000000000, 0.8660254037844387076, 1.000000000000000000, 0.8660254037844387076, 1.000000000000000000, 0.8660254037844387076, 1.000000000000000000, 0.8660254037844387076, 1.000000000000000000, 0.8660254037844387076, 1.000000000000000000, 0.8660254037844387076, 1.000000000000000000, 0.8660254037844387076, 1.000000000000000000, 0.8660254037844387076, 1.000000000000000000, 0.8660254037844387076, 1.000000000000000000, 0.8660254037844387076, 1.000000000000000000, 0.8660254037844387076, 1.000000000000000000, 0.8660254037844387076, 1.000000000000000000, 0.8660254037844387076, 1.000000000000000000, 0.8660254037844387076, 1.000000000000000000, 0.8660254037844387076, 1.000000000000000000, 0.8660254037844387076, 1.000000000000000000, 0.8660254037844387076, 1.000000000000000000, 0.8660254037844387076, 1.000000000000000000, 0.8660254037844387076, 1.000000000000000000, 0.8660254037844387076, 1.000000000000000000, 0.8660254037844387076, 1.000000000000000000, 0.8660254037844387076, 1.000000000000000000, 0.8660254037844387076, 1.000000000000000000, 0.8660254037844387076, 1.000000000000000000, 0.8660254037844387076, 1.000000000000000000, 0.8660254037844387076, 1.000000000000000000, 0.8660254037844387076, 1.000000000000000000, 0.8660254037844387076, 1.000000000000000000, 0.8660254037844387076, 1.000000000000000000, 0.8660254037844387076, 1.000000000000000000, 0.8660254037844387076, 1.000000000000000000, 0.8660254037844387076, 1.000000000000000000, 0.8660254037844387076, 1.000000000000000000, 0.8660254037844387076, 1.000000000000000000, 0.8660254037844387076, 1.000000000000000000, 0.8660254037844387076, 1.000000000000000000, 0.8660254037844387076, 1.000000000000000000, 0.8660254037844387076, 1.000000000000000000, 0.8660254037844387076, 1.000000000000000000, 0.8660254037844387076, 1.000000000000000000, 0.8660254037844387076, 1.000000000000000000, 0.8660254037844387076, 1.000000000000000000, 0.8660254037844387076, 1.000000000000000000, 0.8660254037844387076, 1.000000000000000000, 0.8660254037844387076, 1.000000000000000000, 0.8660254037844387076, 1.000000000000000000, 0.8660254037844387076, 1.000000000000000000, 0.8660254037844387076, 1.000000000000000000, 0.8660254037844387076, 1.000000000000000000, 0.8660254037844387076, 1.000000000000000000, 0.8660254037844387076, 1.000000000000000000, 0.8660254037844387076, 1.000000000000000000, 0.8660254037844387076, 1.000000000000000000, 0.8660254037844387076, 1.000000000000000000, 0.8660254037844387076, 1.000000000000000000, 0.8660254037844387076, 1.000000000000000000, 0.8660254037844387076, 1.000000000000000000, 0.8660254037844387076, 1.000000000000000000, 0.8660254037844387076, 1.000000000000000000, 0.8660254037844387076, 1.000000000000000000, 0.8660254037844387076, 1.000000000000000000, 0.8660254037844387076, 1.000000000000000000, 0.8660254037844387076, 1.000000000000000000, 0.8660254037844387076, 1.000000000000000000, 0.8660254037844387076, 1.000000000000000000, 0.8660254037844387076, 1.000000000000000000, 0.8660254037844387076, 1.000000000000000000, 0.8660254037844387076, 1.000000000000000000, 0.8660254037844387076, 1.000000000000000000, 0.8660254037844387076, 1.000000000000000000, 0.8660254037844387076, 1.000000000000000000, 0.8660254037844387076, 1.000000000000000000, 0.8660254037844387076, 1.000000000000000000, 0.8660254037844387076, 1.000000000000000000, 0.8660254037844387076, 1.000000000000000000, 0.8660254037844387076, 1.000000000000000000, 0.8660254037844387076, 1.000000000000000000, 0.8660254037844387076, 1.000000000000000000, 0.8660254037844387076, 1.000000000000000000, 0.8660254037844387076, 1.000000000000000000, 0.8660254037844387076, 1.000000000000000000, 0.8660254037844387076, 1.000000000000000000, 0.8660254037844387076, 1.000000000000000000, 0.8660254037844387076, 1.000000000000000000, 0.8660254037844387076, 1.000000000000000000, 0.8660254037844387076, 1.000000000000000000, 0.8660254037844387076, 1.000000000000000000, 0.8660254037844387076, 1.000000000000000000, 0.8660254037844387076, 1.000000000000000000, 0.8660254037844387076, 1.000000000000000000, 0.8660254037844387076, 1.000000000000000000, 0.8660254037844387076, 1.000000000000000000, 0.8660254037844387076, 1.000000000000000000, 0.8660254037844387076, 1.000000000000000000, 0.8660254037844387076, 1.000000000000000000, 0.8660254037844387076, 1.000000000000000000, 0.8660254037844387076, 1.000000000000000000, 0.8660254037844387076, 1.000000000000000000, 0.8660254037844387076, 1.000000000000000000, 0.8660254037844387076, 1.000000000000000000, 0.8660254037844387076, 1.000000000000000000, 0.8660254037844387076, 1.000000000000000000, 0.8660254037844387076, 1.000000000000000000, 0.8660254037844387076, 1.000000000000000000, 0.8660254037844387076, 1.000000000000000000, 0.8660254037844387076, 1.000000000000000000, 0.8660254037844387076, 1.000000000000000000, 0.8660254037844387076, 1.000000000000000000, 0.8660254037844387076, 1.000000000000000000, 0.8660254037844387076, 1.000000000000000000, 0.8660254037844387076, 1.000000000000000000, 0.8660254037844387076, 1.000000000000000000, 0.8660254037844387076, 1.000000000000000000, 0.8660254037844387076, 1.000000000000000000, 0.8660254037844387076, 1.000000000000000000, 0.8660254037844387076, 1.000000000000000000, 0.8660254037844387076, 1.000000000000000000, 0.8660254037844387076, 1.000000000000000000, 0.8660254037844387076, 1.000000000000000000, 0.8660254037844387076, 1.000000000000000000, 0.8660254037844387076, 1.000000000000000000, 0.8660254037844387076, 1.000000000000000000, 0.8660254037844387076, 1.000000000000000000, 0.8660254037844387076, 1.000000000000000000, 0.8660254037844387076, 1.000000000000000000, 0.8660254037844387076, 1.000000000000000000, 0.8660254037844387076, 1.000000000000000000, 0.8660254037844387076, 1.000000000000000000, 0.8660254037844387076, 1.000000000000000000, 0.8660254037844387076, 1.000000000000000000, 0.8660254037844387076, 1.000000000000000000, 0.8660254037844387076, 1.000000000000000000, 0.8660254037844387076, 1.000000000000000000, 0.8660254037844387076, 1.000000000000000000, 0.8660254037844387076, 1.000000000000000000, 0.8660254037844387076, 1.000000000000000000, 0.8660254037844387076, 1.000000000000000000, 0.8660254037844387076, 1.000000000000000000, 0.8660254037844387076, 1.000000000000000000, 0.8660254037844387076, 1.000000000000000000, 0.8660254037844387076, 1.000000000000000000, 0.8660254037844387076, 1.000000000000000000, 0.8660254037844387076, 1.000000000000000000, 0.8660254037844387076, 1.000000000000000000, 0.8660254037844387076, 1.000000000000000000, 0.8660254037844387076, 1.000000000000000000, 0.8660254037844387076, 1.000000000000000000, 0.8660254037844387076, 1.000000000000000000, 0.8660254037844387076, 1.000000000000000000, 0.8660254037844387076, 1.000000000000000000, 0.8660254037844387076, 1.000000000000000000, 0.8660254037844387076, 1.000000000000000000, 0.8660254037844387076, 1.000000000000000000, 0.8660254037844387076, 1.000000000000000000, 0.8660254037844387076, 1.000000000000000000, 0.8660254037844387076, 1.000000000000000000, 0.8660254037844387076, 1.000000000000000000, 0.8660254037844387076, 1.000000000000000000, 0.8660254037844387076, 1.000000000000000000, 0.8660254037844387076, 1.000000000000000000, 0.8660254037844387076, 1.000000000000000000, 0.8660254037844387076, 1.000000000000000000, 0.8660254037844387076, 1.000000000000000000, 0.8660254037844387076, 1.000000000000000000, 0.8660254037844387076, 1.000000000000000000, 0.8660254037844387076, 1.000000000000000000, 0.8660254037844387076, 1.000000000000000000, 0.8660254037844387076, 1.000000000000000000, 0.8660254037844387076, 1.000000000000000000, 0.8660254037844387076, 1.000000000000000000) ) ) 
 REPRESENTATION_ITEM ( '' )  SURFACE ( )  );
#35891 = CARTESIAN_POINT ( 'NONE',  ( 26.66250000122903430, -4.330127018922190985, -2.500000000000001332 ) ) ;
#35892 = CARTESIAN_POINT ( 'NONE',  ( 19.73437500061451644, 5.824947211148865298E-16, -4.756430356249998326 ) ) ;
#35893 = CARTESIAN_POINT ( 'NONE',  ( 17.20312500061451644, 0.000000000000000000, 5.243569643749999010 ) ) ;
#35894 = CARTESIAN_POINT ( 'NONE',  ( 8.062500000000000000, -5.773502691896255534, -1.060575238724906372E-15 ) ) ;
#35895 = CARTESIAN_POINT ( 'NONE',  ( 28.32187500061451502, 3.027376345333613106, -5.243569643749998122 ) ) ;
#35896 = CARTESIAN_POINT ( 'NONE',  ( 9.909375000614517148, 4.541064518000418104, -2.621784821874998173 ) ) ;
#35897 = CARTESIAN_POINT ( 'NONE',  ( 8.446875000614518569, -3.027376345333610441, -5.243569643749999898 ) ) ;
#35898 = CARTESIAN_POINT ( 'NONE',  ( 17.40937500061451715, -4.541064518000417216, -2.621784821875001281 ) ) ;
#35899 = ORIENTED_EDGE ( 'NONE', *, *, #34668, .T. ) ;
#35900 = CARTESIAN_POINT ( 'NONE',  ( 24.18750000122903288, 4.330127018922191873, 2.499999999999999556 ) ) ;
#35901 = CARTESIAN_POINT ( 'NONE',  ( 20.57812500061451644, 6.421520780324663323E-16, -5.243569643749999010 ) ) ;
#35902 = CARTESIAN_POINT ( 'NONE',  ( 17.33437500061451431, -4.541064518000419881, 2.621784821874995952 ) ) ;
#35903 = CARTESIAN_POINT ( 'NONE',  ( 22.22812500061451502, -4.541064518000419881, 2.621784821874995952 ) ) ;
#35904 = CARTESIAN_POINT ( 'NONE',  ( 4.000000000000000000, 13.43750000000000000, 32.30940107675849049 ) ) ;
#35905 = VECTOR ( 'NONE', #54404, 1000.000000000000000 ) ;
#35906 = CARTESIAN_POINT ( 'NONE',  ( 28.75312500061451715, 4.541064518000418104, -2.621784821874998173 ) ) ;
#35907 = CARTESIAN_POINT ( 'NONE',  ( 10.50000000122903465, -2.886751345948125991, -5.000000000000000000 ) ) ;
#35908 = ORIENTED_EDGE ( 'NONE', *, *, #12056, .F. ) ;
#35909 = CARTESIAN_POINT ( 'NONE',  ( 4.537500001229034297, -4.330127018922194537, 2.499999999999995559 ) ) ;
#35910 = CARTESIAN_POINT ( 'NONE',  ( -3.999999999999999556, 17.26249999999999929, -32.30940107675850470 ) ) ;
#35911 = CARTESIAN_POINT ( 'NONE',  ( 24.11250000122903359, 4.330127018922192761, -2.499999999999997780 ) ) ;
#35912 = CARTESIAN_POINT ( 'NONE',  ( 4.000000000000000000, 20.09374999877096712, 30.00000000000000000 ) ) ;
#35913 = CARTESIAN_POINT ( 'NONE',  ( 9.159375000614515372, 0.000000000000000000, 5.243569643749999010 ) ) ;
#35914 = CARTESIAN_POINT ( 'NONE',  ( 10.14375000122903181, 5.773502691896255534, 3.535250795749688401E-16 ) ) ;
#35915 = CARTESIAN_POINT ( 'NONE',  ( 14.39062500061451821, 6.054752690667223547, 3.707466751127219781E-16 ) ) ;
#35916 = CARTESIAN_POINT ( 'NONE',  ( 11.40937500061451892, 0.000000000000000000, 5.243569643749999010 ) ) ;
#35917 = CARTESIAN_POINT ( 'NONE',  ( 28.68750000122903288, 4.330127018922191873, 2.499999999999999556 ) ) ;
#35918 = VECTOR ( 'NONE', #47134, 1000.000000000000000 ) ;
#35919 = CARTESIAN_POINT ( 'NONE',  ( 18.53437500061451715, 4.541064518000418104, 2.621784821874999949 ) ) ;
#35920 = CARTESIAN_POINT ( 'NONE',  ( 6.609375000614519102, -4.541064518000417216, -2.621784821875001281 ) ) ;
#35921 = CARTESIAN_POINT ( 'NONE',  ( 7.320879633048903241E-15, 17.63749999999999218, -34.00000000000000000 ) ) ;
#35922 = CARTESIAN_POINT ( 'NONE',  ( 6.965625000614518392, -6.054752690667223547, -1.112240025338166033E-15 ) ) ;
#35923 = CARTESIAN_POINT ( 'NONE',  ( 16.82812500061451644, -4.541064518000419881, 2.621784821874995952 ) ) ;
#35924 =( BOUNDED_CURVE ( )  B_SPLINE_CURVE ( 2, ( #30919, #64166, #35733, #58253, #30198, #25380, #1773 ),
 .UNSPECIFIED., .F., .F. ) 
 B_SPLINE_CURVE_WITH_KNOTS ( ( 3, 2, 2, 3 ),
 ( 0.9900000000000002132, 0.9933333333333334014, 0.9966666666666668117, 1.000000000000000000 ),
 .UNSPECIFIED. ) 
 CURVE ( )  GEOMETRIC_REPRESENTATION_ITEM ( )  RATIONAL_B_SPLINE_CURVE ( ( 0.9999999999999911182, 0.8660254037844475894, 1.000000000000000000, 0.8660254037844387076, 1.000000000000000000, 0.8660254037844387076, 1.000000000000000000 ) ) 
 REPRESENTATION_ITEM ( '' )  );
#35925 = VERTEX_POINT ( 'NONE', #2249 ) ;
#35926 = CARTESIAN_POINT ( 'NONE',  ( 15.85312500061451857, 0.000000000000000000, 5.243569643749999010 ) ) ;
#35927 = VECTOR ( 'NONE', #29236, 1000.000000000000000 ) ;
#35928 = CARTESIAN_POINT ( 'NONE',  ( 11.39062500061451644, -3.027376345333614438, 5.243569643749998122 ) ) ;
#35929 = CARTESIAN_POINT ( 'NONE',  ( 23.40937500061451715, 4.119189519843966529, -2.378215178124998275 ) ) ;
#35930 = CARTESIAN_POINT ( 'NONE',  ( 10.68750000000000000, -2.886751345948129988, 4.999999999999997335 ) ) ;
#35931 = CARTESIAN_POINT ( 'NONE',  ( 7.387500001229032165, 6.123233995736764310E-16, -4.999999999999998224 ) ) ;
#35932 = CARTESIAN_POINT ( 'NONE',  ( 14.48437500061451821, 4.541064518000418104, 2.621784821874999949 ) ) ;
#35933 = CARTESIAN_POINT ( 'NONE',  ( 15.82500000122903216, -5.773502691896255534, -1.060575238724906372E-15 ) ) ;
#35934 = CARTESIAN_POINT ( 'NONE',  ( 25.34999999999999787, 4.330127018922192761, -2.499999999999997780 ) ) ;
#35935 =( BOUNDED_CURVE ( )  B_SPLINE_CURVE ( 2, ( #6041, #10855, #11944, #55925, #61821, #66651, #50027, #16028, #11226 ),
 .UNSPECIFIED., .F., .F. ) 
 B_SPLINE_CURVE_WITH_KNOTS ( ( 3, 2, 2, 2, 3 ),
 ( 0.4891304347826087029, 0.4927536231884058204, 0.5000000000000000000, 0.5072463768115942351, 0.5108695652173913526 ),
 .UNSPECIFIED. ) 
 CURVE ( )  GEOMETRIC_REPRESENTATION_ITEM ( )  RATIONAL_B_SPLINE_CURVE ( ( 0.9330127018922194093, 0.9330127018922194093, 1.000000000000000000, 0.8660254037844387076, 1.000000000000000000, 0.8660254037844387076, 1.000000000000000000, 0.9330127018922182991, 0.9330127018922192983 ) ) 
 REPRESENTATION_ITEM ( '' )  );
#35936 = CARTESIAN_POINT ( 'NONE',  ( -2.121784821874999949, 18.37812500061451715, -33.67503911421598417 ) ) ;
#35937 = CARTESIAN_POINT ( 'NONE',  ( 16.27500000122903501, -5.773502691896255534, -1.060575238724906372E-15 ) ) ;
#35938 = DIRECTION ( 'NONE',  ( -1.000000000000000000, -0.000000000000000000, -0.000000000000000000 ) ) ;
#35939 = DIRECTION ( 'NONE',  ( -1.000000000000000000, -0.000000000000000000, -0.000000000000000000 ) ) ;
#35940 = CARTESIAN_POINT ( 'NONE',  ( 3.387317645811362521, -3.677893962807537775, 3.685928698369520973 ) ) ;
#35941 = CARTESIAN_POINT ( 'NONE',  ( 4.633613603196540254, 1.878729617659674167, 4.895446622381335544 ) ) ;
#35942 = CARTESIAN_POINT ( 'NONE',  ( 18.72187500061451360, -6.054752690667223547, -1.112240025338166033E-15 ) ) ;
#35943 = CARTESIAN_POINT ( 'NONE',  ( 29.39999999999999858, 4.330127018922192761, -2.499999999999997780 ) ) ;
#35944 = EDGE_CURVE ( 'NONE', #46701, #33889, #1715, .T. ) ;
#35945 = CARTESIAN_POINT ( 'NONE',  ( 13.15312500061451750, 0.000000000000000000, 5.243569643749999010 ) ) ;
#35946 = CARTESIAN_POINT ( 'NONE',  ( 10.21875000122903288, 2.886751345948126879, 4.999999999999999112 ) ) ;
#35947 = CARTESIAN_POINT ( 'NONE',  ( 24.08437500061451786, -4.541064518000419881, 2.621784821874995952 ) ) ;
#35948 = CARTESIAN_POINT ( 'NONE',  ( 16.54687500061451644, 4.119189519843966529, -2.378215178124998275 ) ) ;
#35949 = VECTOR ( 'NONE', #40500, 1000.000000000000000 ) ;
#35950 = CARTESIAN_POINT ( 'NONE',  ( 9.178125000614517859, -4.541064518000419881, 2.621784821874995952 ) ) ;
#35951 = CARTESIAN_POINT ( 'NONE',  ( 14.70937500061451786, -4.541064518000417216, -2.621784821875001281 ) ) ;
#35952 = ORIENTED_EDGE ( 'NONE', *, *, #16469, .T. ) ;
#35953 = CARTESIAN_POINT ( 'NONE',  ( 25.50937500061451502, -4.541064518000417216, -2.621784821875001281 ) ) ;
#35954 = CARTESIAN_POINT ( 'NONE',  ( 28.26562500061451289, 3.027376345333613106, -5.243569643749998122 ) ) ;
#35955 = CARTESIAN_POINT ( 'NONE',  ( 18.10312500061451502, 0.000000000000000000, 5.243569643749999010 ) ) ;
#35956 = CARTESIAN_POINT ( 'NONE',  ( 4.898587196589411843E-16, 20.00000000000000000, 33.99999999999999289 ) ) ;
#35957 = DIRECTION ( 'NONE',  ( -0.000000000000000000, -1.000000000000000000, 8.673617379884035472E-17 ) ) ;
#35958 = VECTOR ( 'NONE', #17439, 1000.000000000000000 ) ;
#35959 = CARTESIAN_POINT ( 'NONE',  ( 10.80000000000000071, -4.330127018922190985, -2.500000000000001332 ) ) ;
#35960 = CARTESIAN_POINT ( 'NONE',  ( 18.97500000122903074, -5.773502691896255534, -1.060575238724906372E-15 ) ) ;
#35961 = CARTESIAN_POINT ( 'NONE',  ( 10.48125000122903216, 6.123233995736764310E-16, -4.999999999999998224 ) ) ;
#35962 = CARTESIAN_POINT ( 'NONE',  ( 9.309375000614515727, 2.746126346562645981, -4.756430356249997438 ) ) ;
#35963 = VERTEX_POINT ( 'NONE', #42865 ) ;
#35964 = CARTESIAN_POINT ( 'NONE',  ( 17.73750000000000071, 5.773502691896255534, 3.535250795749688894E-16 ) ) ;
#35965 = CARTESIAN_POINT ( 'NONE',  ( 21.86250000000000071, 2.886751345948126879, 4.999999999999999112 ) ) ;
#35966 = CARTESIAN_POINT ( 'NONE',  ( 17.93437500061451928, 6.421520780324663323E-16, -5.243569643749999010 ) ) ;
#35967 = CARTESIAN_POINT ( 'NONE',  ( 13.15312500061451750, 0.000000000000000000, 5.243569643749999010 ) ) ;
#35969 = ORIENTED_EDGE ( 'NONE', *, *, #35460, .T. ) ;
#35968 = AXIS2_PLACEMENT_3D ( 'NONE', #44714, #66881, #67250 ) ;
#35970 = CARTESIAN_POINT ( 'NONE',  ( 1.071796769724489895, 18.62990381179669797, -34.00000000000000000 ) ) ;
#35971 = CARTESIAN_POINT ( 'NONE',  ( 5.503125000614516260, 0.000000000000000000, 5.243569643749999010 ) ) ;
#35972 = CARTESIAN_POINT ( 'NONE',  ( 8.906250001229031099, 0.000000000000000000, 4.999999999999998224 ) ) ;
#35973 = CARTESIAN_POINT ( 'NONE',  ( 13.04999999999999893, -4.330127018922190985, -2.500000000000001332 ) ) ;
#35974 = CARTESIAN_POINT ( 'NONE',  ( 28.02187500061451431, -4.119189519843968306, 2.378215178124996054 ) ) ;
#35975 = CARTESIAN_POINT ( 'NONE',  ( 9.001249775931846008E-16, 16.31562500061451715, 34.90005215228797653 ) ) ;
#35976 = CARTESIAN_POINT ( 'NONE',  ( 29.39062500061451289, -3.027376345333614438, 5.243569643749998122 ) ) ;
#35977 = CARTESIAN_POINT ( 'NONE',  ( 8.175000000000002487, 6.123233995736764310E-16, -4.999999999999998224 ) ) ;
#35978 = AXIS2_PLACEMENT_3D ( 'NONE', #31968, #70758, #20133 ) ;
#35979 = CARTESIAN_POINT ( 'NONE',  ( -1.878215178125001827, 16.99062499938548498, 33.25316411605952283 ) ) ;
#35980 = CARTESIAN_POINT ( 'NONE',  ( 23.52187500061451786, 3.027376345333611329, 5.243569643749999010 ) ) ;
#35981 = ORIENTED_EDGE ( 'NONE', *, *, #54670, .F. ) ;
#35982 = CARTESIAN_POINT ( 'NONE',  ( 21.47812500061451502, 6.421520780324663323E-16, -5.243569643749999010 ) ) ;
#35983 = CARTESIAN_POINT ( 'NONE',  ( 22.80937500061451573, -4.541064518000417216, -2.621784821875001281 ) ) ;
#35984 = CARTESIAN_POINT ( 'NONE',  ( -3.000416591977282496E-16, 16.54062500061459673, -34.90005215228797653 ) ) ;
#35985 = CARTESIAN_POINT ( 'NONE',  ( 7.303125000614516082, 0.000000000000000000, 5.243569643749999010 ) ) ;
#35986 = CARTESIAN_POINT ( 'NONE',  ( 27.42187500061451644, 2.746126346562645981, -4.756430356249997438 ) ) ;
#35987 = CARTESIAN_POINT ( 'NONE',  ( 24.51562500061451289, -6.054752690667223547, -1.112240025338166033E-15 ) ) ;
#35988 = CARTESIAN_POINT ( 'NONE',  ( 27.57187500061451502, -4.119189519843968306, 2.378215178124996054 ) ) ;
#35989 = CARTESIAN_POINT ( 'NONE',  ( 10.28437500061451715, 5.824947211148865298E-16, -4.756430356249998326 ) ) ;
#35990 = CARTESIAN_POINT ( 'NONE',  ( 15.79687500061451821, 6.054752690667223547, 3.707466751127219781E-16 ) ) ;
#35991 = CARTESIAN_POINT ( 'NONE',  ( 23.67187500061451999, -6.054752690667223547, -1.112240025338166033E-15 ) ) ;
#35992 = CARTESIAN_POINT ( 'NONE',  ( 2.121784821875001281, 14.60937500061451821, 33.67503911421598417 ) ) ;
#35993 = CARTESIAN_POINT ( 'NONE',  ( 8.128125000614515372, 4.541064518000418104, 2.621784821874999949 ) ) ;
#35994 = CARTESIAN_POINT ( 'NONE',  ( 45.00000000000000000, 6.123233995736764310E-16, -4.999999999999998224 ) ) ;
#35995 = CARTESIAN_POINT ( 'NONE',  ( 28.60312500061451502, -4.541064518000417216, -2.621784821875001281 ) ) ;
#35996 = CARTESIAN_POINT ( 'NONE',  ( 0.000000000000000000, 20.00000000000000000, 30.00000000000000000 ) ) ;
#35997 = CARTESIAN_POINT ( 'NONE',  ( 5.315625000614516260, 3.027376345333613106, -5.243569643749998122 ) ) ;
#35998 = CARTESIAN_POINT ( 'NONE',  ( 8.559375000614515727, 4.541064518000418104, -2.621784821874998173 ) ) ;
#35999 = CARTESIAN_POINT ( 'NONE',  ( 16.61250000122903359, 0.000000000000000000, 4.999999999999998224 ) ) ;
#36000 = CARTESIAN_POINT ( 'NONE',  ( 3.871875000614519280, -6.054752690667223547, -1.112240025338166033E-15 ) ) ;
#36001 = CARTESIAN_POINT ( 'NONE',  ( 6.965625000614518392, -6.054752690667223547, -1.112240025338166033E-15 ) ) ;
#36002 = CARTESIAN_POINT ( 'NONE',  ( 2.828200636599751609E-16, 13.90624999877096535, 25.38119784648299415 ) ) ;
#36003 = CARTESIAN_POINT ( 'NONE',  ( 21.35625000122903216, 4.330127018922192761, -2.499999999999997780 ) ) ;
#36004 = CARTESIAN_POINT ( 'NONE',  ( 17.67187500061451644, 3.027376345333611329, 5.243569643749999010 ) ) ;
#36005 = CARTESIAN_POINT ( 'NONE',  ( 22.72499999999999787, 4.330127018922191873, 2.499999999999999556 ) ) ;
#36006 = ORIENTED_EDGE ( 'NONE', *, *, #51854, .T. ) ;
#36007 = CARTESIAN_POINT ( 'NONE',  ( 21.17812500061451431, 4.541064518000418104, 2.621784821874999949 ) ) ;
#36008 = CARTESIAN_POINT ( 'NONE',  ( 10.34062500061451750, 6.054752690667223547, 3.707466751127219781E-16 ) ) ;
#36009 = EDGE_CURVE ( 'NONE', #1724, #68363, #25503, .T. ) ;
#36010 = CARTESIAN_POINT ( 'NONE',  ( 27.57187500061451857, 3.027376345333611329, 5.243569643749999010 ) ) ;
#36011 = CARTESIAN_POINT ( 'NONE',  ( 9.628125000614517148, -4.541064518000419881, 2.621784821874995952 ) ) ;
#36012 = FACE_OUTER_BOUND ( 'NONE', #1647, .T. ) ;
#36013 = CARTESIAN_POINT ( 'NONE',  ( 9.562500001229032875, -4.330127018922190985, -2.500000000000001332 ) ) ;
#36014 = CARTESIAN_POINT ( 'NONE',  ( 24.10312500061451502, -4.541064518000417216, -2.621784821875001281 ) ) ;
#36015 = CARTESIAN_POINT ( 'NONE',  ( -4.243569643749999898, 9.903125000614517504, -30.00000000000000000 ) ) ;
#36016 = CARTESIAN_POINT ( 'NONE',  ( 13.12500000122903288, -5.773502691896255534, -1.060575238724906372E-15 ) ) ;
#36017 = CARTESIAN_POINT ( 'NONE',  ( 22.41562500061451502, 3.027376345333613106, -5.243569643749998122 ) ) ;
#36018 = VECTOR ( 'NONE', #36901, 1000.000000000000000 ) ;
#36019 = CARTESIAN_POINT ( 'NONE',  ( 18.25312500061451715, -4.541064518000417216, -2.621784821875001281 ) ) ;
#36020 = CARTESIAN_POINT ( 'NONE',  ( 5.146875000614517859, -3.027376345333614438, 5.243569643749998122 ) ) ;
#36021 = CARTESIAN_POINT ( 'NONE',  ( 18.37500000000000355, -4.330127018922194537, 2.499999999999995559 ) ) ;
#36022 = CARTESIAN_POINT ( 'NONE',  ( 12.97500000122903252, 2.886751345948126879, 4.999999999999999112 ) ) ;
#36023 = VECTOR ( 'NONE', #57605, 1000.000000000000000 ) ;
#36024 = CARTESIAN_POINT ( 'NONE',  ( 11.54062500061451857, -3.027376345333610441, -5.243569643749999898 ) ) ;
#36025 = CARTESIAN_POINT ( 'NONE',  ( 13.67812500061451786, -4.541064518000419881, 2.621784821874995952 ) ) ;
#36026 = AXIS2_PLACEMENT_3D ( 'NONE', #6641, #22879, #45437 ) ;
#36027 = CARTESIAN_POINT ( 'NONE',  ( 26.02500000122903145, 2.886751345948126879, 4.999999999999999112 ) ) ;
#36028 = AXIS2_PLACEMENT_3D ( 'NONE', #32270, #54803, #9374 ) ;
#36029 = CARTESIAN_POINT ( 'NONE',  ( 21.64687500061451786, 6.054752690667223547, 3.707466751127219781E-16 ) ) ;
#36030 = CARTESIAN_POINT ( 'NONE',  ( 22.13437500061451502, 4.541064518000418104, 2.621784821874999949 ) ) ;
#36031 = DIRECTION ( 'NONE',  ( -1.000000000000000000, -0.000000000000000000, -0.000000000000000000 ) ) ;
#36032 = CARTESIAN_POINT ( 'NONE',  ( 7.837500001229035007, 6.123233995736764310E-16, -4.999999999999998224 ) ) ;
#36033 = CARTESIAN_POINT ( 'NONE',  ( 7.509375000614517681, -4.541064518000417216, -2.621784821875001281 ) ) ;
#36034 = CARTESIAN_POINT ( 'NONE',  ( 26.14687500061451431, 6.054752690667223547, 3.707466751127219781E-16 ) ) ;
#36035 = CARTESIAN_POINT ( 'NONE',  ( 3.459375000614519635, -4.541064518000417216, -2.621784821875001281 ) ) ;
#36036 = CARTESIAN_POINT ( 'NONE',  ( 21.96562500061451573, 3.027376345333613106, -5.243569643749998122 ) ) ;
#36037 = CARTESIAN_POINT ( 'NONE',  ( 27.15937500061451360, 0.000000000000000000, 5.243569643749999010 ) ) ;
#36038 = CARTESIAN_POINT ( 'NONE',  ( 3.756430356249998770, 16.31562499938548427, 32.16877607737301759 ) ) ;
#36039 = CARTESIAN_POINT ( 'NONE',  ( 19.36875000122903501, -5.773502691896255534, -1.060575238724906372E-15 ) ) ;
#36040 = CARTESIAN_POINT ( 'NONE',  ( 10.96875000122903110, 2.886751345948073588, -5.000000000000094147 ) ) ;
#36041 = CARTESIAN_POINT ( 'NONE',  ( 7.096875000614517148, -3.027376345333610441, -5.243569643749999898 ) ) ;
#36042 = CARTESIAN_POINT ( 'NONE',  ( 17.65312500061451573, 0.000000000000000000, 5.243569643749999010 ) ) ;
#36043 = ORIENTED_EDGE ( 'NONE', *, *, #21308, .T. ) ;
#36044 = CARTESIAN_POINT ( 'NONE',  ( 20.10000000000000142, 0.000000000000000000, 4.999999999999998224 ) ) ;
#36045 = CARTESIAN_POINT ( 'NONE',  ( 27.96562500061451928, 3.027376345333611329, 5.243569643749999010 ) ) ;
#36046 = CARTESIAN_POINT ( 'NONE',  ( 5.221875000614519813, -6.054752690667223547, -1.112240025338166033E-15 ) ) ;
#36047 = CARTESIAN_POINT ( 'NONE',  ( -3.999999999999997335, 15.98750000000000249, -27.69059892324149530 ) ) ;
#36048 = CARTESIAN_POINT ( 'NONE',  ( 0.000000000000000000, 20.00000000000000000, -30.00000000000000000 ) ) ;
#36049 = CARTESIAN_POINT ( 'NONE',  ( 17.36249999999999716, 2.886751345948126879, 4.999999999999999112 ) ) ;
#36050 = CARTESIAN_POINT ( 'NONE',  ( 20.20312500061451644, 4.541064518000418104, -2.621784821874998173 ) ) ;
#36051 = ORIENTED_EDGE ( 'NONE', *, *, #11681, .F. ) ;
#36052 = CARTESIAN_POINT ( 'NONE',  ( 23.85000000000000142, -4.330127018922190985, -2.500000000000001332 ) ) ;
#36053 = EDGE_CURVE ( 'NONE', #51146, #48021, #24473, .T. ) ;
#36054 = CARTESIAN_POINT ( 'NONE',  ( 25.24687500061451573, 6.054752690667223547, 3.707466751127219781E-16 ) ) ;
#36055 = ORIENTED_EDGE ( 'NONE', *, *, #72027, .F. ) ;
#36056 = CARTESIAN_POINT ( 'NONE',  ( 26.62500000000000000, 6.123233995736764310E-16, -4.999999999999998224 ) ) ;
#36057 = CARTESIAN_POINT ( 'NONE',  ( 13.19062500061451537, -3.027376345333614438, 5.243569643749998122 ) ) ;
#36058 = CARTESIAN_POINT ( 'NONE',  ( 6.478125000614516793, -4.541064518000419881, 2.621784821874995952 ) ) ;
#36059 = CARTESIAN_POINT ( 'NONE',  ( 16.88437500061451857, -2.746126346562642428, -4.756430356249999214 ) ) ;
#36060 = CARTESIAN_POINT ( 'NONE',  ( 28.94062500061452070, -3.027376345333614438, 5.243569643749998122 ) ) ;
#36061 = CARTESIAN_POINT ( 'NONE',  ( 14.96250000122903323, -4.330127018922190985, -2.500000000000001332 ) ) ;
#36062 = AXIS2_PLACEMENT_3D ( 'NONE', #24190, #24917, #7213 ) ;
#36063 = CARTESIAN_POINT ( 'NONE',  ( 19.34999999999999787, -4.330127018922190985, -2.500000000000001332 ) ) ;
#36064 = CARTESIAN_POINT ( 'NONE',  ( 27.78749999999999787, -2.886751345948129988, 4.999999999999997335 ) ) ;
#36065 = CARTESIAN_POINT ( 'NONE',  ( 3.121875000614518836, 3.027376345333613106, -5.243569643749998122 ) ) ;
#36066 = CARTESIAN_POINT ( 'NONE',  ( 8.559375000614515727, 4.541064518000418104, -2.621784821874998173 ) ) ;
#36067 = CARTESIAN_POINT ( 'NONE',  ( 19.58437500061451786, -4.541064518000419881, 2.621784821874995952 ) ) ;
#36068 = FACE_OUTER_BOUND ( 'NONE', #54143, .T. ) ;
#36069 = ORIENTED_EDGE ( 'NONE', *, *, #54349, .T. ) ;
#36070 = CARTESIAN_POINT ( 'NONE',  ( 28.94062500061452070, -3.027376345333614438, 5.243569643749998122 ) ) ;
#36071 = CARTESIAN_POINT ( 'NONE',  ( 3.562500000000000444, -5.773502691896255534, -1.060575238724906372E-15 ) ) ;
#36072 = CARTESIAN_POINT ( 'NONE',  ( 5.371875000614516615, 3.027376345333613106, -5.243569643749998122 ) ) ;
#36073 = CARTESIAN_POINT ( 'NONE',  ( 16.05000000000000071, 0.000000000000000000, 4.999999999999998224 ) ) ;
#36074 = CARTESIAN_POINT ( 'NONE',  ( 13.71562500061451750, -6.054752690667223547, -1.112240025338166033E-15 ) ) ;
#36075 = LINE ( 'NONE', #30538, #23012 ) ;
#36076 = CYLINDRICAL_SURFACE ( 'NONE', #3262, 3.999999999999996447 ) ;
#36077 = CARTESIAN_POINT ( 'NONE',  ( 18.48750000122903359, -4.330127018922194537, 2.499999999999995559 ) ) ;
#36078 = CARTESIAN_POINT ( 'NONE',  ( -4.000000000000000000, 19.41874999877096641, 30.00000000000000000 ) ) ;
#36079 = CARTESIAN_POINT ( 'NONE',  ( 18.60937500061451644, 0.000000000000000000, 4.756430356249998326 ) ) ;
#36080 = CARTESIAN_POINT ( 'NONE',  ( 8.803125000614517859, -4.541064518000417216, -2.621784821875001281 ) ) ;
#36081 = CARTESIAN_POINT ( 'NONE',  ( 24.68437500061451573, 6.421520780324663323E-16, -5.243569643749999010 ) ) ;
#36083 = CARTESIAN_POINT ( 'NONE',  ( -4.243569643749999898, 19.85937500061451644, 30.00000000000000000 ) ) ;
#36082 =( BOUNDED_CURVE ( )  B_SPLINE_CURVE ( 2, ( #53183, #31757, #48385, #60175, #42838, #31016, #2580, #71648, #54294 ),
 .UNSPECIFIED., .F., .F. ) 
 B_SPLINE_CURVE_WITH_KNOTS ( ( 3, 2, 2, 2, 3 ),
 ( 0.6250000000000000000, 0.6296296296296296502, 0.6388888888888888395, 0.6481481481481481399, 0.6527777777777777901 ),
 .UNSPECIFIED. ) 
 CURVE ( )  GEOMETRIC_REPRESENTATION_ITEM ( )  RATIONAL_B_SPLINE_CURVE ( ( 0.9330127018922194093, 0.9330127018922194093, 1.000000000000000000, 0.8660254037844387076, 1.000000000000000000, 0.8660254037844387076, 1.000000000000000000, 0.9330127018922194093, 0.9330127018922194093 ) ) 
 REPRESENTATION_ITEM ( '' )  );
#36084 = CARTESIAN_POINT ( 'NONE',  ( 24.90937500061451715, 0.000000000000000000, 5.243569643749999010 ) ) ;
#36085 = CARTESIAN_POINT ( 'NONE',  ( 8.400000000000000355, 0.000000000000000000, 4.999999999999998224 ) ) ;
#36086 = CARTESIAN_POINT ( 'NONE',  ( 4.000000000000000000, 14.00000000122903288, 32.30940107675849049 ) ) ;
#36087 = CARTESIAN_POINT ( 'NONE',  ( 14.09062500061451750, -3.027376345333614438, 5.243569643749998122 ) ) ;
#36088 = CARTESIAN_POINT ( 'NONE',  ( 6.975000001229032520, 2.886751345948129099, -4.999999999999998224 ) ) ;
#36089 = CARTESIAN_POINT ( 'NONE',  ( 10.84687500061451892, 6.054752690667223547, 3.707466751127219781E-16 ) ) ;
#36090 = CARTESIAN_POINT ( 'NONE',  ( 3.869872862876293507, -3.166083388853397906, 4.043238470916601379 ) ) ;
#36091 = VERTEX_POINT ( 'NONE', #13310 ) ;
#36092 = CARTESIAN_POINT ( 'NONE',  ( 13.15312500061451750, 0.000000000000000000, 5.243569643749999010 ) ) ;
#36093 = CARTESIAN_POINT ( 'NONE',  ( 5.810221930991193690E-16, 19.75624999877096499, 26.00000000000000000 ) ) ;
#36094 = CARTESIAN_POINT ( 'NONE',  ( 24.11250000122903359, 4.330127018922192761, -2.499999999999997780 ) ) ;
#36095 = CARTESIAN_POINT ( 'NONE',  ( 11.22187500061451892, 3.027376345333613106, -5.243569643749998122 ) ) ;
#36096 = CARTESIAN_POINT ( 'NONE',  ( 14.57812500061451644, -4.541064518000419881, 2.621784821874995952 ) ) ;
#36097 = CARTESIAN_POINT ( 'NONE',  ( 29.34375000122903288, -2.886751345948125991, -5.000000000000000000 ) ) ;
#36098 = CARTESIAN_POINT ( 'NONE',  ( 22.95937500061451431, 4.541064518000418104, -2.621784821874998173 ) ) ;
#36099 = CARTESIAN_POINT ( 'NONE',  ( 3.999999999999999112, 15.83750000122903501, 30.00000000000000000 ) ) ;
#36100 = CYLINDRICAL_SURFACE ( 'NONE', #43407, 4.999999999999998224 ) ;
#36101 = FACE_OUTER_BOUND ( 'NONE', #55262, .T. ) ;
#36102 = CARTESIAN_POINT ( 'NONE',  ( 9.001249775931846008E-16, 14.12187500061451750, -25.09994784771203058 ) ) ;
#36103 = CARTESIAN_POINT ( 'NONE',  ( 14.67187500061451821, -6.054752690667223547, -1.112240025338166033E-15 ) ) ;
#36104 = CARTESIAN_POINT ( 'NONE',  ( 17.28750000122903430, 6.123233995736764310E-16, -4.999999999999998224 ) ) ;
#36105 = CARTESIAN_POINT ( 'NONE',  ( 13.35937500061451821, -4.541064518000417216, -2.621784821875001281 ) ) ;
#36106 = CARTESIAN_POINT ( 'NONE',  ( -4.243569643749997233, 10.89687500061451786, 32.45002607614398471 ) ) ;
#36107 = CARTESIAN_POINT ( 'NONE',  ( 20.77500000122903145, -5.773502691896255534, -1.060575238724906372E-15 ) ) ;
#36108 = CARTESIAN_POINT ( 'NONE',  ( 12.17812500061451608, 4.541064518000418104, 2.621784821874999949 ) ) ;
#36109 = VERTEX_POINT ( 'NONE', #59105 ) ;
#36110 = ORIENTED_EDGE ( 'NONE', *, *, #66718, .T. ) ;
#36111 = CARTESIAN_POINT ( 'NONE',  ( 19.16250000000000142, 2.886751345948126879, 4.999999999999999112 ) ) ;
#36112 = CARTESIAN_POINT ( 'NONE',  ( 4.000000000000000000, 18.29374999877096641, 30.00000000000000000 ) ) ;
#36113 = CARTESIAN_POINT ( 'NONE',  ( 11.55937500061451928, -4.541064518000417216, -2.621784821875001281 ) ) ;
#36114 = DIRECTION ( 'NONE',  ( -1.000000000000000000, -0.000000000000000000, -0.000000000000000000 ) ) ;
#36115 = ADVANCED_FACE ( 'NONE', ( #65024 ), #8512, .T. ) ;
#36116 = CARTESIAN_POINT ( 'NONE',  ( 12.60000000122903430, -2.886751345948129988, 4.999999999999997335 ) ) ;
#36117 = CARTESIAN_POINT ( 'NONE',  ( 21.78750000122903074, 6.123233995736764310E-16, -4.999999999999998224 ) ) ;
#36118 = CARTESIAN_POINT ( 'NONE',  ( 18.32812500061451644, 6.421520780324663323E-16, -5.243569643749999010 ) ) ;
#36119 = CARTESIAN_POINT ( 'NONE',  ( 21.55312500061451431, 4.541064518000418104, -2.621784821874998173 ) ) ;
#36120 = CARTESIAN_POINT ( 'NONE',  ( 26.62500000122903288, -5.773502691896255534, -1.060575238724906372E-15 ) ) ;
#36121 = CARTESIAN_POINT ( 'NONE',  ( 26.55000000000000071, -4.330127018922190985, -2.500000000000001332 ) ) ;
#36122 = CARTESIAN_POINT ( 'NONE',  ( 17.49375000122903145, -2.886751345948074920, 5.000000000000092371 ) ) ;
#36123 = VECTOR ( 'NONE', #7507, 1000.000000000000000 ) ;
#36124 = CARTESIAN_POINT ( 'NONE',  ( 7.471875000614519813, -5.492252693125287522, -1.008910452111647106E-15 ) ) ;
#36125 = CARTESIAN_POINT ( 'NONE',  ( 27.98437500061451289, 4.541064518000418104, 2.621784821874999949 ) ) ;
#36126 = CARTESIAN_POINT ( 'NONE',  ( 4.000000000000000000, 14.33750000000000213, -27.69059892324149885 ) ) ;
#36127 = CARTESIAN_POINT ( 'NONE',  ( 9.001249775931846008E-16, 16.37187500061451573, -25.09994784771203058 ) ) ;
#36128 = CARTESIAN_POINT ( 'NONE',  ( 3.150000001229034119, -2.886751345948129988, 4.999999999999997335 ) ) ;
#36129 = CARTESIAN_POINT ( 'NONE',  ( 6.299999999999999822, -4.330127018922190985, -2.500000000000001332 ) ) ;
#36130 =( BOUNDED_CURVE ( )  B_SPLINE_CURVE ( 2, ( #4087, #38798, #49514, #43975, #27345, #21782, #10711, #66495, #3722 ),
 .UNSPECIFIED., .F., .F. ) 
 B_SPLINE_CURVE_WITH_KNOTS ( ( 3, 2, 2, 2, 3 ),
 ( 0.05434782608695652717, 0.05797101449275362389, 0.06521739130434782428, 0.07246376811594203160, 0.07608695652173913526 ),
 .UNSPECIFIED. ) 
 CURVE ( )  GEOMETRIC_REPRESENTATION_ITEM ( )  RATIONAL_B_SPLINE_CURVE ( ( 0.9330127018922194093, 0.9330127018922194093, 1.000000000000000000, 0.8660254037844387076, 1.000000000000000000, 0.8660254037844387076, 1.000000000000000000, 0.9330127018922191873, 0.9330127018922192983 ) ) 
 REPRESENTATION_ITEM ( '' )  );
#36131 = CARTESIAN_POINT ( 'NONE',  ( 28.89375000122902648, -2.886751345948096237, -5.000000000000050626 ) ) ;
#36132 = CARTESIAN_POINT ( 'NONE',  ( 9.421875000614519990, 3.027376345333613106, -5.243569643749998122 ) ) ;
#36133 = CARTESIAN_POINT ( 'NONE',  ( 28.75312500061451715, 4.541064518000418104, -2.621784821874998173 ) ) ;
#36134 = CARTESIAN_POINT ( 'NONE',  ( 15.54375000122903216, 5.773502691896255534, 3.535250795749688401E-16 ) ) ;
#36135 = CARTESIAN_POINT ( 'NONE',  ( -5.605356288733176484, 8.281802244057951512, -27.85102845225483748 ) ) ;
#36136 = CARTESIAN_POINT ( 'NONE',  ( 2.000000000000001332, 17.56250000122903288, -26.53589838486224650 ) ) ;
#36137 = CARTESIAN_POINT ( 'NONE',  ( 7.284375000614518036, 4.541064518000418104, 2.621784821874999949 ) ) ;
#36138 = CARTESIAN_POINT ( 'NONE',  ( 12.19687500061451679, 6.054752690667223547, 3.707466751127219781E-16 ) ) ;
#36139 = CARTESIAN_POINT ( 'NONE',  ( 4.237500000000001599, 5.773502691896255534, 3.535250795749688894E-16 ) ) ;
#36140 = CARTESIAN_POINT ( 'NONE',  ( -4.243569643749999898, 14.40312500061459389, 30.00000000000000000 ) ) ;
#36141 = EDGE_CURVE ( 'NONE', #33565, #66841, #31416, .T. ) ;
#36142 = CARTESIAN_POINT ( 'NONE',  ( 3.470266163325922193, 25.13317678729335114, 27.99341696106071353 ) ) ;
#36143 = CARTESIAN_POINT ( 'NONE',  ( 7.200000000000001954, -4.330127018922190985, -2.500000000000001332 ) ) ;
#36144 = CARTESIAN_POINT ( 'NONE',  ( 14.14687500061451431, -4.119189519843965641, -2.378215178125001383 ) ) ;
#36145 = CARTESIAN_POINT ( 'NONE',  ( 20.50312500061451715, -4.541064518000417216, -2.621784821875001281 ) ) ;
#36146 = CARTESIAN_POINT ( 'NONE',  ( 13.71562500061451750, -6.054752690667223547, -1.112240025338166033E-15 ) ) ;
#36147 = CARTESIAN_POINT ( 'NONE',  ( 22.69687500061451502, -4.119189519843965641, -2.378215178125001383 ) ) ;
#36148 = CARTESIAN_POINT ( 'NONE',  ( 10.28437500061451715, 6.421520780324663323E-16, -5.243569643749999010 ) ) ;
#36149 = CARTESIAN_POINT ( 'NONE',  ( 25.64999999999999858, -4.330127018922190985, -2.500000000000001332 ) ) ;
#36150 = CARTESIAN_POINT ( 'NONE',  ( 22.61250000122903003, -4.330127018922190985, -2.500000000000001332 ) ) ;
#36151 = CARTESIAN_POINT ( 'NONE',  ( 16.98750000000000426, -2.886751345948096681, 5.000000000000054179 ) ) ;
#36152 = CARTESIAN_POINT ( 'NONE',  ( 12.38437500061451857, -4.541064518000419881, 2.621784821874995952 ) ) ;
#36153 = CARTESIAN_POINT ( 'NONE',  ( 25.84687500061451360, -3.027376345333614438, 5.243569643749998122 ) ) ;
#36154 = CARTESIAN_POINT ( 'NONE',  ( 3.646875000614520079, 6.054752690667223547, 3.707466751127219781E-16 ) ) ;
#36155 = CARTESIAN_POINT ( 'NONE',  ( 30.00000000000000000, 0.000000000000000000, 4.999999999999998224 ) ) ;
#36156 = CARTESIAN_POINT ( 'NONE',  ( 18.83437500061451431, 6.421520780324663323E-16, -5.243569643749999010 ) ) ;
#36157 = CARTESIAN_POINT ( 'NONE',  ( 11.89687500061451608, -3.027376345333614438, 5.243569643749998122 ) ) ;
#36158 = CARTESIAN_POINT ( 'NONE',  ( 1.878215178124997609, 13.01562499938548356, 33.25316411605952993 ) ) ;
#36159 = CARTESIAN_POINT ( 'NONE',  ( 22.80000000000000071, 0.000000000000000000, 4.999999999999998224 ) ) ;
#36160 = CARTESIAN_POINT ( 'NONE',  ( -4.000000000000000000, 12.72499999999999964, 30.00000000000000000 ) ) ;
#36161 = CARTESIAN_POINT ( 'NONE',  ( 2.121784821875001281, 13.25937500061451857, -26.32496088578401938 ) ) ;
#36162 = CARTESIAN_POINT ( 'NONE',  ( 24.68437500061451573, 5.824947211148865298E-16, -4.756430356249998326 ) ) ;
#36163 = CARTESIAN_POINT ( 'NONE',  ( 14.01562500061451644, 3.027376345333611329, 5.243569643749999010 ) ) ;
#36164 = CARTESIAN_POINT ( 'NONE',  ( 4.387500000000002842, -2.886751345948129988, 4.999999999999997335 ) ) ;
#36165 = CARTESIAN_POINT ( 'NONE',  ( 29.80312500061451431, 0.000000000000000000, 5.243569643749999010 ) ) ;
#36166 = DIRECTION ( 'NONE',  ( -1.000000000000000000, -0.000000000000000000, -0.000000000000000000 ) ) ;
#36167 = CARTESIAN_POINT ( 'NONE',  ( 14.92500000000000071, 6.123233995736764310E-16, -4.999999999999998224 ) ) ;
#36168 = CARTESIAN_POINT ( 'NONE',  ( -3.999999999999999112, 19.66250000122903430, 30.00000000000000000 ) ) ;
#36169 = CARTESIAN_POINT ( 'NONE',  ( 13.23750000122903359, 6.123233995736764310E-16, -4.999999999999998224 ) ) ;
#36170 = CARTESIAN_POINT ( 'NONE',  ( 25.54687500061451644, -3.027376345333610441, -5.243569643749999898 ) ) ;
#36171 = CARTESIAN_POINT ( 'NONE',  ( 20.40000000122903501, -2.886751345948092684, -5.000000000000057732 ) ) ;
#36172 = VECTOR ( 'NONE', #25494, 1000.000000000000000 ) ;
#36173 = ORIENTED_EDGE ( 'NONE', *, *, #8082, .T. ) ;
#36174 = CARTESIAN_POINT ( 'NONE',  ( 20.20312500061451644, 4.541064518000418104, -2.621784821874998173 ) ) ;
#36175 = CARTESIAN_POINT ( 'NONE',  ( 4.715625000614516615, -6.054752690667223547, -1.112240025338166033E-15 ) ) ;
#36176 = CARTESIAN_POINT ( 'NONE',  ( 18.87187500061451573, 3.027376345333613106, -5.243569643749998122 ) ) ;
#36177 = CARTESIAN_POINT ( 'NONE',  ( 28.39687500061452141, 6.054752690667223547, 3.707466751127219781E-16 ) ) ;
#36178 = CARTESIAN_POINT ( 'NONE',  ( 6.928125000614516082, -4.541064518000419881, 2.621784821874995952 ) ) ;
#36179 = CARTESIAN_POINT ( 'NONE',  ( 22.79062500061451502, -3.027376345333610441, -5.243569643749999898 ) ) ;
#36180 = CARTESIAN_POINT ( 'NONE',  ( 2.121784821875001281, 15.90312500061451573, 33.67503911421598417 ) ) ;
#36181 = CARTESIAN_POINT ( 'NONE',  ( 18.67500000122903714, 2.886751345948129099, -4.999999999999998224 ) ) ;
#36182 = CARTESIAN_POINT ( 'NONE',  ( 13.28437500061451715, -4.119189519843968306, 2.378215178124996054 ) ) ;
#36183 = CARTESIAN_POINT ( 'NONE',  ( 8.278125000614515727, -4.541064518000419881, 2.621784821874995952 ) ) ;
#36184 = CARTESIAN_POINT ( 'NONE',  ( 3.459375000614519635, -4.541064518000417216, -2.621784821875001281 ) ) ;
#36185 = CARTESIAN_POINT ( 'NONE',  ( 29.72812500061451502, 4.541064518000418104, 2.621784821874999949 ) ) ;
#36186 = CARTESIAN_POINT ( 'NONE',  ( 21.87187500061451573, -6.054752690667223547, -1.112240025338166033E-15 ) ) ;
#36187 = CARTESIAN_POINT ( 'NONE',  ( 14.80312500061451608, 4.541064518000418104, -2.621784821874998173 ) ) ;
#36188 = CARTESIAN_POINT ( 'NONE',  ( 23.85000000122903430, -2.886751345948129988, 4.999999999999997335 ) ) ;
#36189 = CARTESIAN_POINT ( 'NONE',  ( 24.85312500061451502, 0.000000000000000000, 5.243569643749999010 ) ) ;
#36190 = CARTESIAN_POINT ( 'NONE',  ( 19.92187500061451644, 3.027376345333611329, 5.243569643749999010 ) ) ;
#36191 = CARTESIAN_POINT ( 'NONE',  ( 15.06562500061451537, -6.054752690667223547, -1.112240025338166033E-15 ) ) ;
#36192 = CARTESIAN_POINT ( 'NONE',  ( 2.121784821874999061, 16.10937500061451644, 26.32496088578401583 ) ) ;
#36193 = CARTESIAN_POINT ( 'NONE',  ( 20.31562500061451715, 3.027376345333611329, 5.243569643749999010 ) ) ;
#36194 = CARTESIAN_POINT ( 'NONE',  ( 29.50312500061451360, -4.541064518000417216, -2.621784821875001281 ) ) ;
#36195 = VERTEX_POINT ( 'NONE', #35849 ) ;
#36196 = CARTESIAN_POINT ( 'NONE',  ( 26.06250000000000000, -5.773502691896255534, -1.060575238724906372E-15 ) ) ;
#36197 = CARTESIAN_POINT ( 'NONE',  ( 1.999999999999998668, 11.30000000000000071, -33.46410161513775705 ) ) ;
#36198 = CARTESIAN_POINT ( 'NONE',  ( 25.33125000122903003, 6.123233995736764310E-16, -4.999999999999998224 ) ) ;
#36199 = CARTESIAN_POINT ( 'NONE',  ( 26.65312500061451573, 0.000000000000000000, 5.243569643749999010 ) ) ;
#36200 = CARTESIAN_POINT ( 'NONE',  ( 7.903125000614515727, -4.541064518000417216, -2.621784821875001281 ) ) ;
#36201 = CARTESIAN_POINT ( 'NONE',  ( 20.88750000122903572, 6.123233995736764310E-16, -4.999999999999998224 ) ) ;
#36202 = CARTESIAN_POINT ( 'NONE',  ( 24.66562500061451502, 3.027376345333613106, -5.243569643749998122 ) ) ;
#36203 = CARTESIAN_POINT ( 'NONE',  ( 24.75000000000000000, -4.330127018922190985, -2.500000000000001332 ) ) ;
#36204 = CARTESIAN_POINT ( 'NONE',  ( 3.999999999999998668, 15.42500000122903359, -32.30940107675850470 ) ) ;
#36205 = EDGE_CURVE ( 'NONE', #27078, #43803, #21226, .T. ) ;
#36206 = CARTESIAN_POINT ( 'NONE',  ( 28.37812500061451715, 4.541064518000418104, 2.621784821874999949 ) ) ;
#36207 = CARTESIAN_POINT ( 'NONE',  ( 11.54062500061451857, -3.027376345333610441, -5.243569643749999898 ) ) ;
#36208 = ORIENTED_EDGE ( 'NONE', *, *, #4157, .F. ) ;
#36209 = B_SPLINE_CURVE_WITH_KNOTS ( 'NONE', 3,
 ( #22155, #50248, #40603, #56143, #23236, #51688, #28425, #33959, #6256, #50962 ),
 .UNSPECIFIED., .F., .F.,
 ( 4, 3, 3, 4 ),
 ( 1.837010936913719881E-16, 0.0001572264585416875324, 0.0003144530955621989074, 0.0005640517951500036587 ),
 .UNSPECIFIED. ) ;
#36210 = CARTESIAN_POINT ( 'NONE',  ( 25.45312500061451644, -4.541064518000417216, -2.621784821875001281 ) ) ;
#36211 = CARTESIAN_POINT ( 'NONE',  ( 4.603125000614518569, 0.000000000000000000, 5.243569643749999010 ) ) ;
#36212 = CARTESIAN_POINT ( 'NONE',  ( 13.73437500061451821, -4.119189519843968306, 2.378215178124996054 ) ) ;
#36213 = PLANE ( 'NONE',  #69206 ) ;
#36214 = CIRCLE ( 'NONE', #20862, 9.000000000000000000 ) ;
#36215 = VECTOR ( 'NONE', #68638, 1000.000000000000000 ) ;
#36216 = CARTESIAN_POINT ( 'NONE',  ( 12.26249999999999929, 2.886751345948129099, -4.999999999999998224 ) ) ;
#36217 = CARTESIAN_POINT ( 'NONE',  ( 14.63437500061451679, -4.541064518000419881, 2.621784821874995952 ) ) ;
#36218 = CARTESIAN_POINT ( 'NONE',  ( 7.725000001229034297, -5.773502691896255534, -1.060575238724906372E-15 ) ) ;
#36219 = CARTESIAN_POINT ( 'NONE',  ( 17.33437500061451431, -4.541064518000419881, 2.621784821874995952 ) ) ;
#36220 = CARTESIAN_POINT ( 'NONE',  ( 15.26249999999999929, -5.773502691896255534, -1.060575238724906372E-15 ) ) ;
#36221 = CARTESIAN_POINT ( 'NONE',  ( 9.009375000614518569, 4.541064518000418104, -2.621784821874998173 ) ) ;
#36222 = CARTESIAN_POINT ( 'NONE',  ( -3.000416591977282496E-16, 12.49062500061451608, -34.90005215228797653 ) ) ;
#36223 = DIRECTION ( 'NONE',  ( 0.000000000000000000, 0.000000000000000000, 1.000000000000000000 ) ) ;
#36224 = CARTESIAN_POINT ( 'NONE',  ( 23.25937500061451857, 2.746126346562645981, -4.756430356249997438 ) ) ;
#36225 = VERTEX_POINT ( 'NONE', #47668 ) ;
#36226 = CARTESIAN_POINT ( 'NONE',  ( 24.14062500061451289, -3.027376345333610441, -5.243569643749999898 ) ) ;
#36227 = CARTESIAN_POINT ( 'NONE',  ( -2.121784821874999949, 11.23437500061451821, 26.32496088578401938 ) ) ;
#36228 = CARTESIAN_POINT ( 'NONE',  ( 21.26250000122903572, -4.330127018922190985, -2.500000000000001332 ) ) ;
#36229 = CARTESIAN_POINT ( 'NONE',  ( 25.13437500061451502, 6.421520780324663323E-16, -5.243569643749999010 ) ) ;
#36230 = CARTESIAN_POINT ( 'NONE',  ( 28.17187500061451644, -6.054752690667223547, -1.112240025338166033E-15 ) ) ;
#36231 = CARTESIAN_POINT ( 'NONE',  ( 21.67500000000000071, 6.123233995736764310E-16, -4.999999999999998224 ) ) ;
#36232 = ADVANCED_FACE ( 'NONE', ( #42134 ), #64660, .F. ) ;
#36233 = CARTESIAN_POINT ( 'NONE',  ( 5.428125000614517859, 4.541064518000418104, 2.621784821874999949 ) ) ;
#36234 = CARTESIAN_POINT ( 'NONE',  ( 21.53437500061451360, 5.492252693125287522, 3.363034840372157021E-16 ) ) ;
#36235 = CARTESIAN_POINT ( 'NONE',  ( 16.80937500061451573, 0.000000000000000000, 5.243569643749999010 ) ) ;
#36236 = CARTESIAN_POINT ( 'NONE',  ( 9.946875000614516793, 0.000000000000000000, 4.756430356249998326 ) ) ;
#36237 = CARTESIAN_POINT ( 'NONE',  ( 29.51250000122903216, 4.330127018922192761, -2.499999999999997780 ) ) ;
#36238 = CARTESIAN_POINT ( 'NONE',  ( 8.484375000614518214, 6.421520780324663323E-16, -5.243569643749999010 ) ) ;
#36239 = CARTESIAN_POINT ( 'NONE',  ( 20.18437500061451573, 6.421520780324663323E-16, -5.243569643749999010 ) ) ;
#36240 = CARTESIAN_POINT ( 'NONE',  ( -1.774630419999661868, 25.43662396648353408, 33.59426316867342166 ) ) ;
#36241 = CARTESIAN_POINT ( 'NONE',  ( 26.69999999999999929, 4.330127018922192761, -2.499999999999997780 ) ) ;
#36242 = CARTESIAN_POINT ( 'NONE',  ( 28.35937500061451289, 4.541064518000418104, -2.621784821874998173 ) ) ;
#36243 = CARTESIAN_POINT ( 'NONE',  ( 3.486133158594716510E-16, 19.88749999999999929, 26.00000000000000355 ) ) ;
#36244 = CARTESIAN_POINT ( 'NONE',  ( 21.78750000000000142, 5.773502691896255534, 3.535250795749688401E-16 ) ) ;
#36245 = EDGE_LOOP ( 'NONE', ( #72430, #24061, #31671, #63363 ) ) ;
#36246 = CARTESIAN_POINT ( 'NONE',  ( 8.025000000000000355, -4.330127018922194537, 2.499999999999995559 ) ) ;
#36247 = CARTESIAN_POINT ( 'NONE',  ( 11.33437500061451431, -2.746126346562646425, 4.756430356249996549 ) ) ;
#36248 = CARTESIAN_POINT ( 'NONE',  ( 20.99062500061451431, -3.027376345333610441, -5.243569643749999898 ) ) ;
#36249 = CARTESIAN_POINT ( 'NONE',  ( 10.91250000000000320, 2.886751345948129099, -4.999999999999998224 ) ) ;
#36250 = CARTESIAN_POINT ( 'NONE',  ( 8.812500001229034652, 4.330127018922192761, -2.499999999999997780 ) ) ;
#36251 = CARTESIAN_POINT ( 'NONE',  ( 5.915625000614515905, 3.027376345333611329, 5.243569643749999010 ) ) ;
#36252 = CARTESIAN_POINT ( 'NONE',  ( 21.37499999999999645, 4.330127018922191873, 2.499999999999999556 ) ) ;
#36253 = CARTESIAN_POINT ( 'NONE',  ( 21.89062500061451289, -3.027376345333610441, -5.243569643749999898 ) ) ;
#36254 = CARTESIAN_POINT ( 'NONE',  ( 23.69999999999999929, 0.000000000000000000, 4.999999999999998224 ) ) ;
#36255 = CARTESIAN_POINT ( 'NONE',  ( 26.70000000122903572, -2.886751345948125991, -5.000000000000000000 ) ) ;
#36256 = CARTESIAN_POINT ( 'NONE',  ( 0.6522972858965978560, 20.64114861271052348, 33.69936173848522998 ) ) ;
#36257 = CARTESIAN_POINT ( 'NONE',  ( 3.937500000000000444, -2.886751345948129988, 4.999999999999997335 ) ) ;
#36258 = ORIENTED_EDGE ( 'NONE', *, *, #21481, .F. ) ;
#36259 = CARTESIAN_POINT ( 'NONE',  ( 20.12812500061451715, 6.421520780324663323E-16, -5.243569643749999010 ) ) ;
#36260 = CARTESIAN_POINT ( 'NONE',  ( 27.25312500061451360, -4.541064518000417216, -2.621784821875001281 ) ) ;
#36261 = CARTESIAN_POINT ( 'NONE',  ( 26.55937500061451573, 4.541064518000418104, -2.621784821874998173 ) ) ;
#36262 = CARTESIAN_POINT ( 'NONE',  ( 12.37500000000000000, 4.330127018922191873, 2.499999999999999556 ) ) ;
#36263 = CARTESIAN_POINT ( 'NONE',  ( 13.67812500061451786, -4.541064518000419881, 2.621784821874995952 ) ) ;
#36264 = CARTESIAN_POINT ( 'NONE',  ( 28.22812500061451502, 6.421520780324663323E-16, -5.243569643749999010 ) ) ;
#36265 = CARTESIAN_POINT ( 'NONE',  ( 10.19062500061451892, -3.027376345333610441, -5.243569643749999898 ) ) ;
#36266 = CARTESIAN_POINT ( 'NONE',  ( 29.77499999999999858, 6.123233995736764310E-16, -4.999999999999998224 ) ) ;
#36267 = CARTESIAN_POINT ( 'NONE',  ( -3.000416591977282496E-16, 12.54687500061451999, 25.09994784771203058 ) ) ;
#36268 = VECTOR ( 'NONE', #45294, 1000.000000000000000 ) ;
#36269 = CARTESIAN_POINT ( 'NONE',  ( 25.65000000122903145, -2.886751345948129988, 4.999999999999997335 ) ) ;
#36270 = CARTESIAN_POINT ( 'NONE',  ( 19.54687500061451289, -2.746126346562646425, 4.756430356249996549 ) ) ;
#36271 = CARTESIAN_POINT ( 'NONE',  ( 17.54062500061451502, 6.054752690667223547, 3.707466751127219781E-16 ) ) ;
#36272 = DIRECTION ( 'NONE',  ( 0.000000000000000000, 0.000000000000000000, -1.000000000000000000 ) ) ;
#36273 = CARTESIAN_POINT ( 'NONE',  ( 11.29687500061451644, 6.054752690667223547, 3.707466751127219781E-16 ) ) ;
#36274 = CARTESIAN_POINT ( 'NONE',  ( 9.946875000614516793, 6.054752690667223547, 3.707466751127219781E-16 ) ) ;
#36275 = CARTESIAN_POINT ( 'NONE',  ( 17.52187500061451431, 3.027376345333613106, -5.243569643749998122 ) ) ;
#36276 = ORIENTED_EDGE ( 'NONE', *, *, #54349, .F. ) ;
#36277 = CARTESIAN_POINT ( 'NONE',  ( 29.40937500061451715, 0.000000000000000000, 5.243569643749999010 ) ) ;
#36278 = CARTESIAN_POINT ( 'NONE',  ( 21.47812500061451502, 6.421520780324663323E-16, -5.243569643749999010 ) ) ;
#36279 = CARTESIAN_POINT ( 'NONE',  ( 15.34687500061451537, 6.054752690667223547, 3.707466751127219781E-16 ) ) ;
#36280 = CARTESIAN_POINT ( 'NONE',  ( 21.36562500061451431, -6.054752690667223547, -1.112240025338166033E-15 ) ) ;
#36281 = CARTESIAN_POINT ( 'NONE',  ( 3.999999999999999112, 13.47500000000000142, 30.00000000000000000 ) ) ;
#36282 = CARTESIAN_POINT ( 'NONE',  ( 26.76562500061451644, -6.054752690667223547, -1.112240025338166033E-15 ) ) ;
#36283 = CARTESIAN_POINT ( 'NONE',  ( 9.450000001229033941, -2.886751345948129988, 4.999999999999997335 ) ) ;
#36284 = ORIENTED_EDGE ( 'NONE', *, *, #26884, .T. ) ;
#36285 = CARTESIAN_POINT ( 'NONE',  ( 4.237500001229036251, 6.123233995736764310E-16, -4.999999999999998224 ) ) ;
#36286 = CARTESIAN_POINT ( 'NONE',  ( 3.999999999999999112, 18.87500000000000000, -30.00000000000000000 ) ) ;
#36287 = CARTESIAN_POINT ( 'NONE',  ( 24.71250000122903145, 0.000000000000000000, 4.999999999999998224 ) ) ;
#36288 = CARTESIAN_POINT ( 'NONE',  ( 1.999999999999997335, 20.01874999877096428, 33.46410161513775705 ) ) ;
#36289 = CARTESIAN_POINT ( 'NONE',  ( 6.046875000614519102, -3.027376345333614438, 5.243569643749998122 ) ) ;
#36290 = CARTESIAN_POINT ( 'NONE',  ( 1.592000809091587073E-14, 15.38750000000000284, 26.00000000000000000 ) ) ;
#36291 = CARTESIAN_POINT ( 'NONE',  ( 14.42812500061451786, 4.541064518000418104, 2.621784821874999949 ) ) ;
#36292 = CARTESIAN_POINT ( 'NONE',  ( 8.521875000614516082, 3.027376345333613106, -5.243569643749998122 ) ) ;
#36293 = CARTESIAN_POINT ( 'NONE',  ( 27.56250000122902932, -4.330127018922190985, -2.500000000000001332 ) ) ;
#36294 = CARTESIAN_POINT ( 'NONE',  ( 16.47187500061452070, -6.054752690667223547, -1.112240025338166033E-15 ) ) ;
#36295 = CARTESIAN_POINT ( 'NONE',  ( 5.521875000614517859, 3.027376345333611329, 5.243569643749999010 ) ) ;
#36296 = LINE ( 'NONE', #25576, #65119 ) ;
#36297 =( BOUNDED_CURVE ( )  B_SPLINE_CURVE ( 2, ( #50245, #11068, #27704, #33240, #50958, #22863, #67595 ),
 .UNSPECIFIED., .F., .F. ) 
 B_SPLINE_CURVE_WITH_KNOTS ( ( 3, 2, 2, 3 ),
 ( 0.9259902657761827083, 0.9277777777777778123, 0.9305555555555555802, 0.9321263668030935756 ),
 .UNSPECIFIED. ) 
 CURVE ( )  GEOMETRIC_REPRESENTATION_ITEM ( )  RATIONAL_B_SPLINE_CURVE ( ( 0.9385307109133473880, 0.9137867684880971453, 1.000000000000000000, 0.8660254037844387076, 1.000000000000000000, 0.9242384310568843020, 0.9341619918451884441 ) ) 
 REPRESENTATION_ITEM ( '' )  );
#36298 = CARTESIAN_POINT ( 'NONE',  ( 6.665625000614515905, 3.027376345333613106, -5.243569643749998122 ) ) ;
#36299 = CARTESIAN_POINT ( 'NONE',  ( 18.06562500061451715, 3.027376345333611329, 5.243569643749999010 ) ) ;
#36300 = VERTEX_POINT ( 'NONE', #37320 ) ;
#36301 = CARTESIAN_POINT ( 'NONE',  ( 13.30312500061451786, -4.541064518000417216, -2.621784821875001281 ) ) ;
#36302 = CARTESIAN_POINT ( 'NONE',  ( 5.587500001229033231, 6.123233995736764310E-16, -4.999999999999998224 ) ) ;
#36303 = CARTESIAN_POINT ( 'NONE',  ( 11.61562500061451608, 3.027376345333613106, -5.243569643749998122 ) ) ;
#36304 = CARTESIAN_POINT ( 'NONE',  ( 21.34687500061451715, -2.746126346562646425, 4.756430356249996549 ) ) ;
#36305 = CARTESIAN_POINT ( 'NONE',  ( 12.03749999999999964, -2.886751345948129988, 4.999999999999997335 ) ) ;
#36306 = CARTESIAN_POINT ( 'NONE',  ( 6.187500001229032875, 4.330127018922191873, 2.499999999999999556 ) ) ;
#36307 = CARTESIAN_POINT ( 'NONE',  ( 14.97187500061451892, 3.027376345333611329, 5.243569643749999010 ) ) ;
#36308 = CARTESIAN_POINT ( 'NONE',  ( 15.97500000122903430, 2.886751345948129099, -4.999999999999998224 ) ) ;
#36309 = CARTESIAN_POINT ( 'NONE',  ( 23.85000000000000142, -4.330127018922190985, -2.500000000000001332 ) ) ;
#36310 = CARTESIAN_POINT ( 'NONE',  ( 2.121784821875001281, 19.05312500061451431, -26.32496088578401938 ) ) ;
#36311 = CARTESIAN_POINT ( 'NONE',  ( -2.498395430326213790E-14, 20.26249999999999929, 26.00000000000000000 ) ) ;
#36312 = CARTESIAN_POINT ( 'NONE',  ( 4.000000000000000000, 16.04374999877096641, 30.00000000000000000 ) ) ;
#36313 = CARTESIAN_POINT ( 'NONE',  ( 4.359375000614517326, -4.541064518000417216, -2.621784821875001281 ) ) ;
#36314 = DIRECTION ( 'NONE',  ( -1.000000000000000000, -0.000000000000000000, -0.000000000000000000 ) ) ;
#36315 = CARTESIAN_POINT ( 'NONE',  ( 4.898734551532200499, 1.001199177798645534, 4.898734551532190729 ) ) ;
#36316 = CARTESIAN_POINT ( 'NONE',  ( 14.89687500061451786, 6.054752690667223547, 3.707466751127219781E-16 ) ) ;
#36317 = CARTESIAN_POINT ( 'NONE',  ( 28.23750000000000426, -2.886751345948129988, 4.999999999999997335 ) ) ;
#36318 = EDGE_CURVE ( 'NONE', #48564, #63279, #3353, .T. ) ;
#36319 = CARTESIAN_POINT ( 'NONE',  ( 13.97812500061451679, 4.541064518000418104, 2.621784821874999949 ) ) ;
#36320 = CARTESIAN_POINT ( 'NONE',  ( 28.80937500061451217, 2.746126346562643317, 4.756430356249998326 ) ) ;
#36321 = CARTESIAN_POINT ( 'NONE',  ( 24.87187500061451573, 3.027376345333611329, 5.243569643749999010 ) ) ;
#36322 = CARTESIAN_POINT ( 'NONE',  ( 15.64687500061451608, 4.119189519843966529, -2.378215178124998275 ) ) ;
#36323 = CARTESIAN_POINT ( 'NONE',  ( 11.12812500061451715, 6.421520780324663323E-16, -5.243569643749999010 ) ) ;
#36324 = CARTESIAN_POINT ( 'NONE',  ( 16.73437500061451644, 4.541064518000418104, 2.621784821874999949 ) ) ;
#36325 = ORIENTED_EDGE ( 'NONE', *, *, #10637, .F. ) ;
#36326 = CARTESIAN_POINT ( 'NONE',  ( 25.92187500061451999, -6.054752690667223547, -1.112240025338166033E-15 ) ) ;
#36327 = CARTESIAN_POINT ( 'NONE',  ( 28.30312500061451431, 4.541064518000418104, -2.621784821874998173 ) ) ;
#36328 = CARTESIAN_POINT ( 'NONE',  ( 18.89062500061451644, 6.054752690667223547, 3.707466751127219781E-16 ) ) ;
#36329 = CARTESIAN_POINT ( 'NONE',  ( 28.90312500061451217, 0.000000000000000000, 5.243569643749999010 ) ) ;
#36330 = CARTESIAN_POINT ( 'NONE',  ( 4.854756222371646501, 1.196571399816914738, -5.105259861685001788 ) ) ;
#36331 =( BOUNDED_CURVE ( )  B_SPLINE_CURVE ( 2, ( #18761, #24678, #47225, #30596, #2884, #59380, #70849 ),
 .UNSPECIFIED., .F., .F. ) 
 B_SPLINE_CURVE_WITH_KNOTS ( ( 3, 2, 2, 3 ),
 ( 0.8000000000000000444, 0.8027777777777778123, 0.8055555555555555802, 0.8083333333333333481 ),
 .UNSPECIFIED. ) 
 CURVE ( )  GEOMETRIC_REPRESENTATION_ITEM ( )  RATIONAL_B_SPLINE_CURVE ( ( 1.000000000000000000, 0.8660254037844387076, 1.000000000000000000, 0.8660254037844387076, 1.000000000000000000, 0.8660254037844387076, 1.000000000000000000 ) ) 
 REPRESENTATION_ITEM ( '' )  );
#36332 = CARTESIAN_POINT ( 'NONE',  ( 7.724999999999999645, 6.123233995736764310E-16, -4.999999999999998224 ) ) ;
#36333 = CARTESIAN_POINT ( 'NONE',  ( 18.63750000122903216, 6.123233995736764310E-16, -4.999999999999998224 ) ) ;
#36334 = CARTESIAN_POINT ( 'NONE',  ( 1.626862140677534273E-15, 10.21250000000000036, 34.00000000000000000 ) ) ;
#36335 = CARTESIAN_POINT ( 'NONE',  ( 8.484375000614518214, 5.492252693125287522, 3.363034840372157021E-16 ) ) ;
#36336 = ORIENTED_EDGE ( 'NONE', *, *, #63436, .T. ) ;
#36337 = CARTESIAN_POINT ( 'NONE',  ( 17.62500000000000000, 6.123233995736764310E-16, -4.999999999999998224 ) ) ;
#36338 = CARTESIAN_POINT ( 'NONE',  ( 19.98749999999999716, 5.773502691896255534, 3.535250795749688894E-16 ) ) ;
#36339 = CARTESIAN_POINT ( 'NONE',  ( 16.50937500061451502, -4.541064518000417216, -2.621784821875001281 ) ) ;
#36340 = CARTESIAN_POINT ( 'NONE',  ( 13.26562500061451644, -6.054752690667223547, -1.112240025338166033E-15 ) ) ;
#36341 = ORIENTED_EDGE ( 'NONE', *, *, #69921, .F. ) ;
#36342 = CARTESIAN_POINT ( 'NONE',  ( 5.465625000614517504, 3.027376345333611329, 5.243569643749999010 ) ) ;
#36343 = DIRECTION ( 'NONE',  ( -1.000000000000000000, -0.000000000000000000, -0.000000000000000000 ) ) ;
#36344 = CARTESIAN_POINT ( 'NONE',  ( 13.19999999999999929, 4.330127018922192761, -2.499999999999997780 ) ) ;
#36345 = CARTESIAN_POINT ( 'NONE',  ( 29.74687500061451573, 0.000000000000000000, 4.756430356249998326 ) ) ;
#36346 = CARTESIAN_POINT ( 'NONE',  ( -4.243569643749999898, 14.40312500061451750, 30.00000000000000000 ) ) ;
#36347 = CARTESIAN_POINT ( 'NONE',  ( 26.39062500061451644, -3.027376345333610441, -5.243569643749999898 ) ) ;
#36348 = MECHANICAL_DESIGN_GEOMETRIC_PRESENTATION_REPRESENTATION (  '', ( #13656 ), #15568 ) ;
#36349 = CARTESIAN_POINT ( 'NONE',  ( 7.800000000000001599, 4.330127018922192761, -2.499999999999997780 ) ) ;
#36350 = CARTESIAN_POINT ( 'NONE',  ( 1.878215178124997609, 17.06562499938548072, 33.25316411605952993 ) ) ;
#36351 = CARTESIAN_POINT ( 'NONE',  ( 24.34687500061451715, 6.054752690667223547, 3.707466751127219781E-16 ) ) ;
#36352 = CARTESIAN_POINT ( 'NONE',  ( 20.84062500061451573, -3.027376345333614438, 5.243569643749998122 ) ) ;
#36353 = PRODUCT_DEFINITION ( 'UNKNOWN', '', #50949, #12223 ) ;
#36354 = CARTESIAN_POINT ( 'NONE',  ( 4.243569643749999898, 15.49062500061459779, -27.54997392385601529 ) ) ;
#36355 = CARTESIAN_POINT ( 'NONE',  ( 7.190625000614518036, 6.054752690667223547, 3.707466751127219781E-16 ) ) ;
#36356 = CARTESIAN_POINT ( 'NONE',  ( 25.73437500061451644, 4.119189519843966529, 2.378215178124999607 ) ) ;
#36357 = CARTESIAN_POINT ( 'NONE',  ( 23.61562500061451786, -6.054752690667223547, -1.112240025338166033E-15 ) ) ;
#36358 = CARTESIAN_POINT ( 'NONE',  ( 10.65937500061451715, -4.119189519843965641, -2.378215178125001383 ) ) ;
#36359 = CARTESIAN_POINT ( 'NONE',  ( 2.655984681222220721E-16, 15.90312499938548108, 25.66244784525396483 ) ) ;
#36360 = CARTESIAN_POINT ( 'NONE',  ( 17.93437500061451928, 6.421520780324663323E-16, -5.243569643749999010 ) ) ;
#36361 = CARTESIAN_POINT ( 'NONE',  ( 25.05937500061451573, -4.541064518000417216, -2.621784821875001281 ) ) ;
#36362 = CARTESIAN_POINT ( 'NONE',  ( -4.243569643749998122, 14.94687500061451679, 32.45002607614398471 ) ) ;
#36363 = CARTESIAN_POINT ( 'NONE',  ( 4.378125000614518925, 6.421520780324663323E-16, -5.243569643749999010 ) ) ;
#36364 = CARTESIAN_POINT ( 'NONE',  ( 28.90312500061451217, 0.000000000000000000, 5.243569643749999010 ) ) ;
#36365 =( BOUNDED_CURVE ( )  B_SPLINE_CURVE ( 2, ( #67704, #56961, #57328, #51436, #838, #68427, #46254 ),
 .UNSPECIFIED., .F., .F. ) 
 B_SPLINE_CURVE_WITH_KNOTS ( ( 3, 2, 2, 3 ),
 ( 0.3999999999999999112, 0.4027777777777777346, 0.4055555555555555580, 0.4083333333333333814 ),
 .UNSPECIFIED. ) 
 CURVE ( )  GEOMETRIC_REPRESENTATION_ITEM ( )  RATIONAL_B_SPLINE_CURVE ( ( 1.000000000000005329, 0.8660254037844333785, 1.000000000000000000, 0.8660254037844387076, 1.000000000000000000, 0.8660254037844360431, 1.000000000000002665 ) ) 
 REPRESENTATION_ITEM ( '' )  );
#36366 = CARTESIAN_POINT ( 'NONE',  ( 29.76562500061451644, 3.027376345333611329, 5.243569643749999010 ) ) ;
#36367 = CARTESIAN_POINT ( 'NONE',  ( 5.878125000614517148, 4.541064518000418104, 2.621784821874999949 ) ) ;
#36368 = CARTESIAN_POINT ( 'NONE',  ( 9.196875000614518569, -3.027376345333614438, 5.243569643749998122 ) ) ;
#36369 = CARTESIAN_POINT ( 'NONE',  ( 16.65000000122903501, -2.886751345948129988, 4.999999999999997335 ) ) ;
#36370 = CARTESIAN_POINT ( 'NONE',  ( 3.909375000614518481, -4.541064518000417216, -2.621784821875001281 ) ) ;
#36371 = CARTESIAN_POINT ( 'NONE',  ( 5.203125000614518214, -4.541064518000417216, -2.621784821875001281 ) ) ;
#36372 = FACE_OUTER_BOUND ( 'NONE', #70627, .T. ) ;
#36373 = CARTESIAN_POINT ( 'NONE',  ( 20.83125000122903359, 6.123233995736764310E-16, -4.999999999999998224 ) ) ;
#36374 = CARTESIAN_POINT ( 'NONE',  ( 13.47187500061451537, 3.027376345333613106, -5.243569643749998122 ) ) ;
#36375 = CARTESIAN_POINT ( 'NONE',  ( 3.999999999999998668, 19.15624999877096712, 32.30940107675850470 ) ) ;
#36376 = EDGE_LOOP ( 'NONE', ( #58926, #20347, #37529, #64912 ) ) ;
#36377 = CARTESIAN_POINT ( 'NONE',  ( 21.02812500061451573, 6.421520780324663323E-16, -5.243569643749999010 ) ) ;
#36378 = CARTESIAN_POINT ( 'NONE',  ( 8.090625000614515727, 6.054752690667223547, 3.707466751127219781E-16 ) ) ;
#36379 = CARTESIAN_POINT ( 'NONE',  ( 23.55937500061451573, 0.000000000000000000, 5.243569643749999010 ) ) ;
#36380 = CARTESIAN_POINT ( 'NONE',  ( 6.628125000614517148, 6.421520780324663323E-16, -5.243569643749999010 ) ) ;
#36381 = CARTESIAN_POINT ( 'NONE',  ( 8.006250001229034297, 0.000000000000000000, 4.999999999999998224 ) ) ;
#36382 = CARTESIAN_POINT ( 'NONE',  ( 10.57500000122903572, 2.886751345948129099, -4.999999999999998224 ) ) ;
#36383 = ADVANCED_FACE ( 'NONE', ( #63925 ), #65388, .F. ) ;
#36384 = CARTESIAN_POINT ( 'NONE',  ( 25.86562500061451431, -6.054752690667223547, -1.112240025338166033E-15 ) ) ;
#36385 = CARTESIAN_POINT ( 'NONE',  ( -2.828200636599751609E-16, 19.55000000122903359, -34.61880215351700230 ) ) ;
#36386 = CARTESIAN_POINT ( 'NONE',  ( 9.787500001229036073, 4.330127018922191873, 2.499999999999999556 ) ) ;
#36387 =( BOUNDED_CURVE ( )  B_SPLINE_CURVE ( 2, ( #64197, #64931, #57924, #8416, #8784, #70110, #12866 ),
 .UNSPECIFIED., .F., .F. ) 
 B_SPLINE_CURVE_WITH_KNOTS ( ( 3, 2, 2, 3 ),
 ( 0.8000000000000000444, 0.8033333333333333437, 0.8066666666666666430, 0.8100000000000000533 ),
 .UNSPECIFIED. ) 
 CURVE ( )  GEOMETRIC_REPRESENTATION_ITEM ( )  RATIONAL_B_SPLINE_CURVE ( ( 1.000000000000000000, 0.8660254037844387076, 1.000000000000000000, 0.8660254037844387076, 1.000000000000000000, 0.8660254037844387076, 1.000000000000000000 ) ) 
 REPRESENTATION_ITEM ( '' )  );
#36388 = CARTESIAN_POINT ( 'NONE',  ( 21.21562500061451573, 3.027376345333611329, 5.243569643749999010 ) ) ;
#36389 = EDGE_CURVE ( 'NONE', #16272, #53042, #21673, .T. ) ;
#36390 = CARTESIAN_POINT ( 'NONE',  ( 18.74062500061451431, -3.027376345333610441, -5.243569643749999898 ) ) ;
#36391 = CARTESIAN_POINT ( 'NONE',  ( 6.009375000614519458, 0.000000000000000000, 5.243569643749999010 ) ) ;
#36392 = CARTESIAN_POINT ( 'NONE',  ( 18.03749999999999787, -2.886751345948125991, -5.000000000000000000 ) ) ;
#36393 = CARTESIAN_POINT ( 'NONE',  ( 14.73750000122903359, 4.330127018922191873, 2.499999999999999556 ) ) ;
#36394 = CARTESIAN_POINT ( 'NONE',  ( 10.49062500061451431, -3.027376345333614438, 5.243569643749998122 ) ) ;
#36395 = CARTESIAN_POINT ( 'NONE',  ( 12.70312500061451821, 0.000000000000000000, 5.243569643749999010 ) ) ;
#36396 = ADVANCED_FACE ( 'NONE', ( #48778 ), #27338, .T. ) ;
#36397 = CARTESIAN_POINT ( 'NONE',  ( 23.47500000122903430, -5.773502691896255534, -1.060575238724906372E-15 ) ) ;
#36398 = CARTESIAN_POINT ( 'NONE',  ( 21.68437500061451573, 4.541064518000418104, 2.621784821874999949 ) ) ;
#36399 = CARTESIAN_POINT ( 'NONE',  ( 21.72187500061451715, 3.027376345333611329, 5.243569643749999010 ) ) ;
#36400 = DIRECTION ( 'NONE',  ( 1.000000000000000000, 0.000000000000000000, 0.000000000000000000 ) ) ;
#36401 = EDGE_CURVE ( 'NONE', #52021, #72145, #32038, .T. ) ;
#36402 = CARTESIAN_POINT ( 'NONE',  ( 7.687500001229033764, -4.330127018922194537, 2.499999999999995559 ) ) ;
#36403 = CARTESIAN_POINT ( 'NONE',  ( 7.284375000614518036, 4.541064518000418104, 2.621784821874999949 ) ) ;
#36404 = CARTESIAN_POINT ( 'NONE',  ( 23.44687500061451502, 6.054752690667223547, 3.707466751127219781E-16 ) ) ;
#36405 = CARTESIAN_POINT ( 'NONE',  ( 4.465851277537014496, 2.248593419656078840, -4.736966354317482697 ) ) ;
#36406 = CARTESIAN_POINT ( 'NONE',  ( 20.65312500061451573, 4.541064518000418104, -2.621784821874998173 ) ) ;
#36407 = CARTESIAN_POINT ( 'NONE',  ( 24.42187500061451999, 3.027376345333611329, 5.243569643749999010 ) ) ;
#36408 = CARTESIAN_POINT ( 'NONE',  ( 3.756430356250000102, 19.05312499938548143, 30.00000000000000000 ) ) ;
#36409 = CARTESIAN_POINT ( 'NONE',  ( -1.071796769724488563, 13.45490381179670081, -26.00000000000000000 ) ) ;
#36410 = CARTESIAN_POINT ( 'NONE',  ( 6.121875000614517504, -6.054752690667223547, -1.112240025338166033E-15 ) ) ;
#36411 = CARTESIAN_POINT ( 'NONE',  ( 17.31562500061451715, -6.054752690667223547, -1.112240025338166033E-15 ) ) ;
#36412 = VERTEX_POINT ( 'NONE', #71675 ) ;
#36413 = CARTESIAN_POINT ( 'NONE',  ( 24.96562500061451573, -6.054752690667223547, -1.112240025338166033E-15 ) ) ;
#36414 = CARTESIAN_POINT ( 'NONE',  ( 4.171875000614517326, 3.027376345333611329, 5.243569643749999010 ) ) ;
#36415 = CARTESIAN_POINT ( 'NONE',  ( 4.735359408593126318, 1.605107869101089380, 4.812405942391664304 ) ) ;
#36416 = CARTESIAN_POINT ( 'NONE',  ( 3.649209776892925472, 3.418079578393367068, -3.833452633727637338 ) ) ;
#36417 = CARTESIAN_POINT ( 'NONE',  ( 15.86250000000000249, 2.886751345948129099, -4.999999999999998224 ) ) ;
#36418 = CARTESIAN_POINT ( 'NONE',  ( 19.86562500061451786, 3.027376345333611329, 5.243569643749999010 ) ) ;
#36419 = EDGE_LOOP ( 'NONE', ( #56768, #56059, #54663, #59792, #2924, #40001, #18599, #8250, #16173, #58490, #56632, #60723, #31758, #48119, #20017, #22201, #41966, #56243, #38388, #43553, #59313, #28852, #24655, #55331, #51390, #22482, #7611, #43678, #43298, #9363, #20144, #52377, #15341, #30729, #72615, #70768, #21366, #42555, #20784, #27674, #44070, #13564, #64491, #22102, #5273, #26273, #44812, #36692, #13872, #38154, #10027, #23149, #29442, #58047, #50320, #21150, #36982, #56966, #13896, #30928, #13565, #14465, #10658, #40573, #1716, #48622, #21110, #59521, #23873, #11180, #7260, #1356, #25536, #46115, #20741, #31967, #39838, #56919, #61768, #10756, #57319, #54154, #23289, #3169, #70405, #15116, #21529, #48521, #39122, #32573, #8986, #32342, #47161, #36785, #54787, #42209, #67567, #43212, #52901, #11913, #70316, #46424, #40880, #73080, #3831, #64035, #3765, #12090, #7835, #7455, #61583, #58798, #52337, #19901, #28394, #46986 ) ) ;
#36420 = CARTESIAN_POINT ( 'NONE',  ( 24.14999999999999858, 0.000000000000000000, 4.999999999999998224 ) ) ;
#36421 = EDGE_CURVE ( 'NONE', #54892, #26952, #16052, .T. ) ;
#36422 = CARTESIAN_POINT ( 'NONE',  ( 26.70937500061451431, 0.000000000000000000, 5.243569643749999010 ) ) ;
#36423 = EDGE_LOOP ( 'NONE', ( #38912, #32118, #66415, #52537 ) ) ;
#36424 = CARTESIAN_POINT ( 'NONE',  ( 2.996142289009378956, -4.002898508228532215, -3.387016711638999311 ) ) ;
#36425 = CARTESIAN_POINT ( 'NONE',  ( 12.59062500061451573, 6.054752690667223547, 3.707466751127219781E-16 ) ) ;
#36426 = CARTESIAN_POINT ( 'NONE',  ( 19.65000000000000213, 0.000000000000000000, 4.999999999999998224 ) ) ;
#36427 = CARTESIAN_POINT ( 'NONE',  ( 17.70937500061451786, -5.492252693125287522, -1.008910452111647106E-15 ) ) ;
#36428 = CARTESIAN_POINT ( 'NONE',  ( 28.79062500061451502, 6.054752690667223547, 3.707466751127219781E-16 ) ) ;
#36429 = CARTESIAN_POINT ( 'NONE',  ( 14.10000000122903252, -2.886751345948125991, -5.000000000000000000 ) ) ;
#36430 = CARTESIAN_POINT ( 'NONE',  ( 20.28750000000000142, -2.886751345948125991, -5.000000000000000000 ) ) ;
#36431 = CARTESIAN_POINT ( 'NONE',  ( 26.51249999999999929, -5.773502691896255534, -1.060575238724906372E-15 ) ) ;
#36432 = CARTESIAN_POINT ( 'NONE',  ( 29.43750000122903288, 6.123233995736764310E-16, -4.999999999999998224 ) ) ;
#36433 = CARTESIAN_POINT ( 'NONE',  ( 5.934375000614517504, 4.541064518000418104, 2.621784821874999949 ) ) ;
#36434 = CARTESIAN_POINT ( 'NONE',  ( 18.83437500061451431, 6.421520780324663323E-16, -5.243569643749999010 ) ) ;
#36435 = CARTESIAN_POINT ( 'NONE',  ( 19.91250000122903074, -4.330127018922190985, -2.500000000000001332 ) ) ;
#36436 = ORIENTED_EDGE ( 'NONE', *, *, #35732, .F. ) ;
#36437 = CARTESIAN_POINT ( 'NONE',  ( 28.49062500061451431, -3.027376345333614438, 5.243569643749998122 ) ) ;
#36438 = CARTESIAN_POINT ( 'NONE',  ( 29.03437500061451715, -4.541064518000419881, 2.621784821874995952 ) ) ;
#36439 = CARTESIAN_POINT ( 'NONE',  ( 3.496875000614518836, -3.027376345333610441, -5.243569643749999898 ) ) ;
#36440 = CARTESIAN_POINT ( 'NONE',  ( 17.13749999999999929, -2.886751345948125991, -5.000000000000000000 ) ) ;
#36441 = CARTESIAN_POINT ( 'NONE',  ( 13.67812500061451786, -4.541064518000419881, 2.621784821874995952 ) ) ;
#36442 = CARTESIAN_POINT ( 'NONE',  ( 0.000000000000000000, 20.00000000000000000, 30.00000000000000000 ) ) ;
#36443 = DIRECTION ( 'NONE',  ( -0.000000000000000000, -1.000000000000000000, -0.000000000000000000 ) ) ;
#36444 = LINE ( 'NONE', #2461, #5639 ) ;
#36445 = CARTESIAN_POINT ( 'NONE',  ( 18.11250000122903359, -4.330127018922190985, -2.500000000000001332 ) ) ;
#36446 = CARTESIAN_POINT ( 'NONE',  ( -1.626862140677534273E-15, 19.53124999877096357, 34.00000000000000000 ) ) ;
#36447 = CARTESIAN_POINT ( 'NONE',  ( 16.62187500061451573, 2.746126346562645981, -4.756430356249997438 ) ) ;
#36448 = CARTESIAN_POINT ( 'NONE',  ( 8.315625000614515372, -6.054752690667223547, -1.112240025338166033E-15 ) ) ;
#36449 = CARTESIAN_POINT ( 'NONE',  ( 23.22187500061451715, -6.054752690667223547, -1.112240025338166033E-15 ) ) ;
#36450 = CARTESIAN_POINT ( 'NONE',  ( -3.000416591977282496E-16, 18.84687500061452070, 25.09994784771203058 ) ) ;
#36451 = CARTESIAN_POINT ( 'NONE',  ( 25.02187500061451431, -6.054752690667223547, -1.112240025338166033E-15 ) ) ;
#36452 = CARTESIAN_POINT ( 'NONE',  ( 6.112499999999999822, 2.886751345948126879, 4.999999999999999112 ) ) ;
#36453 = CARTESIAN_POINT ( 'NONE',  ( -3.999999999999999112, 10.66250000122903430, 30.00000000000000000 ) ) ;
#36454 = CARTESIAN_POINT ( 'NONE',  ( 14.84062500061451750, 6.054752690667223547, 3.707466751127219781E-16 ) ) ;
#36455 = CARTESIAN_POINT ( 'NONE',  ( 3.900000001229034563, 5.773502691896255534, 3.535250795749688894E-16 ) ) ;
#36456 = CARTESIAN_POINT ( 'NONE',  ( 9.271875000614516082, -6.054752690667223547, -1.112240025338166033E-15 ) ) ;
#36457 = CARTESIAN_POINT ( 'NONE',  ( -1.487416814333745711E-14, 14.82500000122903572, 34.00000000000000000 ) ) ;
#36458 = EDGE_LOOP ( 'NONE', ( #48513, #11412, #39485, #43078 ) ) ;
#36459 = CARTESIAN_POINT ( 'NONE',  ( 13.00312500061451537, 4.541064518000418104, -2.621784821874998173 ) ) ;
#36460 = CARTESIAN_POINT ( 'NONE',  ( 3.999999999999998668, 12.27500000122903501, -32.30940107675850470 ) ) ;
#36461 = CARTESIAN_POINT ( 'NONE',  ( 24.82500000122902861, -5.773502691896255534, -1.060575238724906372E-15 ) ) ;
#36462 = CARTESIAN_POINT ( 'NONE',  ( 9.609375000614518214, 0.000000000000000000, 5.243569643749999010 ) ) ;
#36463 = CARTESIAN_POINT ( 'NONE',  ( 11.54062500061451857, -3.027376345333610441, -5.243569643749999898 ) ) ;
#36464 = CARTESIAN_POINT ( 'NONE',  ( 28.85625000122903216, -4.330127018922190985, -2.500000000000001332 ) ) ;
#36465 = CARTESIAN_POINT ( 'NONE',  ( 24.30937500061451573, 4.541064518000418104, -2.621784821874998173 ) ) ;
#36466 = CARTESIAN_POINT ( 'NONE',  ( 5.000000000000000000, 39.99999999999999289, 45.00000000000000000 ) ) ;
#36467 = LINE ( 'NONE', #64904, #58426 ) ;
#36468 = CARTESIAN_POINT ( 'NONE',  ( 2.121784821874999061, 14.75937500061451679, -33.67503911421598417 ) ) ;
#36469 = CARTESIAN_POINT ( 'NONE',  ( 16.77187500061451786, 3.027376345333611329, 5.243569643749999010 ) ) ;
#36470 = CARTESIAN_POINT ( 'NONE',  ( 18.52500000122903145, -5.773502691896255534, -1.060575238724906372E-15 ) ) ;
#36471 = CARTESIAN_POINT ( 'NONE',  ( 11.67187500061451821, 3.027376345333613106, -5.243569643749998122 ) ) ;
#36472 = CARTESIAN_POINT ( 'NONE',  ( -4.243569643749997233, 17.59062500061451928, -27.54997392385601174 ) ) ;
#36473 = CARTESIAN_POINT ( 'NONE',  ( 20.43750000122903643, 6.123233995736764310E-16, -4.999999999999998224 ) ) ;
#36474 = CARTESIAN_POINT ( 'NONE',  ( 12.32812500061451821, -4.541064518000419881, 2.621784821874995952 ) ) ;
#36475 = ORIENTED_EDGE ( 'NONE', *, *, #3065, .T. ) ;
#36476 = CARTESIAN_POINT ( 'NONE',  ( 16.72500000000000142, 6.123233995736764310E-16, -4.999999999999998224 ) ) ;
#36477 = CARTESIAN_POINT ( 'NONE',  ( 11.48437500061451644, -4.541064518000419881, 2.621784821874995952 ) ) ;
#36478 = CARTESIAN_POINT ( 'NONE',  ( 22.50000000000000000, -4.330127018922190985, -2.500000000000001332 ) ) ;
#36479 = CARTESIAN_POINT ( 'NONE',  ( 13.65000000122903323, -2.886751345948125991, -5.000000000000000000 ) ) ;
#36480 = CARTESIAN_POINT ( 'NONE',  ( 21.30000000122903359, -2.886751345948125991, -5.000000000000000000 ) ) ;
#36481 = CARTESIAN_POINT ( 'NONE',  ( 18.70312500061451644, -4.541064518000417216, -2.621784821875001281 ) ) ;
#36482 = EDGE_CURVE ( 'NONE', #10458, #19994, #16237, .T. ) ;
#36483 = CARTESIAN_POINT ( 'NONE',  ( 20.16562500061451146, 3.027376345333613106, -5.243569643749998122 ) ) ;
#36484 = CARTESIAN_POINT ( 'NONE',  ( 27.63750000122903216, 6.123233995736764310E-16, -4.999999999999998224 ) ) ;
#36485 = CARTESIAN_POINT ( 'NONE',  ( 26.13749999999999929, -2.886751345948125991, -5.000000000000000000 ) ) ;
#36486 = CARTESIAN_POINT ( 'NONE',  ( 0.000000000000000000, 20.00000000000000000, -30.00000000000000000 ) ) ;
#36487 = CARTESIAN_POINT ( 'NONE',  ( 28.98750000000000071, 5.773502691896255534, 3.535250795749688894E-16 ) ) ;
#36488 = CARTESIAN_POINT ( 'NONE',  ( 28.77187500061451431, 3.027376345333613106, -5.243569643749998122 ) ) ;
#36489 = CARTESIAN_POINT ( 'NONE',  ( 28.87499999999999645, 6.123233995736764310E-16, -4.999999999999998224 ) ) ;
#36490 = CARTESIAN_POINT ( 'NONE',  ( 4.243569643749999898, 13.78437500061451715, -30.00000000000000000 ) ) ;
#36491 = CARTESIAN_POINT ( 'NONE',  ( 3.375000001229033320, 2.886751345948129099, -4.999999999999998224 ) ) ;
#36492 = CARTESIAN_POINT ( 'NONE',  ( 6.937499999999999112, 5.773502691896255534, 3.535250795749688894E-16 ) ) ;
#36493 = CARTESIAN_POINT ( 'NONE',  ( 45.00000000000000000, 0.000000000000000000, 0.000000000000000000 ) ) ;
#36494 = CARTESIAN_POINT ( 'NONE',  ( 7.734375000614517326, 4.541064518000418104, 2.621784821874999949 ) ) ;
#36495 = CARTESIAN_POINT ( 'NONE',  ( 29.05312500061451431, -4.541064518000417216, -2.621784821875001281 ) ) ;
#36496 = CARTESIAN_POINT ( 'NONE',  ( 3.999999999999998668, 10.81250000000000178, 27.69059892324149530 ) ) ;
#36497 = CARTESIAN_POINT ( 'NONE',  ( -0.4074127065224517064, 10.00000000000000178, -36.00000000000000711 ) ) ;
#36498 = CYLINDRICAL_SURFACE ( 'NONE', #27718, 4.000000000000000000 ) ;
#36499 = CARTESIAN_POINT ( 'NONE',  ( 5.821875000614519458, 3.027376345333613106, -5.243569643749998122 ) ) ;
#36500 = CARTESIAN_POINT ( 'NONE',  ( 10.32187500061451679, 3.027376345333613106, -5.243569643749998122 ) ) ;
#36501 = CARTESIAN_POINT ( 'NONE',  ( 3.412500000000002309, 2.886751345948126879, 4.999999999999999112 ) ) ;
#36502 = EDGE_CURVE ( 'NONE', #12747, #47914, #49506, .T. ) ;
#36503 = CARTESIAN_POINT ( 'NONE',  ( 4.243569643749999010, 13.76562500061459460, 27.54997392385601174 ) ) ;
#36504 = CARTESIAN_POINT ( 'NONE',  ( 3.492397243767003889, 25.12859708874951892, 32.01989049841399293 ) ) ;
#36505 = CARTESIAN_POINT ( 'NONE',  ( 6.637500000000001066, -2.886751345948129988, 4.999999999999997335 ) ) ;
#36506 = CARTESIAN_POINT ( 'NONE',  ( 14.82187500061451502, 4.119189519843966529, 2.378215178124999607 ) ) ;
#36507 = CARTESIAN_POINT ( 'NONE',  ( 20.99062500061451431, -3.027376345333610441, -5.243569643749999898 ) ) ;
#36508 = CARTESIAN_POINT ( 'NONE',  ( 12.06562500061451537, 3.027376345333613106, -5.243569643749998122 ) ) ;
#36509 = CARTESIAN_POINT ( 'NONE',  ( 23.14687500061451786, -4.119189519843965641, -2.378215178125001383 ) ) ;
#36510 = CARTESIAN_POINT ( 'NONE',  ( 8.821875000614518569, -6.054752690667223547, -1.112240025338166033E-15 ) ) ;
#36511 = CARTESIAN_POINT ( 'NONE',  ( 27.03750000000000142, -2.886751345948125991, -5.000000000000000000 ) ) ;
#36512 = CARTESIAN_POINT ( 'NONE',  ( 21.71250000122903501, -4.330127018922190985, -2.500000000000001332 ) ) ;
#36513 = DIRECTION ( 'NONE',  ( -0.000000000000000000, -1.000000000000000000, -0.000000000000000000 ) ) ;
#36514 = CARTESIAN_POINT ( 'NONE',  ( 9.571875000614518569, 3.027376345333611329, 5.243569643749999010 ) ) ;
#36515 = CARTESIAN_POINT ( 'NONE',  ( 26.74687500061451573, -3.027376345333614438, 5.243569643749998122 ) ) ;
#36516 = CARTESIAN_POINT ( 'NONE',  ( 1.071796769724488119, 17.99509619066137134, -26.00000000000000000 ) ) ;
#36517 = ADVANCED_FACE ( 'NONE', ( #61664 ), #55047, .T. ) ;
#36518 = CARTESIAN_POINT ( 'NONE',  ( 1.626862140677534273E-15, 13.02500000122903323, -26.00000000000000355 ) ) ;
#36519 = CARTESIAN_POINT ( 'NONE',  ( 19.24687500061452283, -3.027376345333610441, -5.243569643749999898 ) ) ;
#36520 = CARTESIAN_POINT ( 'NONE',  ( 10.88437500061451679, 4.541064518000418104, 2.621784821874999949 ) ) ;
#36521 = CARTESIAN_POINT ( 'NONE',  ( -1.878215178125001827, 12.94062499938548427, 33.25316411605952283 ) ) ;
#36522 = CARTESIAN_POINT ( 'NONE',  ( 22.98749999999999716, -2.886751345948125991, -5.000000000000000000 ) ) ;
#36523 = CARTESIAN_POINT ( 'NONE',  ( 2.000000000000000444, 15.72499999999999964, 26.53589838486224650 ) ) ;
#36524 = CARTESIAN_POINT ( 'NONE',  ( 4.243569643749999898, 12.39687500061451608, -27.54997392385601529 ) ) ;
#36525 = CARTESIAN_POINT ( 'NONE',  ( 24.79687500061451999, 5.492252693125287522, 3.363034840372157021E-16 ) ) ;
#36526 = CARTESIAN_POINT ( 'NONE',  ( 14.91562500061451679, 3.027376345333611329, 5.243569643749999010 ) ) ;
#36527 = CARTESIAN_POINT ( 'NONE',  ( 4.949999999999999289, -4.330127018922190985, -2.500000000000001332 ) ) ;
#36528 = DIRECTION ( 'NONE',  ( -1.000000000000000000, -0.000000000000000000, -0.000000000000000000 ) ) ;
#36529 = CARTESIAN_POINT ( 'NONE',  ( 25.68750000000000355, -2.886751345948159742, -4.999999999999942268 ) ) ;
#36530 = CARTESIAN_POINT ( 'NONE',  ( 11.55000000000000071, 0.000000000000000000, 4.999999999999998224 ) ) ;
#36531 = CARTESIAN_POINT ( 'NONE',  ( -3.999999999999999556, 16.92500000122903359, 27.69059892324149530 ) ) ;
#36532 = CARTESIAN_POINT ( 'NONE',  ( 12.86250000122903359, 4.330127018922192761, -2.499999999999997780 ) ) ;
#36533 = CARTESIAN_POINT ( 'NONE',  ( 24.19687500061451857, -3.027376345333610441, -5.243569643749999898 ) ) ;
#36534 = CARTESIAN_POINT ( 'NONE',  ( 15.83437500061451608, 4.541064518000418104, 2.621784821874999949 ) ) ;
#36535 = CARTESIAN_POINT ( 'NONE',  ( 7.218750001229033764, -5.773502691896255534, -1.060575238724906372E-15 ) ) ;
#36536 = ORIENTED_EDGE ( 'NONE', *, *, #69202, .T. ) ;
#36537 = CARTESIAN_POINT ( 'NONE',  ( 19.79062500061451502, 6.054752690667223547, 3.707466751127219781E-16 ) ) ;
#36538 = CARTESIAN_POINT ( 'NONE',  ( 3.590625000614518836, 6.054752690667223547, 3.707466751127219781E-16 ) ) ;
#36539 = CARTESIAN_POINT ( 'NONE',  ( 17.55937500061451573, 4.541064518000418104, -2.621784821874998173 ) ) ;
#36540 = CARTESIAN_POINT ( 'NONE',  ( 28.50937500061451502, 0.000000000000000000, 5.243569643749999010 ) ) ;
#36541 = CARTESIAN_POINT ( 'NONE',  ( 5.765625000614519102, 3.027376345333613106, -5.243569643749998122 ) ) ;
#36542 = CARTESIAN_POINT ( 'NONE',  ( 21.29062500061451502, -3.027376345333614438, 5.243569643749998122 ) ) ;
#36543 = CARTESIAN_POINT ( 'NONE',  ( -3.000416591977282496E-16, 16.09062500061451573, 25.09994784771203058 ) ) ;
#36544 = CARTESIAN_POINT ( 'NONE',  ( 15.56250000122903465, 4.330127018922192761, -2.499999999999997780 ) ) ;
#36545 = CARTESIAN_POINT ( 'NONE',  ( 12.64687500061451786, 5.492252693125287522, 3.363034840372157021E-16 ) ) ;
#36546 = CARTESIAN_POINT ( 'NONE',  ( 6.365625000614518747, 3.027376345333611329, 5.243569643749999010 ) ) ;
#36547 = ADVANCED_FACE ( 'NONE', ( #21411 ), #43601, .F. ) ;
#36548 = CARTESIAN_POINT ( 'NONE',  ( 3.759375000614517681, 0.000000000000000000, 5.243569643749999010 ) ) ;
#36549 = CARTESIAN_POINT ( 'NONE',  ( 2.896875000614518747, -3.027376345333614438, 5.243569643749998122 ) ) ;
#36550 = CARTESIAN_POINT ( 'NONE',  ( 22.43437500061451573, 6.421520780324663323E-16, -5.243569643749999010 ) ) ;
#36551 = CARTESIAN_POINT ( 'NONE',  ( 15.40312500061451573, 0.000000000000000000, 5.243569643749999010 ) ) ;
#36552 = CARTESIAN_POINT ( 'NONE',  ( 25.42500000122903359, 2.886751345948129099, -4.999999999999998224 ) ) ;
#36553 = CARTESIAN_POINT ( 'NONE',  ( 24.25312500061451715, 4.541064518000418104, -2.621784821874998173 ) ) ;
#36554 = CARTESIAN_POINT ( 'NONE',  ( 19.20937500061451786, -4.541064518000417216, -2.621784821875001281 ) ) ;
#36555 = CARTESIAN_POINT ( 'NONE',  ( 14.99062500061451786, -3.027376345333614438, 5.243569643749998122 ) ) ;
#36556 = CARTESIAN_POINT ( 'NONE',  ( -2.121784821874996840, 15.43437500061451928, 33.67503911421598417 ) ) ;
#36557 = CARTESIAN_POINT ( 'NONE',  ( 19.26562500061451644, 3.027376345333613106, -5.243569643749998122 ) ) ;
#36558 = DIRECTION ( 'NONE',  ( 0.000000000000000000, 0.000000000000000000, 1.000000000000000000 ) ) ;
#36559 = ORIENTED_EDGE ( 'NONE', *, *, #29318, .F. ) ;
#36560 = EDGE_LOOP ( 'NONE', ( #41796, #65819, #19100, #41236 ) ) ;
#36561 = CARTESIAN_POINT ( 'NONE',  ( 22.53750000000000142, -2.886751345948125991, -5.000000000000000000 ) ) ;
#36562 = CARTESIAN_POINT ( 'NONE',  ( -4.243569643749999898, 19.82187500061451857, -32.45002607614398471 ) ) ;
#36563 = CARTESIAN_POINT ( 'NONE',  ( 14.98125000122903216, 6.123233995736764310E-16, -4.999999999999998224 ) ) ;
#36564 = CARTESIAN_POINT ( 'NONE',  ( 27.66562500061451146, -6.054752690667223547, -1.112240025338166033E-15 ) ) ;
#36565 = CARTESIAN_POINT ( 'NONE',  ( 7.603125000614517681, 4.541064518000418104, -2.621784821874998173 ) ) ;
#36566 = CARTESIAN_POINT ( 'NONE',  ( 19.80000000122903359, -2.886751345948129988, 4.999999999999997335 ) ) ;
#36567 = CARTESIAN_POINT ( 'NONE',  ( 24.92812500061451431, -4.541064518000419881, 2.621784821874995952 ) ) ;
#36568 = CARTESIAN_POINT ( 'NONE',  ( 25.61250000000000071, -5.773502691896255534, -1.060575238724906372E-15 ) ) ;
#36569 = CARTESIAN_POINT ( 'NONE',  ( 28.71562500061451573, 3.027376345333613106, -5.243569643749998122 ) ) ;
#36570 = CARTESIAN_POINT ( 'NONE',  ( 9.028125000614517504, 4.541064518000418104, 2.621784821874999949 ) ) ;
#36571 =( BOUNDED_CURVE ( )  B_SPLINE_CURVE ( 2, ( #50689, #40323, #17763, #34044, #5980, #28870, #33687 ),
 .UNSPECIFIED., .F., .F. ) 
 B_SPLINE_CURVE_WITH_KNOTS ( ( 3, 2, 2, 3 ),
 ( 0.9000000000000001332, 0.9027777777777779011, 0.9055555555555556690, 0.9083333333333334370 ),
 .UNSPECIFIED. ) 
 CURVE ( )  GEOMETRIC_REPRESENTATION_ITEM ( )  RATIONAL_B_SPLINE_CURVE ( ( 0.9999999999999946709, 0.8660254037844440367, 1.000000000000000000, 0.8660254037844387076, 1.000000000000000000, 0.8660254037844333785, 1.000000000000005329 ) ) 
 REPRESENTATION_ITEM ( '' )  );
#36572 = EDGE_LOOP ( 'NONE', ( #57851, #67697, #30874, #57160 ) ) ;
#36573 = CARTESIAN_POINT ( 'NONE',  ( 25.56562500061452070, 3.027376345333613106, -5.243569643749998122 ) ) ;
#36574 = CARTESIAN_POINT ( 'NONE',  ( 4.415625000614518569, 3.027376345333613106, -5.243569643749998122 ) ) ;
#36575 = CARTESIAN_POINT ( 'NONE',  ( 14.89687500061451786, 5.492252693125287522, 3.363034840372157021E-16 ) ) ;
#36576 = CARTESIAN_POINT ( 'NONE',  ( 4.078125000614517326, 4.541064518000418104, 2.621784821874999949 ) ) ;
#36577 = CARTESIAN_POINT ( 'NONE',  ( -3.999999999999997335, 13.73749999999999893, -27.69059892324149530 ) ) ;
#36578 = CARTESIAN_POINT ( 'NONE',  ( 12.90000000000000213, 0.000000000000000000, 4.999999999999998224 ) ) ;
#36579 = CARTESIAN_POINT ( 'NONE',  ( 13.95937500061451786, 4.541064518000418104, -2.621784821874998173 ) ) ;
#36580 = CARTESIAN_POINT ( 'NONE',  ( 9.787500001229036073, 4.330127018922191873, 2.499999999999999556 ) ) ;
#36581 = CARTESIAN_POINT ( 'NONE',  ( 16.24687500061451573, 6.054752690667223547, 3.707466751127219781E-16 ) ) ;
#36582 = CARTESIAN_POINT ( 'NONE',  ( 15.90000000000000036, 4.330127018922192761, -2.499999999999997780 ) ) ;
#36583 = CARTESIAN_POINT ( 'NONE',  ( 8.071875000614518569, 3.027376345333613106, -5.243569643749998122 ) ) ;
#36584 = CARTESIAN_POINT ( 'NONE',  ( 4.243569643749999010, 12.86562500061451608, -32.45002607614398471 ) ) ;
#36585 = CARTESIAN_POINT ( 'NONE',  ( -5.810221930991193690E-16, 11.78749999999999964, -34.00000000000000000 ) ) ;
#36586 = CARTESIAN_POINT ( 'NONE',  ( 11.74687500061451573, 6.054752690667223547, 3.707466751127219781E-16 ) ) ;
#36587 = FACE_OUTER_BOUND ( 'NONE', #8564, .T. ) ;
#36588 = CARTESIAN_POINT ( 'NONE',  ( 21.70312500061451644, 0.000000000000000000, 5.243569643749999010 ) ) ;
#36589 = LINE ( 'NONE', #20684, #55757 ) ;
#36590 = CARTESIAN_POINT ( 'NONE',  ( 4.000000000000000000, 20.54374999877096641, 30.00000000000000000 ) ) ;
#36591 = CARTESIAN_POINT ( 'NONE',  ( 26.52187500061451431, 3.027376345333613106, -5.243569643749998122 ) ) ;
#36592 = CARTESIAN_POINT ( 'NONE',  ( 28.73437500061451644, 6.421520780324663323E-16, -5.243569643749999010 ) ) ;
#36593 = CARTESIAN_POINT ( 'NONE',  ( 3.928125000614516527, 6.421520780324663323E-16, -5.243569643749999010 ) ) ;
#36594 = CARTESIAN_POINT ( 'NONE',  ( 22.32187500061451502, 5.824947211148865298E-16, -4.756430356249998326 ) ) ;
#36595 = CARTESIAN_POINT ( 'NONE',  ( 17.74687500061451928, -3.027376345333614438, 5.243569643749998122 ) ) ;
#36596 = CARTESIAN_POINT ( 'NONE',  ( 8.596875000614515372, 0.000000000000000000, 4.756430356249998326 ) ) ;
#36597 = CARTESIAN_POINT ( 'NONE',  ( 28.72500000122903074, 2.886751345948126879, 4.999999999999999112 ) ) ;
#36598 = CARTESIAN_POINT ( 'NONE',  ( 6.609375000614519102, -4.541064518000417216, -2.621784821875001281 ) ) ;
#36599 = CARTESIAN_POINT ( 'NONE',  ( 17.33437500061451431, -4.541064518000419881, 2.621784821874995952 ) ) ;
#36600 = CARTESIAN_POINT ( 'NONE',  ( -4.000059620491343892, 24.99998410120267778, 29.73716349952571392 ) ) ;
#36601 = CARTESIAN_POINT ( 'NONE',  ( 25.61250000000000071, -5.773502691896255534, -1.060575238724906372E-15 ) ) ;
#36602 = CARTESIAN_POINT ( 'NONE',  ( 27.94687500061451502, 6.054752690667223547, 3.707466751127219781E-16 ) ) ;
#36603 = CARTESIAN_POINT ( 'NONE',  ( -1.878215178125001827, 13.05312499938548321, 33.25316411605952283 ) ) ;
#36604 = CARTESIAN_POINT ( 'NONE',  ( 14.13750000122903394, 6.123233995736764310E-16, -4.999999999999998224 ) ) ;
#36605 = VERTEX_POINT ( 'NONE', #26241 ) ;
#36606 = CARTESIAN_POINT ( 'NONE',  ( 7.837499999999999467, 5.773502691896255534, 3.535250795749688894E-16 ) ) ;
#36607 = CARTESIAN_POINT ( 'NONE',  ( 9.909375000614517148, 2.746126346562643317, 4.756430356249998326 ) ) ;
#36608 = CARTESIAN_POINT ( 'NONE',  ( 22.49062500061451431, 6.054752690667223547, 3.707466751127219781E-16 ) ) ;
#36609 = CARTESIAN_POINT ( 'NONE',  ( 10.80000000000000071, -4.330127018922190985, -2.500000000000001332 ) ) ;
#36610 = CARTESIAN_POINT ( 'NONE',  ( 7.500000001229034652, 5.773502691896255534, 3.535250795749688894E-16 ) ) ;
#36611 = CARTESIAN_POINT ( 'NONE',  ( 7.040625000614517681, -3.027376345333610441, -5.243569643749999898 ) ) ;
#36612 = CARTESIAN_POINT ( 'NONE',  ( 22.08749999999999858, -2.886751345948125991, -5.000000000000000000 ) ) ;
#36613 = CARTESIAN_POINT ( 'NONE',  ( 18.17812500061451786, -4.541064518000419881, 2.621784821874995952 ) ) ;
#36614 = CARTESIAN_POINT ( 'NONE',  ( 1.980717643099229042, -4.701347860447535609, -1.980717643099229042 ) ) ;
#36615 = CARTESIAN_POINT ( 'NONE',  ( 26.47500000122903074, 2.886751345948126879, 4.999999999999999112 ) ) ;
#36616 = CARTESIAN_POINT ( 'NONE',  ( 1.626862140677534273E-15, 10.21250000000000036, -26.00000000000000355 ) ) ;
#36617 = CARTESIAN_POINT ( 'NONE',  ( 5.137500000000000178, 5.773502691896255534, 3.535250795749688894E-16 ) ) ;
#36618 = ORIENTED_EDGE ( 'NONE', *, *, #16676, .F. ) ;
#36619 = CARTESIAN_POINT ( 'NONE',  ( 20.16562500061451146, 3.027376345333613106, -5.243569643749998122 ) ) ;
#36620 = CARTESIAN_POINT ( 'NONE',  ( 27.62812500061451360, -4.541064518000419881, 2.621784821874995952 ) ) ;
#36621 = CARTESIAN_POINT ( 'NONE',  ( 24.83437500061451431, 4.541064518000418104, 2.621784821874999949 ) ) ;
#36622 = CARTESIAN_POINT ( 'NONE',  ( 8.212500000000000355, 2.886751345948129099, -4.999999999999998224 ) ) ;
#36623 = CARTESIAN_POINT ( 'NONE',  ( 12.70312500061451821, 0.000000000000000000, 5.243569643749999010 ) ) ;
#36624 = CARTESIAN_POINT ( 'NONE',  ( 28.82812500061451644, 4.541064518000418104, 2.621784821874999949 ) ) ;
#36625 = CARTESIAN_POINT ( 'NONE',  ( 8.690625000614515372, -3.027376345333614438, 5.243569643749998122 ) ) ;
#36626 = CARTESIAN_POINT ( 'NONE',  ( 2.994107990571896138, -4.004412234122908920, 3.194628461336531888 ) ) ;
#36627 = CARTESIAN_POINT ( 'NONE',  ( -2.121784821874996840, 11.83437500061451786, 33.67503911421598417 ) ) ;
#36628 = CARTESIAN_POINT ( 'NONE',  ( 23.96250000122903145, -4.330127018922190985, -2.500000000000001332 ) ) ;
#36629 = CARTESIAN_POINT ( 'NONE',  ( 18.94687500061451857, 5.492252693125287522, 3.363034840372157021E-16 ) ) ;
#36630 = CARTESIAN_POINT ( 'NONE',  ( 13.45312500061451466, 4.541064518000418104, -2.621784821874998173 ) ) ;
#36631 = CARTESIAN_POINT ( 'NONE',  ( 10.54687500061451644, -3.027376345333614438, 5.243569643749998122 ) ) ;
#36632 = CARTESIAN_POINT ( 'NONE',  ( 10.58437500061451964, -4.541064518000419881, 2.621784821874995952 ) ) ;
#36633 = CARTESIAN_POINT ( 'NONE',  ( 17.70937500061451431, 0.000000000000000000, 5.243569643749999010 ) ) ;
#36634 = ORIENTED_EDGE ( 'NONE', *, *, #29767, .T. ) ;
#36635 = CARTESIAN_POINT ( 'NONE',  ( -1.393485112971533768, 9.904374691868486735, 35.83932025239862185 ) ) ;
#36636 = CARTESIAN_POINT ( 'NONE',  ( 21.10312500061451502, 4.541064518000418104, -2.621784821874998173 ) ) ;
#36637 = CARTESIAN_POINT ( 'NONE',  ( 17.40937500061451715, -4.541064518000417216, -2.621784821875001281 ) ) ;
#36638 = CARTESIAN_POINT ( 'NONE',  ( 21.02812500061451573, 6.421520780324663323E-16, -5.243569643749999010 ) ) ;
#36639 = CARTESIAN_POINT ( 'NONE',  ( -3.999999999999999556, 14.56250000000000000, 27.69059892324149530 ) ) ;
#36640 = CARTESIAN_POINT ( 'NONE',  ( 26.57812500061451644, 4.541064518000418104, 2.621784821874999949 ) ) ;
#36641 = CARTESIAN_POINT ( 'NONE',  ( 7.237500001229035362, -4.330127018922194537, 2.499999999999995559 ) ) ;
#36642 = EDGE_LOOP ( 'NONE', ( #51254, #31155, #33720, #34150 ) ) ;
#36643 = CARTESIAN_POINT ( 'NONE',  ( 3.750000001229034652, -2.886751345948125991, -5.000000000000000000 ) ) ;
#36644 = CARTESIAN_POINT ( 'NONE',  ( 1.999999999999998668, 17.60000000000000142, -33.46410161513775705 ) ) ;
#36645 = CARTESIAN_POINT ( 'NONE',  ( 24.52500000122903145, 2.886751345948129099, -4.999999999999998224 ) ) ;
#36646 = CARTESIAN_POINT ( 'NONE',  ( -3.999999999999999556, 20.28124999877096712, 27.69059892324149175 ) ) ;
#36647 = CARTESIAN_POINT ( 'NONE',  ( 7.659375000614518036, 4.541064518000418104, -2.621784821874998173 ) ) ;
#36648 = CARTESIAN_POINT ( 'NONE',  ( 20.38125000122903430, 6.123233995736764310E-16, -4.999999999999998224 ) ) ;
#36649 = CARTESIAN_POINT ( 'NONE',  ( 14.91562500061451679, 3.027376345333611329, 5.243569643749999010 ) ) ;
#36650 = CARTESIAN_POINT ( 'NONE',  ( 8.896875000614517859, -3.027376345333610441, -5.243569643749999898 ) ) ;
#36651 = EDGE_CURVE ( 'NONE', #69502, #35463, #41511, .T. ) ;
#36652 = CARTESIAN_POINT ( 'NONE',  ( 26.51250000122903216, 0.000000000000000000, 4.999999999999998224 ) ) ;
#36653 = CARTESIAN_POINT ( 'NONE',  ( 16.35937500061451644, 0.000000000000000000, 5.243569643749999010 ) ) ;
#36654 = CARTESIAN_POINT ( 'NONE',  ( 4.021875000614516082, 3.027376345333613106, -5.243569643749998122 ) ) ;
#36655 = LINE ( 'NONE', #13024, #17923 ) ;
#36656 = CARTESIAN_POINT ( 'NONE',  ( 6.328125000614515550, 4.541064518000418104, 2.621784821874999949 ) ) ;
#36657 = CARTESIAN_POINT ( 'NONE',  ( 14.35312500061451679, 4.541064518000418104, -2.621784821874998173 ) ) ;
#36658 = ADVANCED_FACE ( 'NONE', ( #32873 ), #72763, .F. ) ;
#36659 = VERTEX_POINT ( 'NONE', #4805 ) ;
#36660 = CARTESIAN_POINT ( 'NONE',  ( 12.36562500061451608, -6.054752690667223547, -1.112240025338166033E-15 ) ) ;
#36661 = CARTESIAN_POINT ( 'NONE',  ( 4.762500001229033941, 4.330127018922192761, -2.499999999999997780 ) ) ;
#36662 = CARTESIAN_POINT ( 'NONE',  ( 9.965625000614517504, 3.027376345333611329, 5.243569643749999010 ) ) ;
#36663 = CARTESIAN_POINT ( 'NONE',  ( 21.00937500061451857, -4.119189519843965641, -2.378215178125001383 ) ) ;
#36664 = CARTESIAN_POINT ( 'NONE',  ( 9.937500000000001776, -2.886751345948125991, -5.000000000000000000 ) ) ;
#36665 = CARTESIAN_POINT ( 'NONE',  ( 7.650000001229034119, -2.886751345948129988, 4.999999999999997335 ) ) ;
#36666 = CARTESIAN_POINT ( 'NONE',  ( 21.18749999999999645, -2.886751345948125991, -5.000000000000000000 ) ) ;
#36667 = CARTESIAN_POINT ( 'NONE',  ( 14.33437500061451786, 6.421520780324663323E-16, -5.243569643749999010 ) ) ;
#36668 = CARTESIAN_POINT ( 'NONE',  ( 15.48750000122903359, 6.123233995736764310E-16, -4.999999999999998224 ) ) ;
#36669 = CARTESIAN_POINT ( 'NONE',  ( 22.98749999999999716, -2.886751345948125991, -5.000000000000000000 ) ) ;
#36670 = CARTESIAN_POINT ( 'NONE',  ( 2.121784821874999061, 18.75312500061451715, -33.67503911421598417 ) ) ;
#36671 = CARTESIAN_POINT ( 'NONE',  ( 9.262499999999997513, 2.886751345948182834, 4.999999999999902300 ) ) ;
#36672 = CARTESIAN_POINT ( 'NONE',  ( 45.00000000000000000, 0.000000000000000000, 4.999999999999998224 ) ) ;
#36673 = DIRECTION ( 'NONE',  ( -0.000000000000000000, -1.000000000000000000, -0.000000000000000000 ) ) ;
#36674 = CARTESIAN_POINT ( 'NONE',  ( 1.071796769724505438, 10.97990381179670116, -33.99999999999999289 ) ) ;
#36675 = CARTESIAN_POINT ( 'NONE',  ( 1.071796769724489895, 14.57990381179669903, 26.00000000000000355 ) ) ;
#36676 = CARTESIAN_POINT ( 'NONE',  ( 15.15937500061451715, -4.541064518000417216, -2.621784821875001281 ) ) ;
#36677 = CARTESIAN_POINT ( 'NONE',  ( 27.97500000000000142, 6.123233995736764310E-16, -4.999999999999998224 ) ) ;
#36678 = CARTESIAN_POINT ( 'NONE',  ( 12.44062500061451537, -3.027376345333610441, -5.243569643749999898 ) ) ;
#36679 = CARTESIAN_POINT ( 'NONE',  ( 28.50937500061451857, -5.492252693125287522, -1.008910452111647106E-15 ) ) ;
#36680 = CARTESIAN_POINT ( 'NONE',  ( 24.83437500061451431, 4.541064518000418104, 2.621784821874999949 ) ) ;
#36681 = CARTESIAN_POINT ( 'NONE',  ( 14.85937500061451999, 2.746126346562643317, 4.756430356249998326 ) ) ;
#36682 = CARTESIAN_POINT ( 'NONE',  ( 9.140625000614518214, -3.027376345333614438, 5.243569643749998122 ) ) ;
#36683 = CARTESIAN_POINT ( 'NONE',  ( 14.55937500061451573, 0.000000000000000000, 5.243569643749999010 ) ) ;
#36684 = ORIENTED_EDGE ( 'NONE', *, *, #21207, .F. ) ;
#36685 = CARTESIAN_POINT ( 'NONE',  ( 24.75937500061451502, 4.541064518000418104, -2.621784821874998173 ) ) ;
#36686 = CARTESIAN_POINT ( 'NONE',  ( 26.91562500061451146, 3.027376345333613106, -5.243569643749998122 ) ) ;
#36687 = CARTESIAN_POINT ( 'NONE',  ( 27.29062500061451502, -3.027376345333610441, -5.243569643749999898 ) ) ;
#36688 = CARTESIAN_POINT ( 'NONE',  ( 7.612500000000000711, -5.773502691896255534, -1.060575238724906372E-15 ) ) ;
#36689 = CARTESIAN_POINT ( 'NONE',  ( 17.96250000122903501, 0.000000000000000000, 4.999999999999998224 ) ) ;
#36690 = DIRECTION ( 'NONE',  ( 0.000000000000000000, 6.195440985631456550E-17, 1.000000000000000000 ) ) ;
#36691 = CARTESIAN_POINT ( 'NONE',  ( 7.471875000614514484, 5.824947211148865298E-16, -4.756430356249998326 ) ) ;
#36692 = ORIENTED_EDGE ( 'NONE', *, *, #28846, .T. ) ;
#36693 = CARTESIAN_POINT ( 'NONE',  ( 14.06250000000000000, 2.886751345948129099, -4.999999999999998224 ) ) ;
#36694 = CARTESIAN_POINT ( 'NONE',  ( 19.31250000000000000, -5.773502691896255534, -1.060575238724906372E-15 ) ) ;
#36695 = CARTESIAN_POINT ( 'NONE',  ( 13.11562500061451786, 3.027376345333611329, 5.243569643749999010 ) ) ;
#36696 = EDGE_LOOP ( 'NONE', ( #52549, #14882, #57493, #45390 ) ) ;
#36697 = CARTESIAN_POINT ( 'NONE',  ( 28.42499999999999716, 6.123233995736764310E-16, -4.999999999999998224 ) ) ;
#36698 = CARTESIAN_POINT ( 'NONE',  ( -4.243569643749999898, 18.05937500061451928, -30.00000000000000000 ) ) ;
#36699 = CARTESIAN_POINT ( 'NONE',  ( 6.178125000614518747, 6.421520780324663323E-16, -5.243569643749999010 ) ) ;
#36700 = CARTESIAN_POINT ( 'NONE',  ( 3.756430356250000102, 12.64062499938548356, 30.00000000000000000 ) ) ;
#36701 = CARTESIAN_POINT ( 'NONE',  ( 11.13750000000000284, -2.886751345948129988, 4.999999999999997335 ) ) ;
#36702 = CARTESIAN_POINT ( 'NONE',  ( 28.47187500061451715, -4.119189519843968306, 2.378215178124996054 ) ) ;
#36703 = ORIENTED_EDGE ( 'NONE', *, *, #1145, .T. ) ;
#36704 = CARTESIAN_POINT ( 'NONE',  ( -2.121784821874999949, 15.22812500061451679, 26.32496088578401938 ) ) ;
#36705 = CARTESIAN_POINT ( 'NONE',  ( 25.52812500061451573, 6.421520780324663323E-16, -5.243569643749999010 ) ) ;
#36706 = CARTESIAN_POINT ( 'NONE',  ( 8.362500000000002487, 2.886751345948126879, 4.999999999999999112 ) ) ;
#36707 = CARTESIAN_POINT ( 'NONE',  ( -3.756430356249999214, 18.22812499938548214, 27.83122392262697531 ) ) ;
#36708 = CARTESIAN_POINT ( 'NONE',  ( 22.95937500061451431, 4.541064518000418104, -2.621784821874998173 ) ) ;
#36709 = CARTESIAN_POINT ( 'NONE',  ( 19.04062500061451146, -3.027376345333614438, 5.243569643749998122 ) ) ;
#36710 = CARTESIAN_POINT ( 'NONE',  ( 4.243569643749999010, 14.21562500061459389, -32.45002607614398471 ) ) ;
#36711 = CARTESIAN_POINT ( 'NONE',  ( 24.11250000122903359, 4.330127018922192761, -2.499999999999997780 ) ) ;
#36712 = CARTESIAN_POINT ( 'NONE',  ( 6.065625000614516260, -6.054752690667223547, -1.112240025338166033E-15 ) ) ;
#36713 = CARTESIAN_POINT ( 'NONE',  ( 27.23437500061451644, -4.119189519843968306, 2.378215178124996054 ) ) ;
#36714 = CARTESIAN_POINT ( 'NONE',  ( 22.56562500061451715, 3.027376345333611329, 5.243569643749999010 ) ) ;
#36715 = CARTESIAN_POINT ( 'NONE',  ( 10.35937500061451644, 4.119189519843966529, -2.378215178124998275 ) ) ;
#36716 = CARTESIAN_POINT ( 'NONE',  ( -3.756430356250000102, 16.01562499938548356, 30.00000000000000000 ) ) ;
#36717 =( BOUNDED_CURVE ( )  B_SPLINE_CURVE ( 2, ( #35921, #58445, #30392, #52921, #69912, #37391, #10414, #3424, #4522 ),
 .UNSPECIFIED., .F., .F. ) 
 B_SPLINE_CURVE_WITH_KNOTS ( ( 3, 2, 2, 2, 3 ),
 ( 0.2282608695652174058, 0.2318840579710144956, 0.2391304347826087029, 0.2463768115942029102, 0.2500000000000000000 ),
 .UNSPECIFIED. ) 
 CURVE ( )  GEOMETRIC_REPRESENTATION_ITEM ( )  RATIONAL_B_SPLINE_CURVE ( ( 0.9330127018922194093, 0.9330127018922196314, 1.000000000000000000, 0.8660254037844387076, 1.000000000000000000, 0.8660254037844387076, 1.000000000000000000, 0.9330127018922196314, 0.9330127018922194093 ) ) 
 REPRESENTATION_ITEM ( '' )  );
#36718 = CARTESIAN_POINT ( 'NONE',  ( 16.13437500061451502, 6.421520780324663323E-16, -5.243569643749999010 ) ) ;
#36719 = CARTESIAN_POINT ( 'NONE',  ( 24.34687500061451715, 6.054752690667223547, 3.707466751127219781E-16 ) ) ;
#36720 = CARTESIAN_POINT ( 'NONE',  ( 2.121784821875001281, 13.25937500061451857, 33.67503911421598417 ) ) ;
#36721 = CARTESIAN_POINT ( 'NONE',  ( 4.753125000614515372, -4.541064518000417216, -2.621784821875001281 ) ) ;
#36722 = CARTESIAN_POINT ( 'NONE',  ( 29.54062500061451502, -3.027376345333610441, -5.243569643749999898 ) ) ;
#36723 = CARTESIAN_POINT ( 'NONE',  ( 2.934375000614518392, -4.541064518000419881, 2.621784821874995952 ) ) ;
#36724 = CARTESIAN_POINT ( 'NONE',  ( 4.292152659130343828, 3.669920861174119864, 3.643510608689493058 ) ) ;
#36725 = CARTESIAN_POINT ( 'NONE',  ( 3.909375000614518481, -4.541064518000417216, -2.621784821875001281 ) ) ;
#36726 = CARTESIAN_POINT ( 'NONE',  ( 2.803125000614518747, 0.000000000000000000, 5.243569643749999010 ) ) ;
#36727 = CARTESIAN_POINT ( 'NONE',  ( 7.471875000614519813, -6.054752690667223547, -1.112240025338166033E-15 ) ) ;
#36728 = CARTESIAN_POINT ( 'NONE',  ( 14.40000000122903323, -2.886751345948129988, 4.999999999999997335 ) ) ;
#36729 = CARTESIAN_POINT ( 'NONE',  ( 3.271875000614519635, 3.027376345333611329, 5.243569643749999010 ) ) ;
#36730 = CARTESIAN_POINT ( 'NONE',  ( 10.87500000122903288, -5.773502691896255534, -1.060575238724906372E-15 ) ) ;
#36731 = CARTESIAN_POINT ( 'NONE',  ( 5.315625000614516260, 3.027376345333613106, -5.243569643749998122 ) ) ;
#36732 = CARTESIAN_POINT ( 'NONE',  ( 1.999999999999997335, 13.71874999877096535, 33.46410161513775705 ) ) ;
#36733 = CARTESIAN_POINT ( 'NONE',  ( 20.64375000122903359, -2.886751345948129988, 4.999999999999997335 ) ) ;
#36734 = VECTOR ( 'NONE', #38049, 1000.000000000000227 ) ;
#36735 = CARTESIAN_POINT ( 'NONE',  ( 15.45937500061451608, 0.000000000000000000, 5.243569643749999010 ) ) ;
#36736 = DIRECTION ( 'NONE',  ( -1.000000000000000000, -0.000000000000000000, -0.000000000000000000 ) ) ;
#36737 = ORIENTED_EDGE ( 'NONE', *, *, #45774, .T. ) ;
#36738 = CARTESIAN_POINT ( 'NONE',  ( 23.39062500061451289, 6.054752690667223547, 3.707466751127219781E-16 ) ) ;
#36739 = CARTESIAN_POINT ( 'NONE',  ( 7.715625000614515727, 3.027376345333611329, 5.243569643749999010 ) ) ;
#36740 = CARTESIAN_POINT ( 'NONE',  ( 25.65937500061451715, 4.541064518000418104, -2.621784821874998173 ) ) ;
#36741 = CARTESIAN_POINT ( 'NONE',  ( 6.478125000614516793, -4.541064518000419881, 2.621784821874995952 ) ) ;
#36742 = CARTESIAN_POINT ( 'NONE',  ( -4.243569643749999898, 19.80312500061451786, 30.00000000000000000 ) ) ;
#36743 = CARTESIAN_POINT ( 'NONE',  ( 7.350000001229033408, -2.886751345948125991, -5.000000000000000000 ) ) ;
#36744 = CARTESIAN_POINT ( 'NONE',  ( 24.36562500061451786, 3.027376345333611329, 5.243569643749999010 ) ) ;
#36745 = EDGE_CURVE ( 'NONE', #17299, #22971, #59404, .T. ) ;
#36746 = CARTESIAN_POINT ( 'NONE',  ( -4.243569643749999898, 9.865625000614517859, -32.45002607614398471 ) ) ;
#36747 = CARTESIAN_POINT ( 'NONE',  ( 11.21250000122903501, 0.000000000000000000, 4.999999999999998224 ) ) ;
#36748 = CARTESIAN_POINT ( 'NONE',  ( 20.76562500061451644, 3.027376345333611329, 5.243569643749999010 ) ) ;
#36749 = CARTESIAN_POINT ( 'NONE',  ( 17.46562500061451217, 3.027376345333613106, -5.243569643749998122 ) ) ;
#36750 = CARTESIAN_POINT ( 'NONE',  ( 28.28437500061451715, 5.824947211148865298E-16, -4.756430356249998326 ) ) ;
#36751 = CARTESIAN_POINT ( 'NONE',  ( 17.47499999999999787, -4.330127018922194537, 2.499999999999995559 ) ) ;
#36752 = CARTESIAN_POINT ( 'NONE',  ( 13.20000000122903394, -2.886751345948125991, -5.000000000000000000 ) ) ;
#36753 = CARTESIAN_POINT ( 'NONE',  ( 9.703125000614514661, -4.541064518000417216, -2.621784821875001281 ) ) ;
#36754 = AXIS2_PLACEMENT_3D ( 'NONE', #61185, #15015, #4324 ) ;
#36755 = CARTESIAN_POINT ( 'NONE',  ( 12.59062500061451573, 6.054752690667223547, 3.707466751127219781E-16 ) ) ;
#36756 = CARTESIAN_POINT ( 'NONE',  ( 22.87500000122903288, 2.886751345948126879, 4.999999999999999112 ) ) ;
#36757 = CARTESIAN_POINT ( 'NONE',  ( 21.79687500061451644, -3.027376345333614438, 5.243569643749998122 ) ) ;
#36758 = CARTESIAN_POINT ( 'NONE',  ( 21.00937500061451857, -4.541064518000417216, -2.621784821875001281 ) ) ;
#36759 = CARTESIAN_POINT ( 'NONE',  ( -4.000000000000000000, 18.57500000000000284, 30.00000000000000000 ) ) ;
#36760 = CARTESIAN_POINT ( 'NONE',  ( 7.350000001229033408, -2.886751345948125991, -5.000000000000000000 ) ) ;
#36761 =( BOUNDED_CURVE ( )  B_SPLINE_CURVE ( 2, ( #13057, #30785, #70312, #18951, #2351, #63309, #48147, #35595, #41510 ),
 .UNSPECIFIED., .F., .F. ) 
 B_SPLINE_CURVE_WITH_KNOTS ( ( 3, 2, 2, 2, 3 ),
 ( 0.6630434782608696231, 0.6666666666666666297, 0.6739130434782608647, 0.6811594202898550998, 0.6847826086956522174 ),
 .UNSPECIFIED. ) 
 CURVE ( )  GEOMETRIC_REPRESENTATION_ITEM ( )  RATIONAL_B_SPLINE_CURVE ( ( 0.9330127018922192983, 0.9330127018922202975, 1.000000000000000000, 0.8660254037844387076, 1.000000000000000000, 0.8660254037844387076, 1.000000000000000000, 0.9330127018922182991, 0.9330127018922192983 ) ) 
 REPRESENTATION_ITEM ( '' )  );
#36762 = CARTESIAN_POINT ( 'NONE',  ( 5.296875000614518214, -3.027376345333610441, -5.243569643749999898 ) ) ;
#36763 = CARTESIAN_POINT ( 'NONE',  ( 23.67187500061451999, -6.054752690667223547, -1.112240025338166033E-15 ) ) ;
#36764 =( BOUNDED_CURVE ( )  B_SPLINE_CURVE ( 2, ( #60050, #25346, #8357, #47520, #9461, #3928, #41615 ),
 .UNSPECIFIED., .F., .F. ) 
 B_SPLINE_CURVE_WITH_KNOTS ( ( 3, 2, 2, 3 ),
 ( 0.1416666666666666352, 0.1444444444444444031, 0.1472222222222221710, 0.1499999999999999389 ),
 .UNSPECIFIED. ) 
 CURVE ( )  GEOMETRIC_REPRESENTATION_ITEM ( )  RATIONAL_B_SPLINE_CURVE ( ( 1.000000000000001332, 0.8660254037844373753, 1.000000000000000000, 0.8660254037844387076, 1.000000000000000000, 0.8660254037844413721, 0.9999999999999973355 ) ) 
 REPRESENTATION_ITEM ( '' )  );
#36765 = CARTESIAN_POINT ( 'NONE',  ( -4.000000000000000888, 12.76250000000000107, 32.30940107675850470 ) ) ;
#36766 = CARTESIAN_POINT ( 'NONE',  ( 17.80312500061451786, -4.541064518000417216, -2.621784821875001281 ) ) ;
#36767 = CARTESIAN_POINT ( 'NONE',  ( 24.45937500061451786, 0.000000000000000000, 5.243569643749999010 ) ) ;
#36768 = CARTESIAN_POINT ( 'NONE',  ( 2.655984681222220721E-16, 19.16562499938548214, 25.66244784525396483 ) ) ;
#36769 = CARTESIAN_POINT ( 'NONE',  ( 30.00000000000000000, 0.000000000000000000, 4.999999999999998224 ) ) ;
#36770 = CARTESIAN_POINT ( 'NONE',  ( 30.00000000000000000, 0.000000000000000000, 0.000000000000000000 ) ) ;
#36771 = CARTESIAN_POINT ( 'NONE',  ( 5.034375000614519813, 4.541064518000418104, 2.621784821874999949 ) ) ;
#36772 = CARTESIAN_POINT ( 'NONE',  ( 17.57812500061451644, 4.541064518000418104, 2.621784821874999949 ) ) ;
#36773 = ORIENTED_EDGE ( 'NONE', *, *, #41845, .F. ) ;
#36774 = CARTESIAN_POINT ( 'NONE',  ( 25.19999999999999929, -4.330127018922190985, -2.500000000000001332 ) ) ;
#36775 = CARTESIAN_POINT ( 'NONE',  ( 24.59062500061451573, -3.027376345333610441, -5.243569643749999898 ) ) ;
#36776 = CARTESIAN_POINT ( 'NONE',  ( 3.999999999999999112, 17.07499999999999929, 30.00000000000000000 ) ) ;
#36777 = DIRECTION ( 'NONE',  ( -1.000000000000000000, -0.000000000000000000, -0.000000000000000000 ) ) ;
#36778 = CARTESIAN_POINT ( 'NONE',  ( 13.68750000000000178, 5.773502691896255534, 3.535250795749688894E-16 ) ) ;
#36779 = CARTESIAN_POINT ( 'NONE',  ( 27.63750000122903216, 6.123233995736764310E-16, -4.999999999999998224 ) ) ;
#36780 = CARTESIAN_POINT ( 'NONE',  ( 21.70312500061451644, 0.000000000000000000, 5.243569643749999010 ) ) ;
#36781 = ORIENTED_EDGE ( 'NONE', *, *, #23281, .T. ) ;
#36782 = CARTESIAN_POINT ( 'NONE',  ( 23.13749999999999929, 5.773502691896255534, 3.535250795749688894E-16 ) ) ;
#36783 = CARTESIAN_POINT ( 'NONE',  ( 24.23437500061451644, 6.421520780324663323E-16, -5.243569643749999010 ) ) ;
#36784 =( BOUNDED_CURVE ( )  B_SPLINE_CURVE ( 2, ( #15618, #38160, #49625, #9726, #55167, #71795, #32260, #60683, #33353 ),
 .UNSPECIFIED., .F., .F. ) 
 B_SPLINE_CURVE_WITH_KNOTS ( ( 3, 2, 2, 2, 3 ),
 ( 0.2500000000000000000, 0.2536231884057971175, 0.2608695652173912971, 0.2681159420289855322, 0.2717391304347826497 ),
 .UNSPECIFIED. ) 
 CURVE ( )  GEOMETRIC_REPRESENTATION_ITEM ( )  RATIONAL_B_SPLINE_CURVE ( ( 0.9330127018922194093, 0.9330127018922190762, 1.000000000000000000, 0.8660254037844387076, 1.000000000000000000, 0.8660254037844387076, 1.000000000000000000, 0.9330127018922188542, 0.9330127018922194093 ) ) 
 REPRESENTATION_ITEM ( '' )  );
#36785 = ORIENTED_EDGE ( 'NONE', *, *, #21442, .T. ) ;
#36786 = DIRECTION ( 'NONE',  ( -0.000000000000000000, -0.000000000000000000, -1.000000000000000000 ) ) ;
#36787 = CARTESIAN_POINT ( 'NONE',  ( 13.41562500061451502, 3.027376345333613106, -5.243569643749998122 ) ) ;
#36788 = CARTESIAN_POINT ( 'NONE',  ( 3.628125000614518036, 4.541064518000418104, 2.621784821874999949 ) ) ;
#36789 = CARTESIAN_POINT ( 'NONE',  ( 17.07187500061451502, 4.119189519843966529, 2.378215178124999607 ) ) ;
#36790 = CARTESIAN_POINT ( 'NONE',  ( 25.67812500061451431, 4.541064518000418104, 2.621784821874999949 ) ) ;
#36791 = CARTESIAN_POINT ( 'NONE',  ( 12.97500000122903252, 2.886751345948126879, 4.999999999999999112 ) ) ;
#36792 = CARTESIAN_POINT ( 'NONE',  ( 18.45000000000000284, -4.330127018922190985, -2.500000000000001332 ) ) ;
#36793 = CARTESIAN_POINT ( 'NONE',  ( 26.47499999999999787, -4.330127018922194537, 2.499999999999995559 ) ) ;
#36794 = DIRECTION ( 'NONE',  ( -0.000000000000000000, -1.000000000000000000, -0.000000000000000000 ) ) ;
#36795 = CARTESIAN_POINT ( 'NONE',  ( 6.946875000614517681, -3.027376345333614438, 5.243569643749998122 ) ) ;
#36796 = CARTESIAN_POINT ( 'NONE',  ( 16.28437500061452070, 4.541064518000418104, 2.621784821874999949 ) ) ;
#36797 = B_SPLINE_CURVE_WITH_KNOTS ( 'NONE', 3,
 ( #40512, #6529, #23141, #67506, #39063, #33501 ),
 .UNSPECIFIED., .F., .F.,
 ( 4, 2, 4 ),
 ( 0.001054571168816651220, 0.001510402992670096395, 0.001966234816523541352 ),
 .UNSPECIFIED. ) ;
#36798 = ORIENTED_EDGE ( 'NONE', *, *, #36141, .T. ) ;
#36799 = CARTESIAN_POINT ( 'NONE',  ( 29.27812500061451573, 4.541064518000418104, 2.621784821874999949 ) ) ;
#36800 = CARTESIAN_POINT ( 'NONE',  ( 4.125000000000000000, 6.123233995736764310E-16, -4.999999999999998224 ) ) ;
#36801 = CARTESIAN_POINT ( 'NONE',  ( 4.584375000614516971, 4.541064518000418104, 2.621784821874999949 ) ) ;
#36802 = CARTESIAN_POINT ( 'NONE',  ( 16.50000000000000000, 0.000000000000000000, 4.999999999999998224 ) ) ;
#36803 = CARTESIAN_POINT ( 'NONE',  ( 12.77812500061451750, -4.541064518000419881, 2.621784821874995952 ) ) ;
#36804 = CARTESIAN_POINT ( 'NONE',  ( 25.81875000122903430, 2.886751345948157077, -4.999999999999949374 ) ) ;
#36805 = CARTESIAN_POINT ( 'NONE',  ( 9.618750001229033231, 2.886751345948129099, -4.999999999999997335 ) ) ;
#36806 = CARTESIAN_POINT ( 'NONE',  ( 18.15000000122903501, -2.886751345948125991, -5.000000000000000000 ) ) ;
#36807 = DIRECTION ( 'NONE',  ( 0.000000000000000000, 0.000000000000000000, -1.000000000000000000 ) ) ;
#36808 = CARTESIAN_POINT ( 'NONE',  ( 17.40937500061451715, -4.119189519843965641, -2.378215178125001383 ) ) ;
#36809 = CARTESIAN_POINT ( 'NONE',  ( 8.053125000614516082, 4.541064518000418104, -2.621784821874998173 ) ) ;
#36810 = CARTESIAN_POINT ( 'NONE',  ( 24.83437500061451431, 4.541064518000418104, 2.621784821874999949 ) ) ;
#36811 = CARTESIAN_POINT ( 'NONE',  ( 4.243569643749999010, 17.42187500061451999, 27.54997392385601174 ) ) ;
#36812 = CARTESIAN_POINT ( 'NONE',  ( 25.05937500061451573, -4.541064518000417216, -2.621784821875001281 ) ) ;
#36813 = CARTESIAN_POINT ( 'NONE',  ( 5.512499999999999289, 2.886751345948129099, -4.999999999999998224 ) ) ;
#36814 = CARTESIAN_POINT ( 'NONE',  ( 34.99999999999999289, -2.499999999999999556, -3.499999999999999556 ) ) ;
#36815 = CARTESIAN_POINT ( 'NONE',  ( 12.66562500061451502, 3.027376345333611329, 5.243569643749999010 ) ) ;
#36816 = CARTESIAN_POINT ( 'NONE',  ( 5.475000001229035185, -5.773502691896255534, -1.060575238724906372E-15 ) ) ;
#36817 = VECTOR ( 'NONE', #22650, 1000.000000000000000 ) ;
#36818 = CARTESIAN_POINT ( 'NONE',  ( 9.421875000614519990, 3.027376345333613106, -5.243569643749998122 ) ) ;
#36819 = DIRECTION ( 'NONE',  ( -1.000000000000000000, -0.000000000000000000, -0.000000000000000000 ) ) ;
#36820 = VERTEX_POINT ( 'NONE', #54677 ) ;
#36821 = CARTESIAN_POINT ( 'NONE',  ( 10.41562500061451679, 3.027376345333611329, 5.243569643749999010 ) ) ;
#36822 = CARTESIAN_POINT ( 'NONE',  ( 15.27187500061451786, 3.027376345333613106, -5.243569643749998122 ) ) ;
#36823 = CARTESIAN_POINT ( 'NONE',  ( 45.00000000000000000, 5.218601775200201409, 7.332543590861037686 ) ) ;
#36824 = CARTESIAN_POINT ( 'NONE',  ( 22.72500000122903430, 2.886751345948129099, -4.999999999999998224 ) ) ;
#36825 = CARTESIAN_POINT ( 'NONE',  ( 9.309375000614517504, -4.541064518000417216, -2.621784821875001281 ) ) ;
#36826 = CARTESIAN_POINT ( 'NONE',  ( 11.09062500061451573, -3.027376345333610441, -5.243569643749999898 ) ) ;
#36827 = EDGE_CURVE ( 'NONE', #10011, #63961, #72394, .T. ) ;
#36828 = CARTESIAN_POINT ( 'NONE',  ( 28.74375000122903501, -2.886751345948129988, 4.999999999999997335 ) ) ;
#36829 = CARTESIAN_POINT ( 'NONE',  ( 22.50937500061451857, 4.541064518000418104, -2.621784821874998173 ) ) ;
#36830 = CARTESIAN_POINT ( 'NONE',  ( 50.00000000000000000, -7.332543590861048344, 5.218601775200186310 ) ) ;
#36831 = CARTESIAN_POINT ( 'NONE',  ( 2.411242101361345515E-14, 20.88124999877096499, 34.00000000000000000 ) ) ;
#36832 = CARTESIAN_POINT ( 'NONE',  ( 30.00000000000000000, 0.000000000000000000, 0.000000000000000000 ) ) ;
#36833 = CARTESIAN_POINT ( 'NONE',  ( 2.121784821874999061, 15.65937500061451892, -33.67503911421598417 ) ) ;
#36834 = CARTESIAN_POINT ( 'NONE',  ( 14.97187500061451892, 3.027376345333611329, 5.243569643749999010 ) ) ;
#36835 = CARTESIAN_POINT ( 'NONE',  ( 16.53750000122903430, 4.330127018922191873, 2.499999999999999556 ) ) ;
#36836 = CARTESIAN_POINT ( 'NONE',  ( 11.14687500061451608, -3.027376345333610441, -5.243569643749999898 ) ) ;
#36837 = CARTESIAN_POINT ( 'NONE',  ( 4.243569643749999898, 18.19062500061451360, -27.54997392385601529 ) ) ;
#36838 = CARTESIAN_POINT ( 'NONE',  ( 17.92500000122903359, 2.886751345948126879, 4.999999999999999112 ) ) ;
#36839 = CARTESIAN_POINT ( 'NONE',  ( 12.92812500061451786, 6.421520780324663323E-16, -5.243569643749999010 ) ) ;
#36840 = ORIENTED_EDGE ( 'NONE', *, *, #3964, .T. ) ;
#36841 = CARTESIAN_POINT ( 'NONE',  ( 14.69999999999999929, 0.000000000000000000, 4.999999999999998224 ) ) ;
#36842 = CARTESIAN_POINT ( 'NONE',  ( 9.421875000614518214, 3.027376345333612662, -5.243569643749998122 ) ) ;
#36843 = CARTESIAN_POINT ( 'NONE',  ( -10.00000000000000000, 0.000000000000000000, 50.00000000000000000 ) ) ;
#36844 = CARTESIAN_POINT ( 'NONE',  ( 12.78750000122903430, 6.123233995736764310E-16, -4.999999999999998224 ) ) ;
#36845 = CARTESIAN_POINT ( 'NONE',  ( 20.81250000122903643, -4.330127018922190985, -2.500000000000001332 ) ) ;
#36846 = CARTESIAN_POINT ( 'NONE',  ( 17.84062500061451573, -3.027376345333610441, -5.243569643749999898 ) ) ;
#36847 = CARTESIAN_POINT ( 'NONE',  ( 21.62812500061451360, 4.541064518000418104, 2.621784821874999949 ) ) ;
#36848 = CARTESIAN_POINT ( 'NONE',  ( 26.92500000122903359, 2.886751345948126879, 4.999999999999999112 ) ) ;
#36849 = CARTESIAN_POINT ( 'NONE',  ( 25.98750000000000071, -2.886751345948129988, 4.999999999999997335 ) ) ;
#36850 = CARTESIAN_POINT ( 'NONE',  ( 30.00000000000000000, 0.000000000000000000, 0.000000000000000000 ) ) ;
#36851 = CARTESIAN_POINT ( 'NONE',  ( 28.68749999999999645, -2.886751345948129988, 4.999999999999997335 ) ) ;
#36852 = CARTESIAN_POINT ( 'NONE',  ( 28.05937500061451573, 0.000000000000000000, 5.243569643749999010 ) ) ;
#36853 = FACE_OUTER_BOUND ( 'NONE', #43663, .T. ) ;
#36854 = CARTESIAN_POINT ( 'NONE',  ( -4.243569643749999898, 13.10937500061451821, -30.00000000000000000 ) ) ;
#36855 = CARTESIAN_POINT ( 'NONE',  ( 3.712500001229034563, -4.330127018922190985, -2.500000000000001332 ) ) ;
#36856 = CARTESIAN_POINT ( 'NONE',  ( 4.575000000000002842, 6.123233995736764310E-16, -4.999999999999998224 ) ) ;
#36857 = CARTESIAN_POINT ( 'NONE',  ( 27.29999999999999716, 0.000000000000000000, 4.999999999999998224 ) ) ;
#36858 = CARTESIAN_POINT ( 'NONE',  ( 7.509375000614517681, -4.541064518000417216, -2.621784821875001281 ) ) ;
#36859 = VECTOR ( 'NONE', #71150, 1000.000000000000000 ) ;
#36860 = CARTESIAN_POINT ( 'NONE',  ( 29.54062500061451502, -3.027376345333610441, -5.243569643749999898 ) ) ;
#36861 = CARTESIAN_POINT ( 'NONE',  ( -0.4071169142669905927, 9.993716716995059812, -24.01045583075348233 ) ) ;
#36862 = DIRECTION ( 'NONE',  ( -0.000000000000000000, 8.673617379884035472E-17, 1.000000000000000000 ) ) ;
#36863 = CARTESIAN_POINT ( 'NONE',  ( 4.734375000614518214, -4.541064518000419881, 2.621784821874995952 ) ) ;
#36864 = CARTESIAN_POINT ( 'NONE',  ( 8.896875000614517859, -3.027376345333610441, -5.243569643749999898 ) ) ;
#36865 = CARTESIAN_POINT ( 'NONE',  ( 3.262500000000001510, 2.886751345948129099, -4.999999999999998224 ) ) ;
#36866 = CARTESIAN_POINT ( 'NONE',  ( -4.243569643749999898, 11.66562500061459495, 27.54997392385601529 ) ) ;
#36867 = CARTESIAN_POINT ( 'NONE',  ( 29.47499999999999787, 4.330127018922191873, 2.499999999999999556 ) ) ;
#36868 = CARTESIAN_POINT ( 'NONE',  ( 4.875000000000000888, -4.330127018922194537, 2.499999999999995559 ) ) ;
#36869 = EDGE_CURVE ( 'NONE', #11718, #41592, #11758, .T. ) ;
#36870 = CARTESIAN_POINT ( 'NONE',  ( 14.55937500061451750, -5.492252693125287522, -1.008910452111647106E-15 ) ) ;
#36871 = CARTESIAN_POINT ( 'NONE',  ( 20.27812500061451573, 4.541064518000418104, 2.621784821874999949 ) ) ;
#36872 = CARTESIAN_POINT ( 'NONE',  ( 10.79062500061451679, 6.054752690667223547, 3.707466751127219781E-16 ) ) ;
#36873 = CARTESIAN_POINT ( 'NONE',  ( 23.40937500061451715, 2.746126346562643317, 4.756430356249998326 ) ) ;
#36874 = CARTESIAN_POINT ( 'NONE',  ( 9.421875000614519990, 3.027376345333613106, -5.243569643749998122 ) ) ;
#36875 = CARTESIAN_POINT ( 'NONE',  ( 26.77499999999999858, 4.330127018922191873, 2.499999999999999556 ) ) ;
#36876 = CARTESIAN_POINT ( 'NONE',  ( 19.42500000122903714, -5.773502691896255534, -1.060575238724906372E-15 ) ) ;
#36877 = CARTESIAN_POINT ( 'NONE',  ( 28.34062500061451928, 6.054752690667223547, 3.707466751127219781E-16 ) ) ;
#36878 = CARTESIAN_POINT ( 'NONE',  ( 24.07499999999999929, 4.330127018922191873, 2.499999999999999556 ) ) ;
#36879 = CARTESIAN_POINT ( 'NONE',  ( 8.484375000614518214, 6.421520780324663323E-16, -5.243569643749999010 ) ) ;
#36880 = CARTESIAN_POINT ( 'NONE',  ( 14.55937500061451573, 0.000000000000000000, 5.243569643749999010 ) ) ;
#36881 = CARTESIAN_POINT ( 'NONE',  ( 26.67187500061451644, 3.027376345333611329, 5.243569643749999010 ) ) ;
#36882 = ADVANCED_FACE ( 'NONE', ( #11793 ), #68678, .F. ) ;
#36883 = CARTESIAN_POINT ( 'NONE',  ( 23.60625000122903216, 4.330127018922192761, -2.499999999999997780 ) ) ;
#36884 = CARTESIAN_POINT ( 'NONE',  ( 12.78749999999999964, 5.773502691896255534, 3.535250795749688894E-16 ) ) ;
#36885 = CARTESIAN_POINT ( 'NONE',  ( 19.28437500061451360, 6.421520780324663323E-16, -5.243569643749999010 ) ) ;
#36886 = CARTESIAN_POINT ( 'NONE',  ( 11.18437500061451928, 6.421520780324663323E-16, -5.243569643749999010 ) ) ;
#36887 = CARTESIAN_POINT ( 'NONE',  ( -1.878215178125001827, 20.25312499938548072, 33.25316411605952283 ) ) ;
#36888 = CARTESIAN_POINT ( 'NONE',  ( 24.37500000000000000, 6.123233995736764310E-16, -4.999999999999998224 ) ) ;
#36889 = CARTESIAN_POINT ( 'NONE',  ( 1.999999999999997335, 15.12500000000000000, 33.46410161513775705 ) ) ;
#36890 = CARTESIAN_POINT ( 'NONE',  ( -2.121784821874996840, 12.28437500061451892, -26.32496088578401583 ) ) ;
#36891 = CARTESIAN_POINT ( 'NONE',  ( 25.35937500061451644, 0.000000000000000000, 4.756430356249998326 ) ) ;
#36892 = CARTESIAN_POINT ( 'NONE',  ( 15.40312500061451573, 0.000000000000000000, 5.243569643749999010 ) ) ;
#36893 = CARTESIAN_POINT ( 'NONE',  ( 3.637500000000001954, -2.886751345948125991, -5.000000000000000000 ) ) ;
#36894 = EDGE_CURVE ( 'NONE', #55926, #33907, #6582, .T. ) ;
#36895 = SURFACE_SIDE_STYLE ('',( #14359 ) ) ;
#36896 = CARTESIAN_POINT ( 'NONE',  ( 12.33750000000000036, 5.773502691896255534, 3.535250795749688894E-16 ) ) ;
#36897 = CARTESIAN_POINT ( 'NONE',  ( 1.999999999999998668, 18.61250000122903359, 26.53589838486224650 ) ) ;
#36898 = CARTESIAN_POINT ( 'NONE',  ( 10.68750000122903288, 4.330127018922191873, 2.499999999999999556 ) ) ;
#36899 = CARTESIAN_POINT ( 'NONE',  ( 22.50937500061451857, 4.541064518000418104, -2.621784821874998173 ) ) ;
#36900 = CARTESIAN_POINT ( 'NONE',  ( 15.49687500061451750, -3.027376345333614438, 5.243569643749998122 ) ) ;
#36901 = DIRECTION ( 'NONE',  ( -1.000000000000000000, -0.000000000000000000, -0.000000000000000000 ) ) ;
#36902 = ORIENTED_EDGE ( 'NONE', *, *, #50559, .F. ) ;
#36903 = CARTESIAN_POINT ( 'NONE',  ( 16.82812500061451644, -4.541064518000419881, 2.621784821874995952 ) ) ;
#36904 = CARTESIAN_POINT ( 'NONE',  ( 5.090625000614516615, -3.027376345333614438, 5.243569643749998122 ) ) ;
#36905 = CARTESIAN_POINT ( 'NONE',  ( 18.38437500061451857, 6.421520780324663323E-16, -5.243569643749999010 ) ) ;
#36906 = CARTESIAN_POINT ( 'NONE',  ( 27.94687500061451502, 6.054752690667223547, 3.707466751127219781E-16 ) ) ;
#36907 = CARTESIAN_POINT ( 'NONE',  ( 3.740625000614516527, -3.027376345333614438, 5.243569643749998122 ) ) ;
#36908 = CARTESIAN_POINT ( 'NONE',  ( 19.52812500061451573, -4.541064518000419881, 2.621784821874995952 ) ) ;
#36909 = CARTESIAN_POINT ( 'NONE',  ( 9.001249775931846008E-16, 14.51562500061451466, 34.90005215228797653 ) ) ;
#36910 = CARTESIAN_POINT ( 'NONE',  ( 16.27500000122903501, -5.773502691896255534, -1.060575238724906372E-15 ) ) ;
#36911 = CARTESIAN_POINT ( 'NONE',  ( 11.70937500061451608, 4.119189519843966529, -2.378215178124998275 ) ) ;
#36912 = CARTESIAN_POINT ( 'NONE',  ( 6.253125000614517148, 4.541064518000418104, -2.621784821874998173 ) ) ;
#36913 = CARTESIAN_POINT ( 'NONE',  ( 28.90312500061451217, 0.000000000000000000, 5.243569643749999010 ) ) ;
#36914 = CARTESIAN_POINT ( 'NONE',  ( 7.593750001229034652, -2.886751345948130876, 4.999999999999996447 ) ) ;
#36915 = CARTESIAN_POINT ( 'NONE',  ( 22.50937500061451857, 4.541064518000418104, -2.621784821874998173 ) ) ;
#36916 = CARTESIAN_POINT ( 'NONE',  ( 13.97812500061451679, 4.541064518000418104, 2.621784821874999949 ) ) ;
#36917 = CARTESIAN_POINT ( 'NONE',  ( 25.38750000122903216, 6.123233995736764310E-16, -4.999999999999998224 ) ) ;
#36918 = CARTESIAN_POINT ( 'NONE',  ( 22.26562500061451644, -6.054752690667223547, -1.112240025338166033E-15 ) ) ;
#36919 = CARTESIAN_POINT ( 'NONE',  ( 19.62187500061451573, -6.054752690667223547, -1.112240025338166033E-15 ) ) ;
#36920 = CARTESIAN_POINT ( 'NONE',  ( 14.91562500061451679, 3.027376345333611329, 5.243569643749999010 ) ) ;
#36921 = CARTESIAN_POINT ( 'NONE',  ( 4.243569643749999898, 14.19687500061451857, 32.45002607614398471 ) ) ;
#36922 = CARTESIAN_POINT ( 'NONE',  ( 20.16562500061451146, 3.027376345333613106, -5.243569643749998122 ) ) ;
#36923 = CARTESIAN_POINT ( 'NONE',  ( 29.80312500061451431, 0.000000000000000000, 5.243569643749999010 ) ) ;
#36924 = EDGE_LOOP ( 'NONE', ( #59760, #32430, #47460, #65732 ) ) ;
#36925 = ORIENTED_EDGE ( 'NONE', *, *, #61652, .F. ) ;
#36926 = CARTESIAN_POINT ( 'NONE',  ( 23.55000000000000071, 4.330127018922192761, -2.499999999999997780 ) ) ;
#36927 = CARTESIAN_POINT ( 'NONE',  ( -1.999999999999997113, 11.07500000000000107, -26.53589838486224295 ) ) ;
#36928 = CARTESIAN_POINT ( 'NONE',  ( 3.779449423378813400, -3.273493860712442860, -3.876766845908668824 ) ) ;
#36929 = CARTESIAN_POINT ( 'NONE',  ( 26.24062500061451431, -3.027376345333614438, 5.243569643749998122 ) ) ;
#36930 = CARTESIAN_POINT ( 'NONE',  ( 7.678125000614516082, 4.541064518000418104, 2.621784821874999949 ) ) ;
#36931 = CARTESIAN_POINT ( 'NONE',  ( 19.20000000122903572, 5.773502691896255534, 3.535250795749688894E-16 ) ) ;
#36932 = EDGE_CURVE ( 'NONE', #1400, #38366, #28781, .T. ) ;
#36933 = CARTESIAN_POINT ( 'NONE',  ( 25.15312500061451217, 4.541064518000418104, -2.621784821874998173 ) ) ;
#36934 = CARTESIAN_POINT ( 'NONE',  ( 22.08749999999999858, -2.886751345948125991, -5.000000000000000000 ) ) ;
#36935 = CARTESIAN_POINT ( 'NONE',  ( 28.34062500061451928, 6.054752690667223547, 3.707466751127219781E-16 ) ) ;
#36936 = CARTESIAN_POINT ( 'NONE',  ( 8.990625000614516082, 6.054752690667223547, 3.707466751127219781E-16 ) ) ;
#36937 = VERTEX_POINT ( 'NONE', #34310 ) ;
#36938 = CARTESIAN_POINT ( 'NONE',  ( 24.02812500061451573, -4.541064518000419881, 2.621784821874995952 ) ) ;
#36939 = CARTESIAN_POINT ( 'NONE',  ( 6.403125000614517504, 0.000000000000000000, 5.243569643749999010 ) ) ;
#36940 = CARTESIAN_POINT ( 'NONE',  ( 13.09687500061451892, 5.492252693125287522, 3.363034840372157021E-16 ) ) ;
#36941 = CARTESIAN_POINT ( 'NONE',  ( 4.115625000614516082, 3.027376345333611329, 5.243569643749999010 ) ) ;
#36942 = CARTESIAN_POINT ( 'NONE',  ( 2.000000000000001332, 13.51250000122903394, -26.53589838486224650 ) ) ;
#36943 = CARTESIAN_POINT ( 'NONE',  ( 21.95625000122903003, 0.000000000000000000, 4.999999999999998224 ) ) ;
#36944 = CARTESIAN_POINT ( 'NONE',  ( 11.51250000000000107, 2.886751345948126879, 4.999999999999999112 ) ) ;
#36945 = CARTESIAN_POINT ( 'NONE',  ( 10.50937500061451679, 0.000000000000000000, 5.243569643749999010 ) ) ;
#36946 = CARTESIAN_POINT ( 'NONE',  ( 8.062500001229034652, 0.000000000000000000, 4.999999999999998224 ) ) ;
#36947 = CARTESIAN_POINT ( 'NONE',  ( 14.78437500061451715, 6.421520780324663323E-16, -5.243569643749999010 ) ) ;
#36948 = CARTESIAN_POINT ( 'NONE',  ( 15.45000000000000107, 4.330127018922192761, -2.499999999999997780 ) ) ;
#36949 = CARTESIAN_POINT ( 'NONE',  ( 6.534375000614517148, -4.541064518000419881, 2.621784821874995952 ) ) ;
#36950 = CARTESIAN_POINT ( 'NONE',  ( 9.001249775931846008E-16, 10.46562500061451928, -25.09994784771203058 ) ) ;
#36951 = CARTESIAN_POINT ( 'NONE',  ( 30.00000000000000000, 0.000000000000000000, 0.000000000000000000 ) ) ;
#36952 = CARTESIAN_POINT ( 'NONE',  ( 12.94687500061451857, -3.027376345333610441, -5.243569643749999898 ) ) ;
#36953 = CARTESIAN_POINT ( 'NONE',  ( 22.04062500061451502, 6.054752690667223547, 3.707466751127219781E-16 ) ) ;
#36954 = CARTESIAN_POINT ( 'NONE',  ( 9.001249775931846008E-16, 10.52187500061451964, 34.90005215228797653 ) ) ;
#36955 = DIRECTION ( 'NONE',  ( -1.000000000000000000, -0.000000000000000000, -0.000000000000000000 ) ) ;
#36956 = CARTESIAN_POINT ( 'NONE',  ( 27.23437500061451644, -4.541064518000419881, 2.621784821874995952 ) ) ;
#36957 = CARTESIAN_POINT ( 'NONE',  ( -1.626862140677534273E-15, 16.43750000000000000, 34.00000000000000000 ) ) ;
#36958 = CARTESIAN_POINT ( 'NONE',  ( 3.365625000614516082, -6.054752690667223547, -1.112240025338166033E-15 ) ) ;
#36959 = CARTESIAN_POINT ( 'NONE',  ( 22.47187500061451360, 4.119189519843966529, 2.378215178124999607 ) ) ;
#36960 = CARTESIAN_POINT ( 'NONE',  ( 17.67187500061451644, 3.027376345333611329, 5.243569643749999010 ) ) ;
#36961 = CARTESIAN_POINT ( 'NONE',  ( 9.309375000614517504, 2.746126346562645981, -4.756430356249997438 ) ) ;
#36962 = CARTESIAN_POINT ( 'NONE',  ( 27.22500000122903430, 2.886751345948129099, -4.999999999999998224 ) ) ;
#36963 = CARTESIAN_POINT ( 'NONE',  ( 6.084375000614518747, -4.541064518000419881, 2.621784821874995952 ) ) ;
#36964 = CARTESIAN_POINT ( 'NONE',  ( 16.80937500061451573, 0.000000000000000000, 5.243569643749999010 ) ) ;
#36965 = CARTESIAN_POINT ( 'NONE',  ( 4.809916128174254624, -1.365542690628744449, -5.062639209831853115 ) ) ;
#36966 = CARTESIAN_POINT ( 'NONE',  ( 23.62500000000000000, 4.330127018922191873, 2.499999999999999556 ) ) ;
#36967 = CARTESIAN_POINT ( 'NONE',  ( 4.687500001229034652, 6.123233995736764310E-16, -4.999999999999998224 ) ) ;
#36968 = CARTESIAN_POINT ( 'NONE',  ( 26.63437500061451857, 4.541064518000418104, 2.621784821874999949 ) ) ;
#36969 = CARTESIAN_POINT ( 'NONE',  ( 1.878215178124997609, 14.47812499938548214, 33.25316411605952993 ) ) ;
#36970 = CARTESIAN_POINT ( 'NONE',  ( 6.899999999999999467, 4.330127018922192761, -2.499999999999997780 ) ) ;
#36971 = CARTESIAN_POINT ( 'NONE',  ( 8.559375000614515727, 2.746126346562643317, 4.756430356249998326 ) ) ;
#36972 = CARTESIAN_POINT ( 'NONE',  ( 23.20312500061451644, -4.541064518000417216, -2.621784821875001281 ) ) ;
#36973 = CARTESIAN_POINT ( 'NONE',  ( 12.07499999999999929, -4.330127018922194537, 2.499999999999995559 ) ) ;
#36974 = EDGE_CURVE ( 'NONE', #38724, #60669, #49511, .T. ) ;
#36975 = CARTESIAN_POINT ( 'NONE',  ( 7.453125000614516438, -4.541064518000417216, -2.621784821875001281 ) ) ;
#36976 = CARTESIAN_POINT ( 'NONE',  ( 18.56250000000000000, 2.886751345948129099, -4.999999999999998224 ) ) ;
#36977 = CARTESIAN_POINT ( 'NONE',  ( 18.51562500061451289, 3.027376345333611329, 5.243569643749999010 ) ) ;
#36978 = CARTESIAN_POINT ( 'NONE',  ( 4.192336996406676342, -2.724758798235080715, 4.480034832487019614 ) ) ;
#36979 = CARTESIAN_POINT ( 'NONE',  ( 23.62500000122902932, 2.886751345948129099, -4.999999999999998224 ) ) ;
#36980 = CARTESIAN_POINT ( 'NONE',  ( 2.655984681222220721E-16, 18.60312499938548925, 25.66244784525396483 ) ) ;
#36981 = CARTESIAN_POINT ( 'NONE',  ( 29.82187500061451502, 3.027376345333611329, 5.243569643749999010 ) ) ;
#36982 = ORIENTED_EDGE ( 'NONE', *, *, #52495, .T. ) ;
#36983 = CARTESIAN_POINT ( 'NONE',  ( 20.61562500061451431, 3.027376345333613106, -5.243569643749998122 ) ) ;
#36984 = CARTESIAN_POINT ( 'NONE',  ( 25.86562500061451431, -6.054752690667223547, -1.112240025338166033E-15 ) ) ;
#36985 = CARTESIAN_POINT ( 'NONE',  ( 23.85937500061451644, 4.541064518000418104, -2.621784821874998173 ) ) ;
#36986 = CARTESIAN_POINT ( 'NONE',  ( 7.875000000000000000, 4.330127018922191873, 2.499999999999999556 ) ) ;
#36987 = CARTESIAN_POINT ( 'NONE',  ( 12.66562500061451502, 3.027376345333611329, 5.243569643749999010 ) ) ;
#36988 = CARTESIAN_POINT ( 'NONE',  ( 27.85312500061451502, 4.541064518000418104, -2.621784821874998173 ) ) ;
#36989 = CARTESIAN_POINT ( 'NONE',  ( 16.95937500061451786, -4.541064518000417216, -2.621784821875001281 ) ) ;
#36990 = CARTESIAN_POINT ( 'NONE',  ( 8.390625000614518214, -3.027376345333610441, -5.243569643749999898 ) ) ;
#36991 = CARTESIAN_POINT ( 'NONE',  ( 14.19375000122903252, 5.773502691896255534, 3.535250795749688401E-16 ) ) ;
#36992 = CARTESIAN_POINT ( 'NONE',  ( -4.243569643749997233, 11.34687500061451892, 32.45002607614398471 ) ) ;
#36993 = CARTESIAN_POINT ( 'NONE',  ( 24.48750000122903359, 6.123233995736764310E-16, -4.999999999999998224 ) ) ;
#36994 = CARTESIAN_POINT ( 'NONE',  ( 18.83437500061451431, 5.824947211148865298E-16, -4.756430356249998326 ) ) ;
#36995 = CARTESIAN_POINT ( 'NONE',  ( 13.71562500061451750, -6.054752690667223547, -1.112240025338166033E-15 ) ) ;
#36996 = CARTESIAN_POINT ( 'NONE',  ( 10.35937500061451644, 4.541064518000418104, -2.621784821874998173 ) ) ;
#36997 = CARTESIAN_POINT ( 'NONE',  ( 9.534375000614517148, 4.541064518000418104, 2.621784821874999949 ) ) ;
#36998 = ORIENTED_EDGE ( 'NONE', *, *, #34668, .F. ) ;
#36999 = CARTESIAN_POINT ( 'NONE',  ( -0.4071169142669882612, 9.993716716995061589, 35.98954416924652122 ) ) ;
#37000 = CARTESIAN_POINT ( 'NONE',  ( 21.92812500061451431, 6.421520780324663323E-16, -5.243569643749999010 ) ) ;
#37001 =( BOUNDED_CURVE ( )  B_SPLINE_CURVE ( 2, ( #38603, #44523, #61487, #27887, #66680, #67056, #49325 ),
 .UNSPECIFIED., .F., .F. ) 
 B_SPLINE_CURVE_WITH_KNOTS ( ( 3, 2, 2, 3 ),
 ( 0.9400000000000001688, 0.9433333333333335791, 0.9466666666666667673, 0.9500000000000000666 ),
 .UNSPECIFIED. ) 
 CURVE ( )  GEOMETRIC_REPRESENTATION_ITEM ( )  RATIONAL_B_SPLINE_CURVE ( ( 0.9999999999999911182, 0.8660254037844475894, 1.000000000000000000, 0.8660254037844387076, 1.000000000000000000, 0.8660254037844342667, 1.000000000000004441 ) ) 
 REPRESENTATION_ITEM ( '' )  );
#37002 = CARTESIAN_POINT ( 'NONE',  ( 16.84687500061451715, -3.027376345333614438, 5.243569643749998122 ) ) ;
#37003 = CARTESIAN_POINT ( 'NONE',  ( 21.06562500061451715, 3.027376345333613106, -5.243569643749998122 ) ) ;
#37004 = CARTESIAN_POINT ( 'NONE',  ( 1.999999999999998668, 12.20000000000000107, 26.53589838486224650 ) ) ;
#37005 = CARTESIAN_POINT ( 'NONE',  ( 26.27812500061451573, -4.541064518000419881, 2.621784821874995952 ) ) ;
#37006 = CARTESIAN_POINT ( 'NONE',  ( 6.637500001229035718, 4.330127018922191873, 2.499999999999999556 ) ) ;
#37007 = ORIENTED_EDGE ( 'NONE', *, *, #20885, .T. ) ;
#37008 = CARTESIAN_POINT ( 'NONE',  ( 29.13749999999999929, -2.886751345948129988, 4.999999999999997335 ) ) ;
#37009 = CARTESIAN_POINT ( 'NONE',  ( 1.999999999999998668, 18.05000000000000071, -33.46410161513775705 ) ) ;
#37010 = CARTESIAN_POINT ( 'NONE',  ( 25.68750000122903288, -4.330127018922194537, 2.499999999999995559 ) ) ;
#37011 = CARTESIAN_POINT ( 'NONE',  ( 3.756430356249998770, 14.06562499938548250, 32.16877607737302469 ) ) ;
#37012 = CARTESIAN_POINT ( 'NONE',  ( 8.259375000614518569, 0.000000000000000000, 5.243569643749999010 ) ) ;
#37013 = DIRECTION ( 'NONE',  ( 0.000000000000000000, 0.000000000000000000, 1.000000000000000000 ) ) ;
#37014 = CARTESIAN_POINT ( 'NONE',  ( 16.11562500061451786, 3.027376345333613106, -5.243569643749998122 ) ) ;
#37015 = CARTESIAN_POINT ( 'NONE',  ( 7.546875000614517326, -3.027376345333610441, -5.243569643749999898 ) ) ;
#37016 = CARTESIAN_POINT ( 'NONE',  ( 25.98750000122903003, 4.330127018922191873, 2.499999999999999556 ) ) ;
#37017 = CARTESIAN_POINT ( 'NONE',  ( 18.04687500061451999, 6.054752690667223547, 3.707466751127219781E-16 ) ) ;
#37018 = CARTESIAN_POINT ( 'NONE',  ( 4.621875000614516615, 3.027376345333611329, 5.243569643749999010 ) ) ;
#37019 = CARTESIAN_POINT ( 'NONE',  ( 4.896606315213732685, -1.024120609751041799, 4.896606315213732685 ) ) ;
#37020 = CARTESIAN_POINT ( 'NONE',  ( 6.215625000614517504, 3.027376345333613106, -5.243569643749998122 ) ) ;
#37021 = CARTESIAN_POINT ( 'NONE',  ( 15.92812500061451608, -4.541064518000419881, 2.621784821874995952 ) ) ;
#37022 = ORIENTED_EDGE ( 'NONE', *, *, #8224, .F. ) ;
#37023 = CARTESIAN_POINT ( 'NONE',  ( 12.14062500061451821, 6.054752690667223547, 3.707466751127219781E-16 ) ) ;
#37024 = CARTESIAN_POINT ( 'NONE',  ( 4.650000001229035895, -2.886751345948125991, -5.000000000000000000 ) ) ;
#37025 = CARTESIAN_POINT ( 'NONE',  ( 9.590625000614517504, -3.027376345333614438, 5.243569643749998122 ) ) ;
#37026 = CARTESIAN_POINT ( 'NONE',  ( 20.22187500061451715, 2.746126346562645981, -4.756430356249997438 ) ) ;
#37027 = CARTESIAN_POINT ( 'NONE',  ( 11.81250000000000000, 2.886751345948129099, -4.999999999999998224 ) ) ;
#37028 = EDGE_CURVE ( 'NONE', #28470, #28191, #6147, .T. ) ;
#37029 = CARTESIAN_POINT ( 'NONE',  ( 5.175000001229033586, 2.886751345948129099, -4.999999999999998224 ) ) ;
#37030 = CARTESIAN_POINT ( 'NONE',  ( 21.48750000000000071, -2.886751345948129988, 4.999999999999997335 ) ) ;
#37031 = CARTESIAN_POINT ( 'NONE',  ( 15.53437500061451715, -4.541064518000419881, 2.621784821874995952 ) ) ;
#37032 = CARTESIAN_POINT ( 'NONE',  ( 16.27500000122903501, -5.773502691896255534, -1.060575238724906372E-15 ) ) ;
#37033 = CARTESIAN_POINT ( 'NONE',  ( 23.21250000000000213, 2.886751345948126879, 4.999999999999999112 ) ) ;
#37034 = CARTESIAN_POINT ( 'NONE',  ( 2.121784821875001281, 18.60312500061451857, -26.32496088578401938 ) ) ;
#37035 = CARTESIAN_POINT ( 'NONE',  ( -1.999999999999997113, 16.13750000122903216, 33.46410161513775705 ) ) ;
#37036 = DIRECTION ( 'NONE',  ( -0.000000000000000000, -1.000000000000000000, -0.000000000000000000 ) ) ;
#37037 = LINE ( 'NONE', #42953, #2898 ) ;
#37038 = CARTESIAN_POINT ( 'NONE',  ( 10.87500000000000000, 6.123233995736764310E-16, -4.999999999999998224 ) ) ;
#37039 = CARTESIAN_POINT ( 'NONE',  ( 19.48125000122903216, 6.123233995736764310E-16, -4.999999999999998224 ) ) ;
#37040 = CARTESIAN_POINT ( 'NONE',  ( 16.17187500061451644, 3.027376345333613106, -5.243569643749998122 ) ) ;
#37041 = CARTESIAN_POINT ( 'NONE',  ( 29.02499999999999858, 4.330127018922191873, 2.499999999999999556 ) ) ;
#37042 = CARTESIAN_POINT ( 'NONE',  ( 12.51562500061451821, 3.027376345333613106, -5.243569643749998122 ) ) ;
#37043 = CARTESIAN_POINT ( 'NONE',  ( 28.77187500061451431, 4.119189519843966529, 2.378215178124999607 ) ) ;
#37044 = CARTESIAN_POINT ( 'NONE',  ( 23.52187500061451786, 3.027376345333611329, 5.243569643749999010 ) ) ;
#37045 = CARTESIAN_POINT ( 'NONE',  ( 15.79687500061451644, 0.000000000000000000, 4.756430356249998326 ) ) ;
#37046 = CARTESIAN_POINT ( 'NONE',  ( 7.603125000614517681, 4.541064518000418104, -2.621784821874998173 ) ) ;
#37047 = CARTESIAN_POINT ( 'NONE',  ( 12.98437500061451821, 6.421520780324663323E-16, -5.243569643749999010 ) ) ;
#37048 = VERTEX_POINT ( 'NONE', #18401 ) ;
#37049 = CARTESIAN_POINT ( 'NONE',  ( 25.02187500061451431, -6.054752690667223547, -1.112240025338166033E-15 ) ) ;
#37050 = CARTESIAN_POINT ( 'NONE',  ( 27.10312500061451502, 0.000000000000000000, 5.243569643749999010 ) ) ;
#37051 = DIRECTION ( 'NONE',  ( 0.000000000000000000, 1.000000000000000000, 0.000000000000000000 ) ) ;
#37052 = CARTESIAN_POINT ( 'NONE',  ( 7.275000000000000355, 6.123233995736764310E-16, -4.999999999999998224 ) ) ;
#37053 = CARTESIAN_POINT ( 'NONE',  ( 17.32500000122903216, 2.886751345948129099, -4.999999999999998224 ) ) ;
#37054 = CARTESIAN_POINT ( 'NONE',  ( -3.999999999999997335, 17.90000000122903501, -27.69059892324149530 ) ) ;
#37055 = CARTESIAN_POINT ( 'NONE',  ( 0.000000000000000000, 20.00000000000000000, -30.00000000000000000 ) ) ;
#37056 = VERTEX_POINT ( 'NONE', #6620 ) ;
#37057 = EDGE_CURVE ( 'NONE', #22838, #68526, #19277, .T. ) ;
#37058 = CARTESIAN_POINT ( 'NONE',  ( 15.03749999999999964, 5.773502691896255534, 3.535250795749688894E-16 ) ) ;
#37059 = CARTESIAN_POINT ( 'NONE',  ( 18.41250000000000142, -5.773502691896255534, -1.060575238724906372E-15 ) ) ;
#37060 = CARTESIAN_POINT ( 'NONE',  ( 12.96562500061451750, 3.027376345333613106, -5.243569643749998122 ) ) ;
#37061 = ORIENTED_EDGE ( 'NONE', *, *, #55693, .F. ) ;
#37062 = CARTESIAN_POINT ( 'NONE',  ( -1.071796769724496334, 16.62634618820329990, 26.00000000000000355 ) ) ;
#37063 = CARTESIAN_POINT ( 'NONE',  ( 9.001249775931846008E-16, 17.72187500061451715, -25.09994784771203058 ) ) ;
#37064 = CARTESIAN_POINT ( 'NONE',  ( 29.25000000122903288, -2.886751345948129988, 4.999999999999997335 ) ) ;
#37065 = CARTESIAN_POINT ( 'NONE',  ( -1.878215178125001827, 13.39062499938548356, 33.25316411605952283 ) ) ;
#37066 = CARTESIAN_POINT ( 'NONE',  ( 11.36250000000000071, 2.886751345948129099, -4.999999999999998224 ) ) ;
#37067 = CARTESIAN_POINT ( 'NONE',  ( 29.25937500061451857, 2.746126346562643317, 4.756430356249998326 ) ) ;
#37068 = VECTOR ( 'NONE', #63473, 1000.000000000000000 ) ;
#37069 = ORIENTED_EDGE ( 'NONE', *, *, #19260, .F. ) ;
#37070 = CARTESIAN_POINT ( 'NONE',  ( 4.243569643749999898, 15.94062500061451537, 32.45002607614398471 ) ) ;
#37071 = CARTESIAN_POINT ( 'NONE',  ( 27.81562500061452070, 3.027376345333613106, -5.243569643749998122 ) ) ;
#37072 = CARTESIAN_POINT ( 'NONE',  ( 25.78125000122903288, 6.123233995736764310E-16, -4.999999999999998224 ) ) ;
#37073 = CARTESIAN_POINT ( 'NONE',  ( -3.756430356249999214, 19.57812499938548001, 27.83122392262697531 ) ) ;
#37074 = CARTESIAN_POINT ( 'NONE',  ( 24.45937500061451786, 0.000000000000000000, 5.243569643749999010 ) ) ;
#37075 = CARTESIAN_POINT ( 'NONE',  ( 18.40312500061451573, 4.541064518000418104, -2.621784821874998173 ) ) ;
#37076 = CARTESIAN_POINT ( 'NONE',  ( 2.121784821874999061, 13.35312500061459495, -33.67503911421598417 ) ) ;
#37077 = CARTESIAN_POINT ( 'NONE',  ( 24.30000000122903359, -2.886751345948129988, 4.999999999999997335 ) ) ;
#37078 = CARTESIAN_POINT ( 'NONE',  ( 4.940625000614515372, 6.054752690667223547, 3.707466751127219781E-16 ) ) ;
#37079 = CARTESIAN_POINT ( 'NONE',  ( 26.40937500061451715, -4.119189519843965641, -2.378215178125001383 ) ) ;
#37080 = CARTESIAN_POINT ( 'NONE',  ( 22.30312500061451431, -4.541064518000417216, -2.621784821875001281 ) ) ;
#37081 = CARTESIAN_POINT ( 'NONE',  ( 11.52187500061451608, -5.492252693125287522, -1.008910452111647106E-15 ) ) ;
#37082 = CARTESIAN_POINT ( 'NONE',  ( -1.878215178124999163, 16.39062499938548356, 26.74683588394047007 ) ) ;
#37083 = CARTESIAN_POINT ( 'NONE',  ( 18.57187500061451857, 3.027376345333611329, 5.243569643749999010 ) ) ;
#37084 = CARTESIAN_POINT ( 'NONE',  ( 16.20937500061451786, 4.541064518000418104, -2.621784821874998173 ) ) ;
#37085 = CARTESIAN_POINT ( 'NONE',  ( 23.85937500061451644, 4.541064518000418104, -2.621784821874998173 ) ) ;
#37086 = CARTESIAN_POINT ( 'NONE',  ( -3.000416591977282496E-16, 15.24687500061451928, 25.09994784771203058 ) ) ;
#37087 = CARTESIAN_POINT ( 'NONE',  ( 6.028125000614517504, -4.541064518000419881, 2.621784821874995952 ) ) ;
#37088 = CARTESIAN_POINT ( 'NONE',  ( 29.27812500061451573, 4.541064518000418104, 2.621784821874999949 ) ) ;
#37089 = CARTESIAN_POINT ( 'NONE',  ( 28.37812500061451715, 4.541064518000418104, 2.621784821874999949 ) ) ;
#37090 = CARTESIAN_POINT ( 'NONE',  ( 1.071796769724488785, 17.35759618943233562, 34.00000000000000000 ) ) ;
#37091 = CARTESIAN_POINT ( 'NONE',  ( -2.000000000000000000, 19.47499999999999787, 26.53589838486224650 ) ) ;
#37092 = CARTESIAN_POINT ( 'NONE',  ( 7.396875000614519635, -3.027376345333614438, 5.243569643749998122 ) ) ;
#37093 = CARTESIAN_POINT ( 'NONE',  ( 14.92500000122903181, -5.773502691896255534, -1.060575238724906372E-15 ) ) ;
#37094 = CARTESIAN_POINT ( 'NONE',  ( 9.075000001229033941, -5.773502691896255534, -1.060575238724906372E-15 ) ) ;
#37095 = CARTESIAN_POINT ( 'NONE',  ( 4.378125000614518925, 6.421520780324663323E-16, -5.243569643749999010 ) ) ;
#37096 = CARTESIAN_POINT ( 'NONE',  ( 4.000000000000000000, 15.18124999877096570, 27.69059892324149530 ) ) ;
#37097 = CARTESIAN_POINT ( 'NONE',  ( 21.50625000122903074, 0.000000000000000000, 4.999999999999998224 ) ) ;
#37098 = CARTESIAN_POINT ( 'NONE',  ( 15.08437500061451786, -4.541064518000419881, 2.621784821874995952 ) ) ;
#37099 = CARTESIAN_POINT ( 'NONE',  ( 21.18749999999999645, -2.886751345948126435, -5.000000000000000000 ) ) ;
#37100 = ORIENTED_EDGE ( 'NONE', *, *, #33859, .F. ) ;
#37101 = CARTESIAN_POINT ( 'NONE',  ( 22.90312500061451573, 4.541064518000418104, -2.621784821874998173 ) ) ;
#37102 = CARTESIAN_POINT ( 'NONE',  ( 7.978125000614517681, 6.421520780324663323E-16, -5.243569643749999010 ) ) ;
#37103 = CARTESIAN_POINT ( 'NONE',  ( 23.37187500061451573, 3.027376345333612662, -5.243569643749998122 ) ) ;
#37104 = CARTESIAN_POINT ( 'NONE',  ( 7.340625000614518392, -3.027376345333614438, 5.243569643749998122 ) ) ;
#37105 = CARTESIAN_POINT ( 'NONE',  ( 23.08125000122903359, 6.123233995736764310E-16, -4.999999999999998224 ) ) ;
#37106 = CARTESIAN_POINT ( 'NONE',  ( 8.287500001229034297, 6.123233995736764310E-16, -4.999999999999998224 ) ) ;
#37107 = CARTESIAN_POINT ( 'NONE',  ( 21.85312500061451502, -4.541064518000417216, -2.621784821875001281 ) ) ;
#37108 = CARTESIAN_POINT ( 'NONE',  ( 9.001249775931846008E-16, 10.91562500061451857, -25.09994784771203058 ) ) ;
#37109 = CARTESIAN_POINT ( 'NONE',  ( 10.20000000122903572, 5.773502691896255534, 3.535250795749688894E-16 ) ) ;
#37110 = CARTESIAN_POINT ( 'NONE',  ( 19.49062500061451431, -3.027376345333614438, 5.243569643749998122 ) ) ;
#37111 = CARTESIAN_POINT ( 'NONE',  ( 18.40312500061451573, 4.541064518000418104, -2.621784821874998173 ) ) ;
#37112 = CARTESIAN_POINT ( 'NONE',  ( 27.30937500061451573, -4.119189519843965641, -2.378215178125001383 ) ) ;
#37113 = CARTESIAN_POINT ( 'NONE',  ( 18.18750000000000000, 5.773502691896255534, 3.535250795749688894E-16 ) ) ;
#37114 = CARTESIAN_POINT ( 'NONE',  ( 12.41250000122903430, 4.330127018922192761, -2.499999999999997780 ) ) ;
#37115 = CARTESIAN_POINT ( 'NONE',  ( 10.11562500061451608, -6.054752690667223547, -1.112240025338166033E-15 ) ) ;
#37116 = CARTESIAN_POINT ( 'NONE',  ( 13.49062500061451608, 6.054752690667223547, 3.707466751127219781E-16 ) ) ;
#37117 = CARTESIAN_POINT ( 'NONE',  ( 23.70000000122903216, 5.773502691896255534, 3.535250795749688894E-16 ) ) ;
#37118 = AXIS2_PLACEMENT_3D ( 'NONE', #24492, #69571, #11966 ) ;
#37119 = CARTESIAN_POINT ( 'NONE',  ( 22.17187500061451644, 3.027376345333611329, 5.243569643749999010 ) ) ;
#37120 = DIRECTION ( 'NONE',  ( 0.000000000000000000, 0.7071067811865388020, -0.7071067811865562325 ) ) ;
#37121 = CARTESIAN_POINT ( 'NONE',  ( 5.775000001229033231, 2.886751345948126879, 4.999999999999999112 ) ) ;
#37122 = CARTESIAN_POINT ( 'NONE',  ( 6.946875000614517681, -3.027376345333614438, 5.243569643749998122 ) ) ;
#37123 = CARTESIAN_POINT ( 'NONE',  ( 23.52187500061451786, 3.027376345333611329, 5.243569643749999010 ) ) ;
#37124 = CARTESIAN_POINT ( 'NONE',  ( 26.73750000122903003, 6.123233995736764310E-16, -4.999999999999998224 ) ) ;
#37125 = VECTOR ( 'NONE', #37251, 1000.000000000000000 ) ;
#37126 = CARTESIAN_POINT ( 'NONE',  ( 17.95312500061451644, 4.541064518000418104, -2.621784821874998173 ) ) ;
#37127 = CARTESIAN_POINT ( 'NONE',  ( 24.12187500061451217, -6.054752690667223547, -1.112240025338166033E-15 ) ) ;
#37128 = CARTESIAN_POINT ( 'NONE',  ( 2.655984681222220721E-16, 18.71562499938548285, 25.66244784525396483 ) ) ;
#37129 = CARTESIAN_POINT ( 'NONE',  ( 9.412500001229034297, 0.000000000000000000, 4.999999999999998224 ) ) ;
#37130 = CARTESIAN_POINT ( 'NONE',  ( 27.82500000122903572, 2.886751345948119329, 5.000000000000014211 ) ) ;
#37131 = CARTESIAN_POINT ( 'NONE',  ( 5.671875000614519102, -6.054752690667223547, -1.112240025338166033E-15 ) ) ;
#37132 = CARTESIAN_POINT ( 'NONE',  ( 16.15312500061451573, 4.541064518000418104, -2.621784821874998173 ) ) ;
#37133 = AXIS2_PLACEMENT_3D ( 'NONE', #2522, #71586, #26892 ) ;
#37134 = CARTESIAN_POINT ( 'NONE',  ( 14.25937500061451679, -4.541064518000417216, -2.621784821875001281 ) ) ;
#37135 = ORIENTED_EDGE ( 'NONE', *, *, #20329, .T. ) ;
#37136 = LINE ( 'NONE', #20498, #40747 ) ;
#37137 = CARTESIAN_POINT ( 'NONE',  ( 24.02812500061451573, -4.541064518000419881, 2.621784821874995952 ) ) ;
#37138 = CARTESIAN_POINT ( 'NONE',  ( 5.810221930991193690E-16, 17.11249999999999716, 26.00000000000000000 ) ) ;
#37139 = FACE_OUTER_BOUND ( 'NONE', #39931, .T. ) ;
#37140 = CARTESIAN_POINT ( 'NONE',  ( 14.69999999999999929, 0.000000000000000000, 4.999999999999998224 ) ) ;
#37141 = EDGE_CURVE ( 'NONE', #72227, #30208, #40596, .T. ) ;
#37142 = CARTESIAN_POINT ( 'NONE',  ( 23.88750000122903216, -4.330127018922194537, 2.499999999999995559 ) ) ;
#37143 = CARTESIAN_POINT ( 'NONE',  ( 18.92812500061451431, 4.541064518000418104, 2.621784821874999949 ) ) ;
#37144 = VERTEX_POINT ( 'NONE', #33952 ) ;
#37145 = CARTESIAN_POINT ( 'NONE',  ( 21.82499999999999574, 4.330127018922191873, 2.499999999999999556 ) ) ;
#37146 =( BOUNDED_CURVE ( )  B_SPLINE_CURVE ( 2, ( #46314, #63650, #36313, #53299, #19669, #46677, #2699 ),
 .UNSPECIFIED., .F., .F. ) 
 B_SPLINE_CURVE_WITH_KNOTS ( ( 3, 2, 2, 3 ),
 ( 0.9429157369121473620, 0.9444444444444444198, 0.9472222222222221877, 0.9486015587049059228 ),
 .UNSPECIFIED. ) 
 CURVE ( )  GEOMETRIC_REPRESENTATION_ITEM ( )  RATIONAL_B_SPLINE_CURVE ( ( 0.9336915734631608954, 0.9262691292263730558, 1.000000000000000000, 0.8660254037844387076, 1.000000000000000000, 0.9334734226073392316, 0.9330158706060402984 ) ) 
 REPRESENTATION_ITEM ( '' )  );
#37147 = CARTESIAN_POINT ( 'NONE',  ( 23.07187500061451857, 3.027376345333611329, 5.243569643749999010 ) ) ;
#37148 = EDGE_CURVE ( 'NONE', #5464, #3749, #26872, .T. ) ;
#37149 = ORIENTED_EDGE ( 'NONE', *, *, #23556, .T. ) ;
#37150 = CARTESIAN_POINT ( 'NONE',  ( 11.77500000000000036, 6.123233995736764310E-16, -4.999999999999998224 ) ) ;
#37151 = CARTESIAN_POINT ( 'NONE',  ( 13.07812500061451821, 4.541064518000418104, 2.621784821874999949 ) ) ;
#37152 = CARTESIAN_POINT ( 'NONE',  ( 3.553125000614516082, 4.541064518000418104, -2.621784821874998173 ) ) ;
#37153 = CARTESIAN_POINT ( 'NONE',  ( 15.83437500061451253, -2.746126346562646425, 4.756430356249996549 ) ) ;
#37154 = CARTESIAN_POINT ( 'NONE',  ( 27.06562500061451004, 3.027376345333611329, 5.243569643749999010 ) ) ;
#37155 = CARTESIAN_POINT ( 'NONE',  ( 19.53749999999999432, 5.773502691896255534, 3.535250795749688894E-16 ) ) ;
#37156 = CARTESIAN_POINT ( 'NONE',  ( 26.81250000000000000, 2.886751345948126879, 4.999999999999999112 ) ) ;
#37157 = CARTESIAN_POINT ( 'NONE',  ( 3.421875000614516882, -6.054752690667223547, -1.112240025338166033E-15 ) ) ;
#37158 = CARTESIAN_POINT ( 'NONE',  ( 7.471875000614519813, -6.054752690667223547, -1.112240025338166033E-15 ) ) ;
#37159 = CARTESIAN_POINT ( 'NONE',  ( 17.97187500061451715, 3.027376345333613106, -5.243569643749998122 ) ) ;
#37160 = DIRECTION ( 'NONE',  ( -1.000000000000000000, -0.000000000000000000, -0.000000000000000000 ) ) ;
#37161 = VERTEX_POINT ( 'NONE', #25414 ) ;
#37162 = CARTESIAN_POINT ( 'NONE',  ( 27.32812500061451644, 6.421520780324663323E-16, -5.243569643749999010 ) ) ;
#37163 = CARTESIAN_POINT ( 'NONE',  ( 27.27187500061451431, -6.054752690667223547, -1.112240025338166033E-15 ) ) ;
#37164 = FACE_OUTER_BOUND ( 'NONE', #38980, .T. ) ;
#37165 = CARTESIAN_POINT ( 'NONE',  ( 15.97499999999999964, 4.330127018922191873, 2.499999999999999556 ) ) ;
#37166 = CARTESIAN_POINT ( 'NONE',  ( 10.41562500061451679, 3.027376345333611329, 5.243569643749999010 ) ) ;
#37167 = CARTESIAN_POINT ( 'NONE',  ( -3.999999999999997335, 15.08750000000000036, -27.69059892324149530 ) ) ;
#37168 = CARTESIAN_POINT ( 'NONE',  ( 45.00000000000000000, 0.000000000000000000, 4.999999999999998224 ) ) ;
#37169 = CARTESIAN_POINT ( 'NONE',  ( 29.57812500061451644, 6.421520780324663323E-16, -5.243569643749999010 ) ) ;
#37170 = CARTESIAN_POINT ( 'NONE',  ( 18.07500000122903216, -5.773502691896255534, -1.060575238724906372E-15 ) ) ;
#37171 = CARTESIAN_POINT ( 'NONE',  ( 3.065815551951259543, -3.949781639713015657, 3.065815551951216467 ) ) ;
#37172 = CARTESIAN_POINT ( 'NONE',  ( 17.48437500061451999, 5.824947211148865298E-16, -4.756430356249998326 ) ) ;
#37173 = CARTESIAN_POINT ( 'NONE',  ( 6.103125000614515905, -4.541064518000417216, -2.621784821875001281 ) ) ;
#37174 = CARTESIAN_POINT ( 'NONE',  ( 22.47187500061451715, 3.027376345333613106, -5.243569643749998122 ) ) ;
#37175 = ADVANCED_FACE ( 'NONE', ( #19863 ), #36498, .T. ) ;
#37176 = CARTESIAN_POINT ( 'NONE',  ( 2.121784821874999061, 17.45937500061451786, 26.32496088578401583 ) ) ;
#37177 = CARTESIAN_POINT ( 'NONE',  ( 24.19687500061451857, -3.027376345333610441, -5.243569643749999898 ) ) ;
#37178 = CARTESIAN_POINT ( 'NONE',  ( 3.975000000000002753, -4.330127018922194537, 2.499999999999995559 ) ) ;
#37179 = CARTESIAN_POINT ( 'NONE',  ( -2.000000000000000000, 10.58750000122903323, 26.53589838486224650 ) ) ;
#37180 = CARTESIAN_POINT ( 'NONE',  ( 11.16562500061451679, 3.027376345333613106, -5.243569643749998122 ) ) ;
#37181 = CARTESIAN_POINT ( 'NONE',  ( 3.262500001229035718, -4.330127018922190985, -2.500000000000001332 ) ) ;
#37182 = CARTESIAN_POINT ( 'NONE',  ( 9.159375000614515372, 0.000000000000000000, 5.243569643749999010 ) ) ;
#37183 = DIRECTION ( 'NONE',  ( 0.000000000000000000, 0.000000000000000000, 1.000000000000000000 ) ) ;
#37184 = AXIS2_PLACEMENT_3D ( 'NONE', #39023, #49012, #38658 ) ;
#37185 = CARTESIAN_POINT ( 'NONE',  ( 9.778125000614517504, 6.421520780324663323E-16, -5.243569643749999010 ) ) ;
#37186 = CARTESIAN_POINT ( 'NONE',  ( 14.40937500061451715, 4.541064518000418104, -2.621784821874998173 ) ) ;
#37187 = CARTESIAN_POINT ( 'NONE',  ( 4.898587196589411843E-16, 20.00000000000000000, 33.99999999999999289 ) ) ;
#37188 = CARTESIAN_POINT ( 'NONE',  ( 22.57500000122903572, -5.773502691896255534, -1.060575238724906372E-15 ) ) ;
#37189 = CARTESIAN_POINT ( 'NONE',  ( 9.421875000614519990, 3.027376345333613106, -5.243569643749998122 ) ) ;
#37190 = CARTESIAN_POINT ( 'NONE',  ( 12.81562500061451537, -6.054752690667223547, -1.112240025338166033E-15 ) ) ;
#37191 = CARTESIAN_POINT ( 'NONE',  ( 27.76875000122903003, 2.886751345948126879, 4.999999999999999112 ) ) ;
#37192 = CARTESIAN_POINT ( 'NONE',  ( 20.59687500061451360, -3.027376345333610441, -5.243569643749999898 ) ) ;
#37193 = CARTESIAN_POINT ( 'NONE',  ( 26.68125000122903145, 6.123233995736764310E-16, -4.999999999999998224 ) ) ;
#37194 = CIRCLE ( 'NONE', #46627, 1.500000000000000444 ) ;
#37195 = CARTESIAN_POINT ( 'NONE',  ( -3.999999999999999112, 12.01250000122903394, -30.00000000000000000 ) ) ;
#37196 = CARTESIAN_POINT ( 'NONE',  ( -5.000000000000004441, 0.000000000000000000, 4.999999999999998224 ) ) ;
#37197 = CARTESIAN_POINT ( 'NONE',  ( -2.121784821874996840, 14.08437500061451786, -26.32496088578401583 ) ) ;
#37198 = CARTESIAN_POINT ( 'NONE',  ( 14.13750000122903394, 6.123233995736764310E-16, -4.999999999999998224 ) ) ;
#37199 = CARTESIAN_POINT ( 'NONE',  ( 9.834375000614517859, 6.421520780324663323E-16, -5.243569643749999010 ) ) ;
#37200 = CARTESIAN_POINT ( 'NONE',  ( 4.243569643749999898, 16.84062500061451573, -27.54997392385601529 ) ) ;
#37201 = CARTESIAN_POINT ( 'NONE',  ( 17.81250000122903288, 4.330127018922192761, -2.499999999999997780 ) ) ;
#37202 = CARTESIAN_POINT ( 'NONE',  ( 11.80312500061451608, 0.000000000000000000, 5.243569643749999010 ) ) ;
#37203 = ORIENTED_EDGE ( 'NONE', *, *, #51099, .T. ) ;
#37204 = VECTOR ( 'NONE', #21763, 1000.000000000000000 ) ;
#37205 = CARTESIAN_POINT ( 'NONE',  ( 16.35000000000000142, 4.330127018922192761, -2.499999999999997780 ) ) ;
#37206 = DIRECTION ( 'NONE',  ( 0.000000000000000000, 0.000000000000000000, 1.000000000000000000 ) ) ;
#37207 = CARTESIAN_POINT ( 'NONE',  ( 10.35937500061451644, 4.541064518000418104, -2.621784821874998173 ) ) ;
#37208 = LINE ( 'NONE', #9138, #29153 ) ;
#37209 = CARTESIAN_POINT ( 'NONE',  ( 11.43750000122903465, 6.123233995736764310E-16, -4.999999999999998224 ) ) ;
#37210 = CARTESIAN_POINT ( 'NONE',  ( 20.77500000122903145, -5.773502691896255534, -1.060575238724906372E-15 ) ) ;
#37211 = CARTESIAN_POINT ( 'NONE',  ( 16.97812500061451502, 6.421520780324663323E-16, -5.243569643749999010 ) ) ;
#37212 = CARTESIAN_POINT ( 'NONE',  ( 21.51562500061451644, 3.027376345333613106, -5.243569643749998122 ) ) ;
#37213 = CARTESIAN_POINT ( 'NONE',  ( 27.00000000122903288, -2.886751345948129988, 4.999999999999997335 ) ) ;
#37214 =( BOUNDED_CURVE ( )  B_SPLINE_CURVE ( 2, ( #71180, #43110, #66006, #49389, #39770, #22031, #39397 ),
 .UNSPECIFIED., .F., .F. ) 
 B_SPLINE_CURVE_WITH_KNOTS ( ( 3, 2, 2, 3 ),
 ( 0.9939769717443815988, 0.9944444444444444642, 0.9972222222222222321, 0.9976335333330554889 ),
 .UNSPECIFIED. ) 
 CURVE ( )  GEOMETRIC_REPRESENTATION_ITEM ( )  RATIONAL_B_SPLINE_CURVE ( ( 0.9624955293375538901, 0.9774533921562205130, 1.000000000000000000, 0.8660254037844387076, 1.000000000000000000, 0.9801621136025704395, 0.9661990982304526909 ) ) 
 REPRESENTATION_ITEM ( '' )  );
#37215 = CARTESIAN_POINT ( 'NONE',  ( 3.328125000614516438, -4.541064518000419881, 2.621784821874995952 ) ) ;
#37216 = CARTESIAN_POINT ( 'NONE',  ( 25.76249999999999929, 2.886751345948129099, -4.999999999999998224 ) ) ;
#37217 = CYLINDRICAL_SURFACE ( 'NONE', #11220, 4.999999999999998224 ) ;
#37218 = CARTESIAN_POINT ( 'NONE',  ( 29.09999999999999787, 0.000000000000000000, 4.999999999999998224 ) ) ;
#37219 = CARTESIAN_POINT ( 'NONE',  ( 28.73437500061451644, 6.421520780324663323E-16, -5.243569643749999010 ) ) ;
#37220 = DIRECTION ( 'NONE',  ( 0.000000000000000000, 0.000000000000000000, -1.000000000000000000 ) ) ;
#37221 = CARTESIAN_POINT ( 'NONE',  ( 4.725000001229034297, 2.886751345948129099, -4.999999999999998224 ) ) ;
#37222 = CARTESIAN_POINT ( 'NONE',  ( 3.525000000000000355, -4.330127018922194537, 2.499999999999995559 ) ) ;
#37223 = CARTESIAN_POINT ( 'NONE',  ( 7.546875000614517326, -3.027376345333610441, -5.243569643749999898 ) ) ;
#37224 = CARTESIAN_POINT ( 'NONE',  ( 25.60312500061451502, 4.541064518000418104, -2.621784821874998173 ) ) ;
#37225 = CARTESIAN_POINT ( 'NONE',  ( 3.756430356249998770, 13.16562499938548392, 32.16877607737301759 ) ) ;
#37226 = CARTESIAN_POINT ( 'NONE',  ( -1.004196803065525945, 9.951383199219650422, -24.08129654815694920 ) ) ;
#37227 = VECTOR ( 'NONE', #43181, 1000.000000000000000 ) ;
#37228 = CARTESIAN_POINT ( 'NONE',  ( 22.01250000122903216, 0.000000000000000000, 4.999999999999998224 ) ) ;
#37229 = CARTESIAN_POINT ( 'NONE',  ( 4.584375000614516971, 4.541064518000418104, 2.621784821874999949 ) ) ;
#37230 = CARTESIAN_POINT ( 'NONE',  ( 8.484375000614518214, 6.421520780324663323E-16, -5.243569643749999010 ) ) ;
#37231 = CARTESIAN_POINT ( 'NONE',  ( 3.525000000000000355, -4.330127018922194537, 2.499999999999995559 ) ) ;
#37232 = VECTOR ( 'NONE', #50274, 1000.000000000000000 ) ;
#37233 = CARTESIAN_POINT ( 'NONE',  ( 9.001249775931846008E-16, 11.36562500061459602, 34.90005215228797653 ) ) ;
#37234 = CARTESIAN_POINT ( 'NONE',  ( 20.77500000122903145, -5.773502691896255534, -1.060575238724906372E-15 ) ) ;
#37235 = CARTESIAN_POINT ( 'NONE',  ( 3.862500000000001155, 2.886751345948126879, 4.999999999999999112 ) ) ;
#37237 = EDGE_CURVE ( 'NONE', #22838, #30519, #42416, .T. ) ;
#37236 = AXIS2_PLACEMENT_3D ( 'NONE', #24511, #70672, #40796 ) ;
#37238 = CARTESIAN_POINT ( 'NONE',  ( 16.05937500061451573, 2.746126346562645981, -4.756430356249997438 ) ) ;
#37239 = ORIENTED_EDGE ( 'NONE', *, *, #42756, .T. ) ;
#37240 = CARTESIAN_POINT ( 'NONE',  ( 19.26562500061451644, 3.027376345333613106, -5.243569643749998122 ) ) ;
#37241 = CARTESIAN_POINT ( 'NONE',  ( 10.82812500061451644, 4.541064518000418104, 2.621784821874999949 ) ) ;
#37242 = CARTESIAN_POINT ( 'NONE',  ( 24.90937500061451004, -5.492252693125287522, -1.008910452111647106E-15 ) ) ;
#37243 = CARTESIAN_POINT ( 'NONE',  ( 7.696875000614516793, 6.054752690667223547, 3.707466751127219781E-16 ) ) ;
#37244 = CARTESIAN_POINT ( 'NONE',  ( 24.44999999999999929, 4.330127018922192761, -2.499999999999997780 ) ) ;
#37245 = CARTESIAN_POINT ( 'NONE',  ( 20.25000000122903288, -2.886751345948129988, 4.999999999999997335 ) ) ;
#37246 = CARTESIAN_POINT ( 'NONE',  ( 27.74062500061451431, -3.027376345333610441, -5.243569643749999898 ) ) ;
#37247 = CARTESIAN_POINT ( 'NONE',  ( 15.48749999999999893, 5.773502691896255534, 3.535250795749688401E-16 ) ) ;
#37248 = CARTESIAN_POINT ( 'NONE',  ( 9.534375000614517148, 4.541064518000418104, 2.621784821874999949 ) ) ;
#37249 = CARTESIAN_POINT ( 'NONE',  ( 13.39687500061451608, -3.027376345333610441, -5.243569643749999898 ) ) ;
#37250 = CARTESIAN_POINT ( 'NONE',  ( 24.68437500061451573, 6.421520780324663323E-16, -5.243569643749999010 ) ) ;
#37251 = DIRECTION ( 'NONE',  ( 0.000000000000000000, 1.000000000000000000, -8.673617379884036705E-17 ) ) ;
#37252 = CARTESIAN_POINT ( 'NONE',  ( 12.71250000000000036, 2.886751345948129099, -4.999999999999998224 ) ) ;
#37253 = CARTESIAN_POINT ( 'NONE',  ( 20.29687500061451644, 6.054752690667223547, 3.707466751127219781E-16 ) ) ;
#37254 = CARTESIAN_POINT ( 'NONE',  ( 8.521875000614516082, 3.027376345333613106, -5.243569643749998122 ) ) ;
#37255 = CARTESIAN_POINT ( 'NONE',  ( 3.756430356250000546, 20.44062499938547717, 27.83122392262697886 ) ) ;
#37256 = CARTESIAN_POINT ( 'NONE',  ( 22.50000000000000000, -4.330127018922190985, -2.500000000000001332 ) ) ;
#37257 = CARTESIAN_POINT ( 'NONE',  ( 4.000000000000000000, 13.85000000000000142, 30.00000000000000000 ) ) ;
#37258 = CARTESIAN_POINT ( 'NONE',  ( 29.81249999999999645, 2.886751345948139313, -4.999999999999980460 ) ) ;
#37259 = CARTESIAN_POINT ( 'NONE',  ( 25.77187500061451075, 2.746126346562643317, 4.756430356249998326 ) ) ;
#37260 = CARTESIAN_POINT ( 'NONE',  ( 11.80312500061451608, 0.000000000000000000, 5.243569643749999010 ) ) ;
#37261 = CARTESIAN_POINT ( 'NONE',  ( 5.587500000000003020, 5.773502691896255534, 3.535250795749688894E-16 ) ) ;
#37262 = CARTESIAN_POINT ( 'NONE',  ( 6.712500001229034119, 0.000000000000000000, 4.999999999999998224 ) ) ;
#37263 = CARTESIAN_POINT ( 'NONE',  ( 15.20625000122903181, 0.000000000000000000, 4.999999999999998224 ) ) ;
#37264 = CARTESIAN_POINT ( 'NONE',  ( 11.88749999999999751, 5.773502691896255534, 3.535250795749688894E-16 ) ) ;
#37265 = CARTESIAN_POINT ( 'NONE',  ( 3.999999999999998668, 17.22500000122903785, 27.69059892324149175 ) ) ;
#37266 = CARTESIAN_POINT ( 'NONE',  ( 11.25000000122903288, -2.886751345948129988, 4.999999999999997335 ) ) ;
#37267 = CARTESIAN_POINT ( 'NONE',  ( 21.72187500061451715, 3.027376345333611329, 5.243569643749999010 ) ) ;
#37268 = CARTESIAN_POINT ( 'NONE',  ( 15.94687500061451502, -3.027376345333614438, 5.243569643749998122 ) ) ;
#37269 = CARTESIAN_POINT ( 'NONE',  ( 7.331250001229031810, 6.123233995736764310E-16, -4.999999999999998224 ) ) ;
#37270 = ORIENTED_EDGE ( 'NONE', *, *, #63369, .T. ) ;
#37271 = CARTESIAN_POINT ( 'NONE',  ( 17.39062500061451644, -3.027376345333610441, -5.243569643749999898 ) ) ;
#37272 = CARTESIAN_POINT ( 'NONE',  ( 28.42500000122904069, -5.773502691896255534, -1.060575238724906372E-15 ) ) ;
#37273 = CARTESIAN_POINT ( 'NONE',  ( 17.52187500061451431, 3.027376345333613106, -5.243569643749998122 ) ) ;
#37274 = CARTESIAN_POINT ( 'NONE',  ( 28.35937500061451289, 4.541064518000418104, -2.621784821874998173 ) ) ;
#37275 = CARTESIAN_POINT ( 'NONE',  ( 3.965625000614515727, 3.027376345333613106, -5.243569643749998122 ) ) ;
#37276 = CARTESIAN_POINT ( 'NONE',  ( 19.19062500061452070, -3.027376345333610441, -5.243569643749999898 ) ) ;
#37277 = CARTESIAN_POINT ( 'NONE',  ( 28.20937500061451786, -4.541064518000417216, -2.621784821875001281 ) ) ;
#37278 = CARTESIAN_POINT ( 'NONE',  ( -2.121784821874996840, 12.67812500061451786, 33.67503911421598417 ) ) ;
#37279 = CARTESIAN_POINT ( 'NONE',  ( 17.73750000122903359, 6.123233995736764310E-16, -4.999999999999998224 ) ) ;
#37280 = CARTESIAN_POINT ( 'NONE',  ( 10.02187500061451964, 2.746126346562643317, 4.756430356249998326 ) ) ;
#37281 = CARTESIAN_POINT ( 'NONE',  ( 8.053125000614516082, 4.541064518000418104, -2.621784821874998173 ) ) ;
#37282 = CARTESIAN_POINT ( 'NONE',  ( 25.90312500061451573, -4.541064518000417216, -2.621784821875001281 ) ) ;
#37283 = CARTESIAN_POINT ( 'NONE',  ( 9.037499999999997868, -2.886751345948193048, -4.999999999999883649 ) ) ;
#37284 = CARTESIAN_POINT ( 'NONE',  ( 23.85937500061451644, 4.541064518000418104, -2.621784821874998173 ) ) ;
#37285 = CARTESIAN_POINT ( 'NONE',  ( 14.87812500061451537, 4.541064518000418104, 2.621784821874999949 ) ) ;
#37286 = CARTESIAN_POINT ( 'NONE',  ( 23.32500000122903572, 2.886751345948126879, 4.999999999999999112 ) ) ;
#37287 = CARTESIAN_POINT ( 'NONE',  ( 23.01562500061451644, 3.027376345333611329, 5.243569643749999010 ) ) ;
#37288 = CARTESIAN_POINT ( 'NONE',  ( 20.63437500061451857, 6.421520780324663323E-16, -5.243569643749999010 ) ) ;
#37289 = CARTESIAN_POINT ( 'NONE',  ( 13.07812500061451821, 4.541064518000418104, 2.621784821874999949 ) ) ;
#37290 = CARTESIAN_POINT ( 'NONE',  ( 4.243569643749999010, 14.72187500061451715, 27.54997392385601174 ) ) ;
#37291 = CARTESIAN_POINT ( 'NONE',  ( 20.91562500061451502, -6.054752690667223547, -1.112240025338166033E-15 ) ) ;
#37292 = CARTESIAN_POINT ( 'NONE',  ( 23.34375000122902577, -2.886751345948130876, 4.999999999999996447 ) ) ;
#37293 = ORIENTED_EDGE ( 'NONE', *, *, #70290, .F. ) ;
#37294 = ORIENTED_EDGE ( 'NONE', *, *, #39744, .T. ) ;
#37295 = CARTESIAN_POINT ( 'NONE',  ( 23.69999999999999929, 0.000000000000000000, 4.999999999999998224 ) ) ;
#37296 = CARTESIAN_POINT ( 'NONE',  ( 3.999999999999999112, 11.67500000000000071, -30.00000000000000000 ) ) ;
#37297 = CARTESIAN_POINT ( 'NONE',  ( 2.000000000000001332, 18.01250000122903572, 33.46410161513774995 ) ) ;
#37298 = CARTESIAN_POINT ( 'NONE',  ( 27.21562500061451928, -6.054752690667223547, -1.112240025338166033E-15 ) ) ;
#37299 = CARTESIAN_POINT ( 'NONE',  ( 5.090625000614516615, -3.027376345333614438, 5.243569643749998122 ) ) ;
#37300 = CARTESIAN_POINT ( 'NONE',  ( 20.06250000122903643, 4.330127018922192761, -2.499999999999997780 ) ) ;
#37301 = CARTESIAN_POINT ( 'NONE',  ( 25.75312500061451715, 0.000000000000000000, 5.243569643749999010 ) ) ;
#37302 = CARTESIAN_POINT ( 'NONE',  ( 21.93750000000000000, -2.886751345948129988, 4.999999999999997335 ) ) ;
#37303 = CARTESIAN_POINT ( 'NONE',  ( 28.30312500061451431, 4.541064518000418104, -2.621784821874998173 ) ) ;
#37304 = CARTESIAN_POINT ( 'NONE',  ( 7.940625000614518036, -3.027376345333610441, -5.243569643749999898 ) ) ;
#37305 = ORIENTED_EDGE ( 'NONE', *, *, #43499, .F. ) ;
#37306 = EDGE_CURVE ( 'NONE', #38366, #67359, #64593, .T. ) ;
#37307 = CARTESIAN_POINT ( 'NONE',  ( 22.30312500061451431, -4.541064518000417216, -2.621784821875001281 ) ) ;
#37308 = CARTESIAN_POINT ( 'NONE',  ( 5.915625000614515905, 3.027376345333611329, 5.243569643749999010 ) ) ;
#37309 = CARTESIAN_POINT ( 'NONE',  ( 12.94687500061451857, -2.746126346562642428, -4.756430356249999214 ) ) ;
#37310 = CARTESIAN_POINT ( 'NONE',  ( 4.040625000614517681, 6.054752690667223547, 3.707466751127219781E-16 ) ) ;
#37311 = CARTESIAN_POINT ( 'NONE',  ( 3.999999999999999112, 14.03750000122903430, -30.00000000000000000 ) ) ;
#37312 = CARTESIAN_POINT ( 'NONE',  ( 13.40625000122903288, 0.000000000000000000, 4.999999999999998224 ) ) ;
#37313 = CARTESIAN_POINT ( 'NONE',  ( 11.84999999999999964, 4.330127018922192761, -2.499999999999997780 ) ) ;
#37314 = CARTESIAN_POINT ( 'NONE',  ( 10.47187500061451715, 3.027376345333611329, 5.243569643749999010 ) ) ;
#37315 = CARTESIAN_POINT ( 'NONE',  ( 7.837500001229035007, 6.123233995736764310E-16, -4.999999999999998224 ) ) ;
#37316 = CARTESIAN_POINT ( 'NONE',  ( 14.18437500061451750, -4.541064518000419881, 2.621784821874995952 ) ) ;
#37317 = CARTESIAN_POINT ( 'NONE',  ( 15.67500000000000071, -4.330127018922194537, 2.499999999999995559 ) ) ;
#37318 = CARTESIAN_POINT ( 'NONE',  ( 5.971875000614516260, 3.027376345333611329, 5.243569643749999010 ) ) ;
#37319 = CARTESIAN_POINT ( 'NONE',  ( -1.473776270879187500, 9.816672227264547246, -34.04916702557058983 ) ) ;
#37320 = CARTESIAN_POINT ( 'NONE',  ( -1.243387493232115393E-14, 15.25624999877096499, 26.00000000000000000 ) ) ;
#37321 = ADVANCED_FACE ( 'NONE', ( #58288 ), #35766, .F. ) ;
#37322 = CARTESIAN_POINT ( 'NONE',  ( 12.68437500061451573, 4.541064518000418104, 2.621784821874999949 ) ) ;
#37323 = CARTESIAN_POINT ( 'NONE',  ( 3.678818219770688902, 3.386201399061161688, 4.003588590596459440 ) ) ;
#37324 = CARTESIAN_POINT ( 'NONE',  ( 22.86562500061451431, 3.027376345333613106, -5.243569643749998122 ) ) ;
#37325 = CARTESIAN_POINT ( 'NONE',  ( -2.121784821874999949, 9.884375000614518569, 26.32496088578401938 ) ) ;
#37326 = CARTESIAN_POINT ( 'NONE',  ( 4.243569643749999898, 18.67812500061459602, 30.00000000000000000 ) ) ;
#37327 = CARTESIAN_POINT ( 'NONE',  ( 24.98437500061451644, -4.541064518000419881, 2.621784821874995952 ) ) ;
#37328 = CARTESIAN_POINT ( 'NONE',  ( 30.00000000000000000, 0.000000000000000000, 0.000000000000000000 ) ) ;
#37329 = CARTESIAN_POINT ( 'NONE',  ( 4.865625000614517859, 3.027376345333613106, -5.243569643749998122 ) ) ;
#37330 = CARTESIAN_POINT ( 'NONE',  ( 22.62187500061451573, -4.119189519843968306, 2.378215178124996054 ) ) ;
#37331 = CARTESIAN_POINT ( 'NONE',  ( 13.43437500061451750, 6.421520780324663323E-16, -5.243569643749999010 ) ) ;
#37332 = CARTESIAN_POINT ( 'NONE',  ( 9.384375000614515017, 5.492252693125287522, 3.363034840372157021E-16 ) ) ;
#37333 = AXIS2_PLACEMENT_3D ( 'NONE', #5256, #16690, #5626 ) ;
#37334 = CARTESIAN_POINT ( 'NONE',  ( 28.08750000122903145, 6.123233995736764310E-16, -4.999999999999998224 ) ) ;
#37335 = CARTESIAN_POINT ( 'NONE',  ( 5.071875000614519458, 3.027376345333611329, 5.243569643749999010 ) ) ;
#37336 = CARTESIAN_POINT ( 'NONE',  ( 16.39687500061451786, -3.027376345333614438, 5.243569643749998122 ) ) ;
#37337 = CARTESIAN_POINT ( 'NONE',  ( -3.999999999999999112, 11.90000000000000036, 30.00000000000000000 ) ) ;
#37338 = CARTESIAN_POINT ( 'NONE',  ( 24.93750000000000355, 5.773502691896255534, 3.535250795749688894E-16 ) ) ;
#37339 = CARTESIAN_POINT ( 'NONE',  ( 4.087500001229035007, -4.330127018922194537, 2.499999999999995559 ) ) ;
#37340 = CARTESIAN_POINT ( 'NONE',  ( 28.32187500061451502, 3.027376345333613106, -5.243569643749998122 ) ) ;
#37341 = CARTESIAN_POINT ( 'NONE',  ( 1.878215178124997609, 14.02812499938548285, 33.25316411605952993 ) ) ;
#37342 = CARTESIAN_POINT ( 'NONE',  ( 29.62500000000000000, -4.330127018922194537, 2.499999999999995559 ) ) ;
#37343 = CARTESIAN_POINT ( 'NONE',  ( 7.762500000000001954, 2.886751345948129099, -4.999999999999998224 ) ) ;
#37344 = CARTESIAN_POINT ( 'NONE',  ( 9.646875000614514306, -4.119189519843965641, -2.378215178125001383 ) ) ;
#37345 = CARTESIAN_POINT ( 'NONE',  ( 21.36562500061451431, -6.054752690667223547, -1.112240025338166033E-15 ) ) ;
#37346 = CARTESIAN_POINT ( 'NONE',  ( 11.84999999999999964, 4.330127018922192761, -2.499999999999997780 ) ) ;
#37347 = ADVANCED_FACE ( 'NONE', ( #14686 ), #42049, .T. ) ;
#37348 = CARTESIAN_POINT ( 'NONE',  ( 4.415625000614518569, 3.027376345333613106, -5.243569643749998122 ) ) ;
#37349 = CARTESIAN_POINT ( 'NONE',  ( 20.51249999999999929, 2.886751345948126879, 4.999999999999999112 ) ) ;
#37350 = CARTESIAN_POINT ( 'NONE',  ( 18.02812500061451573, 4.541064518000418104, 2.621784821874999949 ) ) ;
#37351 = CARTESIAN_POINT ( 'NONE',  ( -1.071796769724490783, 18.85490381179670649, 34.00000000000000000 ) ) ;
#37352 = CARTESIAN_POINT ( 'NONE',  ( 23.47500000122903430, -5.773502691896255534, -1.060575238724906372E-15 ) ) ;
#37353 = CARTESIAN_POINT ( 'NONE',  ( -7.967954043666661671E-16, 19.27812499938548640, 34.33755215474603517 ) ) ;
#37354 = CARTESIAN_POINT ( 'NONE',  ( 3.412500000000002309, 2.886751345948126879, 4.999999999999999112 ) ) ;
#37355 = ORIENTED_EDGE ( 'NONE', *, *, #17544, .F. ) ;
#37356 = CARTESIAN_POINT ( 'NONE',  ( 20.46562500061451928, -6.054752690667223547, -1.112240025338166033E-15 ) ) ;
#37357 = CARTESIAN_POINT ( 'NONE',  ( 24.02812500061451573, -4.541064518000419881, 2.621784821874995952 ) ) ;
#37358 = CARTESIAN_POINT ( 'NONE',  ( 24.27187500061452141, 3.027376345333613106, -5.243569643749998122 ) ) ;
#37359 = CARTESIAN_POINT ( 'NONE',  ( 9.337500000000000355, -2.886751345948129988, 4.999999999999997335 ) ) ;
#37360 = CARTESIAN_POINT ( 'NONE',  ( 12.32812500061451821, -4.541064518000419881, 2.621784821874995952 ) ) ;
#37361 = CARTESIAN_POINT ( 'NONE',  ( 25.67812500061451431, 4.541064518000418104, 2.621784821874999949 ) ) ;
#37362 = CARTESIAN_POINT ( 'NONE',  ( 17.03437500061451715, 6.421520780324663323E-16, -5.243569643749999010 ) ) ;
#37363 = CARTESIAN_POINT ( 'NONE',  ( 8.015625000614518214, 3.027376345333613106, -5.243569643749998122 ) ) ;
#37364 = CARTESIAN_POINT ( 'NONE',  ( 5.810221930991193690E-16, 14.80624999877096570, 26.00000000000000000 ) ) ;
#37365 = CARTESIAN_POINT ( 'NONE',  ( 2.226602359779148887, 9.807522476441999260, 25.29835638300850320 ) ) ;
#37366 = CARTESIAN_POINT ( 'NONE',  ( 23.77500000122903145, 2.886751345948126879, 4.999999999999999112 ) ) ;
#37367 = CARTESIAN_POINT ( 'NONE',  ( 19.88437500061451857, 4.119189519843966529, 2.378215178124999607 ) ) ;
#37368 = CARTESIAN_POINT ( 'NONE',  ( 15.17812500061451608, 6.421520780324663323E-16, -5.243569643749999010 ) ) ;
#37369 = CARTESIAN_POINT ( 'NONE',  ( 9.046875000614518214, 6.054752690667223547, 3.707466751127219781E-16 ) ) ;
#37370 = CARTESIAN_POINT ( 'NONE',  ( 7.846875000614518036, -3.027376345333614438, 5.243569643749998122 ) ) ;
#37371 = ORIENTED_EDGE ( 'NONE', *, *, #64830, .F. ) ;
#37372 = CARTESIAN_POINT ( 'NONE',  ( -6.275039685470489619E-15, 17.97500000122903074, 33.99999999999999289 ) ) ;
#37373 = CARTESIAN_POINT ( 'NONE',  ( 22.41562500061451502, 3.027376345333613106, -5.243569643749998122 ) ) ;
#37374 = CARTESIAN_POINT ( 'NONE',  ( 16.77187500061451786, 3.027376345333611329, 5.243569643749999010 ) ) ;
#37375 = CARTESIAN_POINT ( 'NONE',  ( 22.94062500061451715, 6.054752690667223547, 3.707466751127219781E-16 ) ) ;
#37376 = CARTESIAN_POINT ( 'NONE',  ( 3.999999999999998668, 13.06250000000000355, 27.69059892324149175 ) ) ;
#37377 = CARTESIAN_POINT ( 'NONE',  ( 28.19062500061451715, -3.027376345333610441, -5.243569643749999898 ) ) ;
#37378 = CARTESIAN_POINT ( 'NONE',  ( 8.062500001229034652, 0.000000000000000000, 4.999999999999998224 ) ) ;
#37379 = ORIENTED_EDGE ( 'NONE', *, *, #9276, .F. ) ;
#37380 = CARTESIAN_POINT ( 'NONE',  ( 29.25000000000000000, -4.330127018922190985, -2.500000000000001332 ) ) ;
#37381 = CARTESIAN_POINT ( 'NONE',  ( 1.999999999999998668, 17.15000000000000213, -33.46410161513775705 ) ) ;
#37382 = AXIS2_PLACEMENT_3D ( 'NONE', #25819, #64603, #71621 ) ;
#37383 = CARTESIAN_POINT ( 'NONE',  ( 25.12500000122903288, 2.886751345948126879, 4.999999999999999112 ) ) ;
#37384 = CARTESIAN_POINT ( 'NONE',  ( 1.878215178124997609, 16.27812499938548285, 33.25316411605952993 ) ) ;
#37385 = CARTESIAN_POINT ( 'NONE',  ( 6.834375000614518747, 4.541064518000418104, 2.621784821874999949 ) ) ;
#37386 = CARTESIAN_POINT ( 'NONE',  ( 15.36562500061451608, 3.027376345333611329, 5.243569643749999010 ) ) ;
#37387 = CARTESIAN_POINT ( 'NONE',  ( 7.771875000614516971, 3.027376345333611329, 5.243569643749999010 ) ) ;
#37388 = CARTESIAN_POINT ( 'NONE',  ( 27.33750000122903145, 4.330127018922191873, 2.499999999999999556 ) ) ;
#37389 = CARTESIAN_POINT ( 'NONE',  ( 17.89687500061451431, -3.027376345333610441, -5.243569643749999898 ) ) ;
#37390 = CARTESIAN_POINT ( 'NONE',  ( 5.671875000614519102, -6.054752690667223547, -1.112240025338166033E-15 ) ) ;
#37391 = CARTESIAN_POINT ( 'NONE',  ( 4.000000000000000000, 17.48750000000000071, -27.69059892324149885 ) ) ;
#37392 = CARTESIAN_POINT ( 'NONE',  ( 5.240625000614516971, -3.027376345333610441, -5.243569643749999898 ) ) ;
#37393 = CARTESIAN_POINT ( 'NONE',  ( 15.51562500061451644, -6.054752690667223547, -1.112240025338166033E-15 ) ) ;
#37394 = ORIENTED_EDGE ( 'NONE', *, *, #61111, .T. ) ;
#37395 = CARTESIAN_POINT ( 'NONE',  ( 12.77812500061451750, -4.541064518000419881, 2.621784821874995952 ) ) ;
#37396 = CARTESIAN_POINT ( 'NONE',  ( 6.600000001229032520, 5.773502691896255534, 3.535250795749688894E-16 ) ) ;
#37397 = CARTESIAN_POINT ( 'NONE',  ( 8.315625000614515372, -6.054752690667223547, -1.112240025338166033E-15 ) ) ;
#37398 = CARTESIAN_POINT ( 'NONE',  ( 19.99687500061451573, -2.746126346562646425, 4.756430356249996549 ) ) ;
#37399 = CARTESIAN_POINT ( 'NONE',  ( 8.437500000000000000, -2.886751345948129988, 4.999999999999997335 ) ) ;
#37400 = CARTESIAN_POINT ( 'NONE',  ( 3.712500001229034563, -4.330127018922190985, -2.500000000000001332 ) ) ;
#37401 = CARTESIAN_POINT ( 'NONE',  ( 18.22499999999999787, 4.330127018922191873, 2.499999999999999556 ) ) ;
#37402 = EDGE_CURVE ( 'NONE', #26902, #57550, #36331, .T. ) ;
#37403 = CARTESIAN_POINT ( 'NONE',  ( 18.60937500061451644, 0.000000000000000000, 5.243569643749999010 ) ) ;
#37404 = CARTESIAN_POINT ( 'NONE',  ( 15.60000000122903607, 5.773502691896255534, 3.535250795749688894E-16 ) ) ;
#37405 = CARTESIAN_POINT ( 'NONE',  ( 21.18749999999999645, -2.886751345948125991, -5.000000000000000000 ) ) ;
#37406 = CARTESIAN_POINT ( 'NONE',  ( 2.121784821874999061, 15.60312500061451857, -33.67503911421598417 ) ) ;
#37407 = CARTESIAN_POINT ( 'NONE',  ( -1.394453263437886801E-15, 19.66249999999999787, -26.00000000000000000 ) ) ;
#37408 = CYLINDRICAL_SURFACE ( 'NONE', #26507, 4.999999999999998224 ) ;
#37409 = DIRECTION ( 'NONE',  ( -1.000000000000000000, -0.000000000000000000, -0.000000000000000000 ) ) ;
#37410 = CARTESIAN_POINT ( 'NONE',  ( 28.30312500061451431, 4.541064518000418104, -2.621784821874998173 ) ) ;
#37411 =( LENGTH_UNIT ( ) NAMED_UNIT ( * ) SI_UNIT ( .MILLI., .METRE. ) );
#37412 = CARTESIAN_POINT ( 'NONE',  ( 29.60625000122903216, 0.000000000000000000, 4.999999999999998224 ) ) ;
#37413 = CARTESIAN_POINT ( 'NONE',  ( 15.60937500061451644, -4.541064518000417216, -2.621784821875001281 ) ) ;
#37414 = CARTESIAN_POINT ( 'NONE',  ( 28.49999999999999645, 4.330127018922192761, -2.499999999999997780 ) ) ;
#37415 = CARTESIAN_POINT ( 'NONE',  ( 11.80312500061451608, 0.000000000000000000, 5.243569643749999010 ) ) ;
#37416 = CARTESIAN_POINT ( 'NONE',  ( 29.37187500061451573, -4.119189519843968306, 2.378215178124996054 ) ) ;
#37417 = CARTESIAN_POINT ( 'NONE',  ( 24.72187500061451360, 3.027376345333613106, -5.243569643749998122 ) ) ;
#37418 = CARTESIAN_POINT ( 'NONE',  ( 17.14687500061451431, 0.000000000000000000, 4.756430356249998326 ) ) ;
#37419 = CARTESIAN_POINT ( 'NONE',  ( 8.278125000614515727, -4.541064518000419881, 2.621784821874995952 ) ) ;
#37420 = CARTESIAN_POINT ( 'NONE',  ( 12.72187500061451537, 3.027376345333611329, 5.243569643749999010 ) ) ;
#37421 = VERTEX_POINT ( 'NONE', #69756 ) ;
#37422 = CARTESIAN_POINT ( 'NONE',  ( 24.79687500061451999, 6.054752690667223547, 3.707466751127219781E-16 ) ) ;
#37423 = CARTESIAN_POINT ( 'NONE',  ( 28.30312500061451431, 4.541064518000418104, -2.621784821874998173 ) ) ;
#37424 = DIRECTION ( 'NONE',  ( -0.000000000000000000, -1.000000000000000000, -0.000000000000000000 ) ) ;
#37425 = CARTESIAN_POINT ( 'NONE',  ( 7.237500000000000711, -2.886751345948125991, -5.000000000000000000 ) ) ;
#37426 = CIRCLE ( 'NONE', #28008, 1.500000000000000444 ) ;
#37427 = CARTESIAN_POINT ( 'NONE',  ( 15.78750000122903430, -4.330127018922194537, 2.499999999999995559 ) ) ;
#37428 = CARTESIAN_POINT ( 'NONE',  ( 27.33750000122903145, 4.330127018922191873, 2.499999999999999556 ) ) ;
#37429 = CARTESIAN_POINT ( 'NONE',  ( 0.000000000000000000, 20.00000000000000000, 26.00000000000000000 ) ) ;
#37430 = VERTEX_POINT ( 'NONE', #41326 ) ;
#37431 = CARTESIAN_POINT ( 'NONE',  ( 15.78749999999999964, -2.886751345948125991, -5.000000000000000000 ) ) ;
#37432 = CARTESIAN_POINT ( 'NONE',  ( 20.06250000000000000, 2.886751345948126879, 4.999999999999999112 ) ) ;
#37433 = CARTESIAN_POINT ( 'NONE',  ( 10.30312500061451431, 4.541064518000418104, -2.621784821874998173 ) ) ;
#37434 =( BOUNDED_CURVE ( )  B_SPLINE_CURVE ( 2, ( #72876, #72143, #45165, #32620, #21522, #11179, #33703 ),
 .UNSPECIFIED., .F., .F. ) 
 B_SPLINE_CURVE_WITH_KNOTS ( ( 3, 2, 2, 3 ),
 ( 0.3999999999999999112, 0.4027777777777777346, 0.4055555555555555580, 0.4083333333333333814 ),
 .UNSPECIFIED. ) 
 CURVE ( )  GEOMETRIC_REPRESENTATION_ITEM ( )  RATIONAL_B_SPLINE_CURVE ( ( 1.000000000000005329, 0.8660254037844333785, 1.000000000000000000, 0.8660254037844387076, 1.000000000000000000, 0.8660254037844360431, 1.000000000000002665 ) ) 
 REPRESENTATION_ITEM ( '' )  );
#37435 = ORIENTED_EDGE ( 'NONE', *, *, #73023, .T. ) ;
#37436 = CARTESIAN_POINT ( 'NONE',  ( 3.675000001229035362, -5.773502691896255534, -1.060575238724906372E-15 ) ) ;
#37437 = CARTESIAN_POINT ( 'NONE',  ( 9.001249775931846008E-16, 17.27187500061451786, -25.09994784771203058 ) ) ;
#37438 = CARTESIAN_POINT ( 'NONE',  ( 3.853125000614517681, -4.541064518000417216, -2.621784821875001281 ) ) ;
#37439 = CARTESIAN_POINT ( 'NONE',  ( 3.756430356250000102, 13.54062499938548392, 30.00000000000000000 ) ) ;
#37440 = CARTESIAN_POINT ( 'NONE',  ( 10.61250000000000071, 2.886751345948126879, 4.999999999999999112 ) ) ;
#37441 = CARTESIAN_POINT ( 'NONE',  ( 3.366080804335946919, -3.697228694398128290, 3.718268762498968094 ) ) ;
#37442 = EDGE_LOOP ( 'NONE', ( #44092, #38775, #21908, #17872 ) ) ;
#37443 = CARTESIAN_POINT ( 'NONE',  ( 4.243569643749999898, 14.17812500061451608, 30.00000000000000000 ) ) ;
#37444 = CARTESIAN_POINT ( 'NONE',  ( 27.40312500061451573, 4.541064518000418104, -2.621784821874998173 ) ) ;
#37445 = CARTESIAN_POINT ( 'NONE',  ( 29.21250000122903145, 0.000000000000000000, 4.999999999999998224 ) ) ;
#37446 = CARTESIAN_POINT ( 'NONE',  ( -1.878215178125001827, 18.79062499938548214, 33.25316411605952283 ) ) ;
#37447 = CARTESIAN_POINT ( 'NONE',  ( 23.33437500061451786, 6.421520780324663323E-16, -5.243569643749999010 ) ) ;
#37448 = CARTESIAN_POINT ( 'NONE',  ( 18.06562500061451715, 3.027376345333611329, 5.243569643749999010 ) ) ;
#37449 = EDGE_CURVE ( 'NONE', #11892, #2226, #31593, .T. ) ;
#37450 = CARTESIAN_POINT ( 'NONE',  ( 4.243569643749999898, 12.82812500061459460, -30.00000000000000000 ) ) ;
#37451 = CARTESIAN_POINT ( 'NONE',  ( 24.00000000122902932, -2.886751345948125991, -5.000000000000000000 ) ) ;
#37452 = CARTESIAN_POINT ( 'NONE',  ( 3.403125000614518836, -4.541064518000417216, -2.621784821875001281 ) ) ;
#37453 = CARTESIAN_POINT ( 'NONE',  ( 26.18437500061451573, 4.119189519843966529, 2.378215178124999607 ) ) ;
#37454 = CARTESIAN_POINT ( 'NONE',  ( 22.15312500061451573, 0.000000000000000000, 5.243569643749999010 ) ) ;
#37455 = CARTESIAN_POINT ( 'NONE',  ( 8.971875000614515372, 2.746126346562645981, -4.756430356249997438 ) ) ;
#37456 = CARTESIAN_POINT ( 'NONE',  ( 3.756430356250000102, 17.14062499938548356, 30.00000000000000000 ) ) ;
#37457 = CARTESIAN_POINT ( 'NONE',  ( 14.74687500061451573, -3.027376345333610441, -5.243569643749999898 ) ) ;
#37458 = CARTESIAN_POINT ( 'NONE',  ( 17.89687500061451431, -3.027376345333610441, -5.243569643749999898 ) ) ;
#37459 = CARTESIAN_POINT ( 'NONE',  ( 24.72187500061451360, 3.027376345333613106, -5.243569643749998122 ) ) ;
#37460 = CARTESIAN_POINT ( 'NONE',  ( 4.243569643749999010, 13.82187500061451857, 27.54997392385601174 ) ) ;
#37461 = CARTESIAN_POINT ( 'NONE',  ( 5.203125000614518214, -4.541064518000417216, -2.621784821875001281 ) ) ;
#37462 = CARTESIAN_POINT ( 'NONE',  ( 27.77812500061451573, 6.421520780324663323E-16, -5.243569643749999010 ) ) ;
#37463 = CARTESIAN_POINT ( 'NONE',  ( 29.42812500061451431, -4.541064518000419881, 2.621784821874995952 ) ) ;
#37464 = CARTESIAN_POINT ( 'NONE',  ( 1.626862140677534273E-15, 16.17500000122903359, -26.00000000000000355 ) ) ;
#37465 = CARTESIAN_POINT ( 'NONE',  ( -3.999999999999999112, 19.55000000000000071, 30.00000000000000000 ) ) ;
#37466 = CARTESIAN_POINT ( 'NONE',  ( 7.621875000614519280, 3.027376345333613106, -5.243569643749998122 ) ) ;
#37467 = CARTESIAN_POINT ( 'NONE',  ( 14.96250000122903323, -4.330127018922190985, -2.500000000000001332 ) ) ;
#37468 = CARTESIAN_POINT ( 'NONE',  ( 8.662500001229034297, -4.330127018922190985, -2.500000000000001332 ) ) ;
#37469 = CARTESIAN_POINT ( 'NONE',  ( 4.753125000614515372, -4.541064518000417216, -2.621784821875001281 ) ) ;
#37470 = CARTESIAN_POINT ( 'NONE',  ( -8.484601909799255319E-16, 15.03124999877096535, 34.61880215351700940 ) ) ;
#37471 = CARTESIAN_POINT ( 'NONE',  ( 21.09375000122903288, -2.886751345948129988, 4.999999999999997335 ) ) ;
#37472 = CARTESIAN_POINT ( 'NONE',  ( 14.37187500061451928, 3.027376345333613106, -5.243569643749998122 ) ) ;
#37473 = CARTESIAN_POINT ( 'NONE',  ( 21.39375000122903359, 5.773502691896255534, 3.535250795749688401E-16 ) ) ;
#37474 = VERTEX_POINT ( 'NONE', #70486 ) ;
#37475 = CARTESIAN_POINT ( 'NONE',  ( 21.51562500061451644, 3.027376345333613106, -5.243569643749998122 ) ) ;
#37476 = CARTESIAN_POINT ( 'NONE',  ( 6.590625000614518392, -3.027376345333610441, -5.243569643749999898 ) ) ;
#37477 = CARTESIAN_POINT ( 'NONE',  ( 24.49687500061451573, -3.027376345333614438, 5.243569643749998122 ) ) ;
#37478 = CARTESIAN_POINT ( 'NONE',  ( 6.740625000614516082, 6.054752690667223547, 3.707466751127219781E-16 ) ) ;
#37479 = CARTESIAN_POINT ( 'NONE',  ( 45.00000000000000000, 0.000000000000000000, 4.999999999999998224 ) ) ;
#37480 = CARTESIAN_POINT ( 'NONE',  ( 7.312500001229033764, -4.330127018922190985, -2.500000000000001332 ) ) ;
#37481 = CARTESIAN_POINT ( 'NONE',  ( 22.64062500061451644, -3.027376345333614438, 5.243569643749998122 ) ) ;
#37482 = CARTESIAN_POINT ( 'NONE',  ( -4.243569643749997233, 10.39062500061451644, -27.54997392385601174 ) ) ;
#37483 = CARTESIAN_POINT ( 'NONE',  ( 10.16250000122903252, 4.330127018922192761, -2.499999999999997780 ) ) ;
#37484 = CARTESIAN_POINT ( 'NONE',  ( 19.34062500061451573, 6.054752690667223547, 3.707466751127219781E-16 ) ) ;
#37485 = CARTESIAN_POINT ( 'NONE',  ( 18.92812500061451431, 4.541064518000418104, 2.621784821874999949 ) ) ;
#37486 = CARTESIAN_POINT ( 'NONE',  ( 28.80937500061451573, 4.119189519843966529, -2.378215178124998275 ) ) ;
#37487 = CARTESIAN_POINT ( 'NONE',  ( 18.86249999999999716, -5.773502691896255534, -1.060575238724906372E-15 ) ) ;
#37488 = CARTESIAN_POINT ( 'NONE',  ( 10.61250000122903536, 4.330127018922192761, -2.499999999999997780 ) ) ;
#37489 = AXIS2_PLACEMENT_3D ( 'NONE', #11376, #17981, #61974 ) ;
#37490 = CARTESIAN_POINT ( 'NONE',  ( 8.653125000614515727, 0.000000000000000000, 5.243569643749999010 ) ) ;
#37491 = CARTESIAN_POINT ( 'NONE',  ( 11.69062500061451360, 6.054752690667223547, 3.707466751127219781E-16 ) ) ;
#37492 = CARTESIAN_POINT ( 'NONE',  ( 22.31250000122903288, 4.330127018922192761, -2.499999999999997780 ) ) ;
#37493 = CARTESIAN_POINT ( 'NONE',  ( 22.32187500061451502, -6.054752690667223547, -1.112240025338166033E-15 ) ) ;
#37494 = CARTESIAN_POINT ( 'NONE',  ( 22.10625000122903216, -4.330127018922190985, -2.500000000000001332 ) ) ;
#37495 = CARTESIAN_POINT ( 'NONE',  ( 4.837500001229035895, 4.330127018922191873, 2.499999999999999556 ) ) ;
#37496 = CARTESIAN_POINT ( 'NONE',  ( 5.934375000614517504, 4.541064518000418104, 2.621784821874999949 ) ) ;
#37497 = CARTESIAN_POINT ( 'NONE',  ( 22.43437500061451573, 6.421520780324663323E-16, -5.243569643749999010 ) ) ;
#37498 = CARTESIAN_POINT ( 'NONE',  ( 21.78750000122903074, 6.123233995736764310E-16, -4.999999999999998224 ) ) ;
#37499 = CARTESIAN_POINT ( 'NONE',  ( 19.26562500061451644, 3.027376345333613106, -5.243569643749998122 ) ) ;
#37500 = CARTESIAN_POINT ( 'NONE',  ( 25.28437500061451715, 4.541064518000418104, 2.621784821874999949 ) ) ;
#37501 = CARTESIAN_POINT ( 'NONE',  ( 2.655984681222220721E-16, 20.06562499938548427, 25.66244784525396483 ) ) ;
#37502 = CARTESIAN_POINT ( 'NONE',  ( -3.137519842735245283E-14, 11.22500000122903430, -26.00000000000000711 ) ) ;
#37503 = CARTESIAN_POINT ( 'NONE',  ( -2.000000000000000000, 13.28750000122903430, -33.46410161513775705 ) ) ;
#37504 = CARTESIAN_POINT ( 'NONE',  ( 5.071875000614519458, 3.027376345333611329, 5.243569643749999010 ) ) ;
#37505 = CARTESIAN_POINT ( 'NONE',  ( 15.70312500061451644, 4.541064518000418104, -2.621784821874998173 ) ) ;
#37506 = CARTESIAN_POINT ( 'NONE',  ( 13.80937500061451750, -4.541064518000417216, -2.621784821875001281 ) ) ;
#37507 = ORIENTED_EDGE ( 'NONE', *, *, #60732, .T. ) ;
#37508 = CARTESIAN_POINT ( 'NONE',  ( 9.187500000000001776, 5.773502691896255534, 3.535250795749688401E-16 ) ) ;
#37509 = CARTESIAN_POINT ( 'NONE',  ( 23.95312500061451289, 0.000000000000000000, 5.243569643749999010 ) ) ;
#37510 = CARTESIAN_POINT ( 'NONE',  ( -1.487416814333745711E-14, 16.96250000000000213, 34.00000000000000000 ) ) ;
#37511 = CARTESIAN_POINT ( 'NONE',  ( -1.071796769724491005, 11.47009619066136565, -34.00000000000000000 ) ) ;
#37512 = CARTESIAN_POINT ( 'NONE',  ( 15.11249999999999893, 2.886751345948126879, 4.999999999999999112 ) ) ;
#37513 = CARTESIAN_POINT ( 'NONE',  ( 23.43750000122902932, -4.330127018922194537, 2.499999999999995559 ) ) ;
#37514 = CARTESIAN_POINT ( 'NONE',  ( 17.95312500061451644, 4.541064518000418104, -2.621784821874998173 ) ) ;
#37515 = ORIENTED_EDGE ( 'NONE', *, *, #35397, .F. ) ;
#37516 = CARTESIAN_POINT ( 'NONE',  ( 21.89999999999999858, 0.000000000000000000, 4.999999999999998224 ) ) ;
#37517 = CARTESIAN_POINT ( 'NONE',  ( 24.68437500061451573, 6.421520780324663323E-16, -5.243569643749999010 ) ) ;
#37518 = ORIENTED_EDGE ( 'NONE', *, *, #26233, .T. ) ;
#37519 = CYLINDRICAL_SURFACE ( 'NONE', #6511, 4.999999999999998224 ) ;
#37520 = CARTESIAN_POINT ( 'NONE',  ( 10.56562500061451715, -6.054752690667223547, -1.112240025338166033E-15 ) ) ;
#37521 = CARTESIAN_POINT ( 'NONE',  ( 4.040625000614517681, 6.054752690667223547, 3.707466751127219781E-16 ) ) ;
#37522 = CARTESIAN_POINT ( 'NONE',  ( 13.58437500061451431, -2.746126346562646425, 4.756430356249996549 ) ) ;
#37523 = CARTESIAN_POINT ( 'NONE',  ( 27.59062500061451573, -3.027376345333614438, 5.243569643749998122 ) ) ;
#37524 = CARTESIAN_POINT ( 'NONE',  ( 18.14999999999999858, 4.330127018922192761, -2.499999999999997780 ) ) ;
#37525 = CARTESIAN_POINT ( 'NONE',  ( 27.63749999999999929, 5.773502691896255534, 3.535250795749688894E-16 ) ) ;
#37526 = CARTESIAN_POINT ( 'NONE',  ( 1.999999999999997335, 14.16874999877096641, 33.46410161513775705 ) ) ;
#37527 = CARTESIAN_POINT ( 'NONE',  ( 6.459375000614518747, 0.000000000000000000, 5.243569643749999010 ) ) ;
#37528 = CARTESIAN_POINT ( 'NONE',  ( 17.48437500061451999, 6.421520780324663323E-16, -5.243569643749999010 ) ) ;
#37529 = ORIENTED_EDGE ( 'NONE', *, *, #61088, .T. ) ;
#37530 = CARTESIAN_POINT ( 'NONE',  ( 25.37812500061451715, -4.541064518000419881, 2.621784821874995952 ) ) ;
#37531 = CARTESIAN_POINT ( 'NONE',  ( 26.97187500061451360, 3.027376345333613106, -5.243569643749998122 ) ) ;
#37532 = CARTESIAN_POINT ( 'NONE',  ( -1.071796769724492115, 15.01115380933863186, 34.00000000000000000 ) ) ;
#37533 = CARTESIAN_POINT ( 'NONE',  ( 14.36249999999999893, -5.773502691896255534, -1.060575238724906372E-15 ) ) ;
#37534 = CARTESIAN_POINT ( 'NONE',  ( 11.87812500061451537, -4.541064518000419881, 2.621784821874995952 ) ) ;
#37535 = CARTESIAN_POINT ( 'NONE',  ( 16.50000000000000000, 0.000000000000000000, 4.999999999999998224 ) ) ;
#37536 = CARTESIAN_POINT ( 'NONE',  ( 14.21249999999999858, 2.886751345948238789, 4.999999999999807265 ) ) ;
#37537 = CARTESIAN_POINT ( 'NONE',  ( 28.52812500061451573, -4.541064518000419881, 2.621784821874995952 ) ) ;
#37538 = CARTESIAN_POINT ( 'NONE',  ( 15.22500000122903252, 2.886751345948126879, 4.999999999999999112 ) ) ;
#37539 = CARTESIAN_POINT ( 'NONE',  ( 8.606250001229033941, -4.330127018922190985, -2.500000000000001332 ) ) ;
#37540 = CARTESIAN_POINT ( 'NONE',  ( 18.57187500061451857, 2.746126346562643317, 4.756430356249998326 ) ) ;
#37541 = CARTESIAN_POINT ( 'NONE',  ( 4.678125000614516971, -4.541064518000419881, 2.621784821874995952 ) ) ;
#37542 = CARTESIAN_POINT ( 'NONE',  ( 21.34687500061451715, -3.027376345333614438, 5.243569643749998122 ) ) ;
#37543 = CARTESIAN_POINT ( 'NONE',  ( 2.121784821875001281, 18.20937500061451786, 33.67503911421598417 ) ) ;
#37544 = CARTESIAN_POINT ( 'NONE',  ( 23.14687500061451786, -3.027376345333614438, 5.243569643749998122 ) ) ;
#37545 = CARTESIAN_POINT ( 'NONE',  ( 4.462500000000001243, -5.773502691896255534, -1.060575238724906372E-15 ) ) ;
#37546 = CARTESIAN_POINT ( 'NONE',  ( -3.999999999999999556, 11.52500000122903501, 27.69059892324149530 ) ) ;
#37547 = CARTESIAN_POINT ( 'NONE',  ( 12.29062500061451857, -3.027376345333614438, 5.243569643749998122 ) ) ;
#37548 = CARTESIAN_POINT ( 'NONE',  ( 5.250000001229035540, 5.773502691896255534, 3.535250795749688894E-16 ) ) ;
#37549 = CARTESIAN_POINT ( 'NONE',  ( 10.50937500061451679, 0.000000000000000000, 5.243569643749999010 ) ) ;
#37550 = CARTESIAN_POINT ( 'NONE',  ( 11.21250000122903501, 0.000000000000000000, 4.999999999999998224 ) ) ;
#37551 = CARTESIAN_POINT ( 'NONE',  ( 9.590625000614517504, -3.027376345333614438, 5.243569643749998122 ) ) ;
#37552 = CARTESIAN_POINT ( 'NONE',  ( 14.93437500061451750, 4.541064518000418104, 2.621784821874999949 ) ) ;
#37553 = CARTESIAN_POINT ( 'NONE',  ( 25.50000000000000000, 0.000000000000000000, 4.999999999999998224 ) ) ;
#37554 = CARTESIAN_POINT ( 'NONE',  ( 20.47500000122903074, 2.886751345948129099, -4.999999999999998224 ) ) ;
#37555 = CARTESIAN_POINT ( 'NONE',  ( 10.80937500061451928, 4.541064518000418104, -2.621784821874998173 ) ) ;
#37556 = CARTESIAN_POINT ( 'NONE',  ( 12.74062500061451786, -3.027376345333614438, 5.243569643749998122 ) ) ;
#37557 = CARTESIAN_POINT ( 'NONE',  ( 29.00625000122903074, 4.330127018922192761, -2.499999999999997780 ) ) ;
#37558 = CARTESIAN_POINT ( 'NONE',  ( 20.85937500061451644, 0.000000000000000000, 5.243569643749999010 ) ) ;
#37559 = CARTESIAN_POINT ( 'NONE',  ( 25.46250000122903501, 4.330127018922192761, -2.499999999999997780 ) ) ;
#37560 = CARTESIAN_POINT ( 'NONE',  ( -1.090676731616020634, 4.887066358488520557, 26.14194573437305635 ) ) ;
#37561 = CARTESIAN_POINT ( 'NONE',  ( 17.62500000000000000, 6.123233995736764310E-16, -4.999999999999998224 ) ) ;
#37562 = CARTESIAN_POINT ( 'NONE',  ( 4.243569643749999898, 13.33437500061451786, -30.00000000000000000 ) ) ;
#37563 = CARTESIAN_POINT ( 'NONE',  ( 15.48750000122903359, 6.123233995736764310E-16, -4.999999999999998224 ) ) ;
#37564 = CARTESIAN_POINT ( 'NONE',  ( 9.984375000614518214, 4.541064518000418104, 2.621784821874999949 ) ) ;
#37565 = CARTESIAN_POINT ( 'NONE',  ( -4.243569643749997233, 17.14062500061451644, -27.54997392385601174 ) ) ;
#37566 = CARTESIAN_POINT ( 'NONE',  ( 17.62500000122903288, -5.773502691896255534, -1.060575238724906372E-15 ) ) ;
#37567 = CARTESIAN_POINT ( 'NONE',  ( 10.45312500061451644, 0.000000000000000000, 5.243569643749999010 ) ) ;
#37568 = ORIENTED_EDGE ( 'NONE', *, *, #48397, .F. ) ;
#37569 = CARTESIAN_POINT ( 'NONE',  ( 15.29999999999999893, -4.330127018922190985, -2.500000000000001332 ) ) ;
#37570 = CARTESIAN_POINT ( 'NONE',  ( -3.999999999999999112, 17.41250000122903430, -30.00000000000000000 ) ) ;
#37571 = CARTESIAN_POINT ( 'NONE',  ( 9.609375000614518214, 0.000000000000000000, 5.243569643749999010 ) ) ;
#37572 = CARTESIAN_POINT ( 'NONE',  ( -3.999999999999999112, 14.22500000122903430, 27.69059892324149885 ) ) ;
#37573 = CARTESIAN_POINT ( 'NONE',  ( 11.17500000122903536, 2.886751345948126879, 4.999999999999999112 ) ) ;
#37574 = CARTESIAN_POINT ( 'NONE',  ( 19.50000000122903288, -2.886751345948125991, -5.000000000000000000 ) ) ;
#37575 = CARTESIAN_POINT ( 'NONE',  ( 14.72812500061451679, 6.421520780324663323E-16, -5.243569643749999010 ) ) ;
#37576 = CARTESIAN_POINT ( 'NONE',  ( 20.46562500061451928, -6.054752690667223547, -1.112240025338166033E-15 ) ) ;
#37577 = CARTESIAN_POINT ( 'NONE',  ( 28.23750000122903359, 4.330127018922191873, 2.499999999999999556 ) ) ;
#37578 = ADVANCED_FACE ( 'NONE', ( #53867 ), #19492, .T. ) ;
#37579 = CARTESIAN_POINT ( 'NONE',  ( 29.66250000122903074, 0.000000000000000000, 4.999999999999998224 ) ) ;
#37581 = EDGE_CURVE ( 'NONE', #29982, #44755, #3258, .T. ) ;
#37580 = CARTESIAN_POINT ( 'NONE',  ( 24.22500000000000142, -4.330127018922194537, 2.499999999999995559 ) ) ;
#37582 = CARTESIAN_POINT ( 'NONE',  ( -7.967954043666661671E-16, 14.77812499938548463, 34.33755215474603517 ) ) ;
#37583 = CARTESIAN_POINT ( 'NONE',  ( 27.26249999999999929, 2.886751345948126879, 4.999999999999999112 ) ) ;
#37584 = CARTESIAN_POINT ( 'NONE',  ( 27.68437500061451573, -4.541064518000419881, 2.621784821874995952 ) ) ;
#37585 = CARTESIAN_POINT ( 'NONE',  ( 26.64375000122903003, -2.886751345948139758, -4.999999999999975131 ) ) ;
#37586 = CARTESIAN_POINT ( 'NONE',  ( 13.61250000122903359, -4.330127018922190985, -2.500000000000001332 ) ) ;
#37587 = CARTESIAN_POINT ( 'NONE',  ( 4.200000000000001954, 4.330127018922192761, -2.499999999999997780 ) ) ;
#37588 =( BOUNDED_CURVE ( )  B_SPLINE_CURVE ( 2, ( #3985, #49050, #55316, #66395, #65288, #37949, #14676, #60468, #3617 ),
 .UNSPECIFIED., .F., .F. ) 
 B_SPLINE_CURVE_WITH_KNOTS ( ( 3, 2, 2, 2, 3 ),
 ( 0.7065217391304348116, 0.7101449275362319291, 0.7173913043478260532, 0.7246376811594202882, 0.7282608695652174058 ),
 .UNSPECIFIED. ) 
 CURVE ( )  GEOMETRIC_REPRESENTATION_ITEM ( )  RATIONAL_B_SPLINE_CURVE ( ( 0.9330127018922194093, 0.9330127018922194093, 1.000000000000000000, 0.8660254037844387076, 1.000000000000000000, 0.8660254037844387076, 1.000000000000000000, 0.9330127018922194093, 0.9330127018922194093 ) ) 
 REPRESENTATION_ITEM ( '' )  );
#37589 = FACE_BOUND ( 'NONE', #14934, .T. ) ;
#37590 = CARTESIAN_POINT ( 'NONE',  ( 6.721875000614518925, 3.027376345333613106, -5.243569643749998122 ) ) ;
#37591 = CARTESIAN_POINT ( 'NONE',  ( 26.99062500061451431, 6.054752690667223547, 3.707466751127219781E-16 ) ) ;
#37592 = CARTESIAN_POINT ( 'NONE',  ( 1.878215178125000495, 13.27812499938548285, 26.74683588394047007 ) ) ;
#37593 = CARTESIAN_POINT ( 'NONE',  ( 3.999999999999999112, 10.43750000122903465, 30.00000000000000000 ) ) ;
#37594 = CARTESIAN_POINT ( 'NONE',  ( 27.43125000122903145, -4.330127018922194537, 2.499999999999995559 ) ) ;
#37595 = CARTESIAN_POINT ( 'NONE',  ( 4.884375000614518569, 6.421520780324663323E-16, -5.243569643749999010 ) ) ;
#37596 = CARTESIAN_POINT ( 'NONE',  ( 9.534375000614517148, 4.541064518000418104, 2.621784821874999949 ) ) ;
#37597 = CARTESIAN_POINT ( 'NONE',  ( 4.762499999999999289, 2.886751345948126879, 4.999999999999999112 ) ) ;
#37598 = CARTESIAN_POINT ( 'NONE',  ( 4.243569643749999898, 12.37812500061459353, 30.00000000000000000 ) ) ;
#37599 = CARTESIAN_POINT ( 'NONE',  ( 22.64999999999999858, 4.330127018922192761, -2.499999999999997780 ) ) ;
#37600 = CARTESIAN_POINT ( 'NONE',  ( 28.80000000000000071, -4.330127018922190985, -2.500000000000001332 ) ) ;
#37601 = CARTESIAN_POINT ( 'NONE',  ( 3.675000000000001155, 6.123233995736764310E-16, -4.999999999999998224 ) ) ;
#37602 = EDGE_LOOP ( 'NONE', ( #71428, #70187, #58525, #18243 ) ) ;
#37603 = CARTESIAN_POINT ( 'NONE',  ( 18.40312500061451573, 4.541064518000418104, -2.621784821874998173 ) ) ;
#37604 = CARTESIAN_POINT ( 'NONE',  ( 11.31562500061451892, 3.027376345333611329, 5.243569643749999010 ) ) ;
#37605 = CARTESIAN_POINT ( 'NONE',  ( 20.33437500061451786, -2.746126346562646425, 4.756430356249996549 ) ) ;
#37606 = CARTESIAN_POINT ( 'NONE',  ( 6.534375000614517148, -4.541064518000419881, 2.621784821874995952 ) ) ;
#37607 = CARTESIAN_POINT ( 'NONE',  ( 24.03750000000000142, 5.773502691896255534, 3.535250795749688894E-16 ) ) ;
#37608 = CARTESIAN_POINT ( 'NONE',  ( 20.21250000122903145, 0.000000000000000000, 4.999999999999998224 ) ) ;
#37609 = CARTESIAN_POINT ( 'NONE',  ( 15.56249999999999467, 2.886751345948182834, 4.999999999999902300 ) ) ;
#37610 = CARTESIAN_POINT ( 'NONE',  ( 10.28437500061451715, 6.421520780324663323E-16, -5.243569643749999010 ) ) ;
#37611 = CARTESIAN_POINT ( 'NONE',  ( 13.69687500061451679, -3.027376345333614438, 5.243569643749998122 ) ) ;
#37612 = CARTESIAN_POINT ( 'NONE',  ( 23.59687500061451715, -3.027376345333614438, 5.243569643749998122 ) ) ;
#37613 = DIRECTION ( 'NONE',  ( 0.000000000000000000, 0.000000000000000000, 1.000000000000000000 ) ) ;
#37614 = CARTESIAN_POINT ( 'NONE',  ( 13.38750000000000107, -2.886751345948129988, 4.999999999999997335 ) ) ;
#37615 = CARTESIAN_POINT ( 'NONE',  ( 17.55937500061451573, 4.541064518000418104, -2.621784821874998173 ) ) ;
#37616 = CARTESIAN_POINT ( 'NONE',  ( 8.859375000614518214, -4.541064518000417216, -2.621784821875001281 ) ) ;
#37617 = CARTESIAN_POINT ( 'NONE',  ( -0.6941602726958887581, 20.72676555956768851, 33.93677853444431491 ) ) ;
#37618 = CARTESIAN_POINT ( 'NONE',  ( 20.47500000000000142, 4.330127018922191873, 2.499999999999999556 ) ) ;
#37619 = CARTESIAN_POINT ( 'NONE',  ( -4.000000000000000888, 15.91249999999999964, 32.30940107675850470 ) ) ;
#37620 = CARTESIAN_POINT ( 'NONE',  ( 5.810221930991193690E-16, 17.11249999999999716, 26.00000000000000000 ) ) ;
#37621 = CARTESIAN_POINT ( 'NONE',  ( 24.23437500061451644, 5.824947211148865298E-16, -4.756430356249998326 ) ) ;
#37622 = CARTESIAN_POINT ( 'NONE',  ( 11.31562500061451892, 3.027376345333611329, 5.243569643749999010 ) ) ;
#37623 = CARTESIAN_POINT ( 'NONE',  ( 28.58437500061451786, -4.541064518000419881, 2.621784821874995952 ) ) ;
#37624 = LINE ( 'NONE', #60147, #55046 ) ;
#37625 = CARTESIAN_POINT ( 'NONE',  ( 12.41249999999999964, 2.886751345948126879, 4.999999999999999112 ) ) ;
#37626 = CARTESIAN_POINT ( 'NONE',  ( 1.999999999999998668, 17.71250000122903501, 26.53589838486224650 ) ) ;
#37627 = CARTESIAN_POINT ( 'NONE',  ( 12.37500000122903465, 2.886751345948129099, -4.999999999999998224 ) ) ;
#37628 = CARTESIAN_POINT ( 'NONE',  ( 21.45937500061451786, -4.541064518000417216, -2.621784821875001281 ) ) ;
#37629 = CARTESIAN_POINT ( 'NONE',  ( 17.70937500061451431, 0.000000000000000000, 5.243569643749999010 ) ) ;
#37630 = CARTESIAN_POINT ( 'NONE',  ( -2.000000000000000000, 16.32499999999999929, -33.46410161513775705 ) ) ;
#37631 = ORIENTED_EDGE ( 'NONE', *, *, #32039, .T. ) ;
#37632 = CARTESIAN_POINT ( 'NONE',  ( 16.90312500061451573, -4.541064518000417216, -2.621784821875001281 ) ) ;
#37633 = CARTESIAN_POINT ( 'NONE',  ( 29.40000000122903145, -2.886751345948125991, -5.000000000000000000 ) ) ;
#37634 = CARTESIAN_POINT ( 'NONE',  ( 17.67187500061451644, 3.027376345333611329, 5.243569643749999010 ) ) ;
#37635 = CARTESIAN_POINT ( 'NONE',  ( 3.665625000614517681, 3.027376345333611329, 5.243569643749999010 ) ) ;
#37636 = CARTESIAN_POINT ( 'NONE',  ( 18.36562500061451431, 3.027376345333613106, -5.243569643749998122 ) ) ;
#37637 = CARTESIAN_POINT ( 'NONE',  ( 30.00000000000000000, 0.000000000000000000, 4.999999999999998224 ) ) ;
#37638 = CARTESIAN_POINT ( 'NONE',  ( 27.90937500061451715, 4.541064518000418104, -2.621784821874998173 ) ) ;
#37639 = CARTESIAN_POINT ( 'NONE',  ( -4.243569643749999898, 12.15312500061451573, 30.00000000000000000 ) ) ;
#37640 = CARTESIAN_POINT ( 'NONE',  ( 16.42500000122903359, 2.886751345948129099, -4.999999999999998224 ) ) ;
#37641 = CARTESIAN_POINT ( 'NONE',  ( 10.50937500061451679, 0.000000000000000000, 4.756430356249998326 ) ) ;
#37642 = CARTESIAN_POINT ( 'NONE',  ( 27.25312500061451360, -4.541064518000417216, -2.621784821875001281 ) ) ;
#37643 = CARTESIAN_POINT ( 'NONE',  ( 0.000000000000000000, 20.00000000000000000, 30.00000000000000000 ) ) ;
#37644 = CARTESIAN_POINT ( 'NONE',  ( 19.80937500061451573, 4.541064518000418104, -2.621784821874998173 ) ) ;
#37645 = CARTESIAN_POINT ( 'NONE',  ( 22.65000000122903856, -2.886751345948125991, -5.000000000000000000 ) ) ;
#37646 =( BOUNDED_CURVE ( )  B_SPLINE_CURVE ( 2, ( #51164, #567, #45629, #40088, #62602, #11998, #65880, #58858, #48529 ),
 .UNSPECIFIED., .F., .F. ) 
 B_SPLINE_CURVE_WITH_KNOTS ( ( 3, 2, 2, 2, 3 ),
 ( 0.7500000000000000000, 0.7536231884057971175, 0.7608695652173913526, 0.7681159420289854767, 0.7717391304347825942 ),
 .UNSPECIFIED. ) 
 CURVE ( )  GEOMETRIC_REPRESENTATION_ITEM ( )  RATIONAL_B_SPLINE_CURVE ( ( 0.9330127018922194093, 0.9330127018922194093, 1.000000000000000000, 0.8660254037844387076, 1.000000000000000000, 0.8660254037844387076, 1.000000000000000000, 0.9330127018922194093, 0.9330127018922194093 ) ) 
 REPRESENTATION_ITEM ( '' )  );
#37647 = CARTESIAN_POINT ( 'NONE',  ( 22.90312500061451573, 4.541064518000418104, -2.621784821874998173 ) ) ;
#37648 = CARTESIAN_POINT ( 'NONE',  ( 17.93437500061451928, 6.421520780324663323E-16, -5.243569643749999010 ) ) ;
#37649 = CARTESIAN_POINT ( 'NONE',  ( 11.65312500061451573, 4.541064518000418104, -2.621784821874998173 ) ) ;
#37650 = CARTESIAN_POINT ( 'NONE',  ( 2.121784821874999061, 15.20937500061451786, 26.32496088578401583 ) ) ;
#37651 = CARTESIAN_POINT ( 'NONE',  ( 19.75312500061451360, 4.541064518000418104, -2.621784821874998173 ) ) ;
#37652 = CARTESIAN_POINT ( 'NONE',  ( 28.75312500061451715, 4.541064518000418104, -2.621784821874998173 ) ) ;
#37653 = ORIENTED_EDGE ( 'NONE', *, *, #32494, .F. ) ;
#37654 = ORIENTED_EDGE ( 'NONE', *, *, #63887, .T. ) ;
#37655 = CARTESIAN_POINT ( 'NONE',  ( 23.62500000000000000, 4.330127018922191873, 2.499999999999999556 ) ) ;
#37656 = CARTESIAN_POINT ( 'NONE',  ( 9.001249775931846008E-16, 19.07187500061451502, -25.09994784771203058 ) ) ;
#37657 = CARTESIAN_POINT ( 'NONE',  ( 13.20000000122903394, -2.886751345948126435, -5.000000000000000000 ) ) ;
#37658 = CARTESIAN_POINT ( 'NONE',  ( 24.06562500061451715, -6.054752690667223547, -1.112240025338166033E-15 ) ) ;
#37659 = CARTESIAN_POINT ( 'NONE',  ( 4.828125000614518214, 6.421520780324663323E-16, -5.243569643749999010 ) ) ;
#37660 = CARTESIAN_POINT ( 'NONE',  ( 16.65000000122903501, -2.886751345948129988, 4.999999999999997335 ) ) ;
#37661 = CARTESIAN_POINT ( 'NONE',  ( 23.46562500061451573, 3.027376345333611329, 5.243569643749999010 ) ) ;
#37662 = CARTESIAN_POINT ( 'NONE',  ( 21.86250000000000071, 2.886751345948126879, 4.999999999999999112 ) ) ;
#37663 = CARTESIAN_POINT ( 'NONE',  ( 27.17812500061451786, -4.541064518000419881, 2.621784821874995952 ) ) ;
#37664 = CARTESIAN_POINT ( 'NONE',  ( 8.578125000614518214, 4.541064518000418104, 2.621784821874999949 ) ) ;
#37665 = ORIENTED_EDGE ( 'NONE', *, *, #57573, .F. ) ;
#37666 = ADVANCED_FACE ( 'NONE', ( #65296 ), #57929, .F. ) ;
#37667 = CARTESIAN_POINT ( 'NONE',  ( 23.31562500061451715, 3.027376345333613106, -5.243569643749998122 ) ) ;
#37668 = CARTESIAN_POINT ( 'NONE',  ( 4.865625000614517859, 3.027376345333613106, -5.243569643749998122 ) ) ;
#37669 = CARTESIAN_POINT ( 'NONE',  ( 15.00937500061451679, 0.000000000000000000, 4.756430356249998326 ) ) ;
#37670 = CARTESIAN_POINT ( 'NONE',  ( 4.415625000614518569, 3.027376345333613106, -5.243569643749998122 ) ) ;
#37671 = CARTESIAN_POINT ( 'NONE',  ( -1.999999999999997113, 12.53750000122903430, -26.53589838486224295 ) ) ;
#37672 = CARTESIAN_POINT ( 'NONE',  ( -3.999999999999999112, 10.51250000000000107, -32.30940107675850470 ) ) ;
#37673 = CARTESIAN_POINT ( 'NONE',  ( 10.53750000000000320, 5.773502691896255534, 3.535250795749688894E-16 ) ) ;
#37674 = CARTESIAN_POINT ( 'NONE',  ( 11.29687500061451644, 6.054752690667223547, 3.707466751127219781E-16 ) ) ;
#37675 = CARTESIAN_POINT ( 'NONE',  ( 7.237500001229035362, -4.330127018922194537, 2.499999999999995559 ) ) ;
#37676 = CARTESIAN_POINT ( 'NONE',  ( 15.08437500061451786, -4.541064518000419881, 2.621784821874995952 ) ) ;
#37677 = CARTESIAN_POINT ( 'NONE',  ( 7.059375000614518392, -4.541064518000417216, -2.621784821875001281 ) ) ;
#37678 = CARTESIAN_POINT ( 'NONE',  ( 30.00000000000000000, 0.000000000000000000, 0.000000000000000000 ) ) ;
#37679 = CARTESIAN_POINT ( 'NONE',  ( 45.00000000000000000, 0.000000000000000000, 0.000000000000000000 ) ) ;
#37680 = CARTESIAN_POINT ( 'NONE',  ( 13.35937500061451821, -4.541064518000417216, -2.621784821875001281 ) ) ;
#37681 = CARTESIAN_POINT ( 'NONE',  ( 20.99062500061451431, -3.027376345333610441, -5.243569643749999898 ) ) ;
#37682 = CARTESIAN_POINT ( 'NONE',  ( 1.999999999999998668, 11.75000000000000178, 26.53589838486224650 ) ) ;
#37683 = CARTESIAN_POINT ( 'NONE',  ( 20.04375000122902861, 5.773502691896255534, 3.535250795749688401E-16 ) ) ;
#37684 = CARTESIAN_POINT ( 'NONE',  ( 23.52187500061451786, 3.027376345333611329, 5.243569643749999010 ) ) ;
#37685 = CARTESIAN_POINT ( 'NONE',  ( 7.176562500921773946, 0.000000000000000000, 4.878215178124998275 ) ) ;
#37686 = CARTESIAN_POINT ( 'NONE',  ( 4.453125000614517326, 4.541064518000418104, -2.621784821874998173 ) ) ;
#37687 = CARTESIAN_POINT ( 'NONE',  ( 21.08437500061451786, 5.492252693125287522, 3.363034840372157021E-16 ) ) ;
#37688 = CARTESIAN_POINT ( 'NONE',  ( 18.62812500061451715, -4.541064518000419881, 2.621784821874995952 ) ) ;
#37689 = CARTESIAN_POINT ( 'NONE',  ( 14.22187500061451537, -6.054752690667223547, -1.112240025338166033E-15 ) ) ;
#37690 = CARTESIAN_POINT ( 'NONE',  ( 26.06250000122903288, 0.000000000000000000, 4.999999999999998224 ) ) ;
#37691 = CARTESIAN_POINT ( 'NONE',  ( 27.67500000122903359, 2.886751345948129099, -4.999999999999998224 ) ) ;
#37692 = CARTESIAN_POINT ( 'NONE',  ( 6.009375000614519458, 0.000000000000000000, 5.243569643749999010 ) ) ;
#37693 = CARTESIAN_POINT ( 'NONE',  ( 17.25937500061451502, 0.000000000000000000, 5.243569643749999010 ) ) ;
#37694 = CARTESIAN_POINT ( 'NONE',  ( 16.10625000122903216, 0.000000000000000000, 4.999999999999998224 ) ) ;
#37695 = CARTESIAN_POINT ( 'NONE',  ( 23.36250000000000071, -5.773502691896255534, -1.060575238724906372E-15 ) ) ;
#37696 = CARTESIAN_POINT ( 'NONE',  ( 5.000000000000000888, 2.882564675336284927E-11, 5.151554443534156036 ) ) ;
#37697 = CARTESIAN_POINT ( 'NONE',  ( 24.98437500061451644, -4.541064518000419881, 2.621784821874995952 ) ) ;
#37698 = CARTESIAN_POINT ( 'NONE',  ( 17.74687500061451928, -3.027376345333614438, 5.243569643749998122 ) ) ;
#37699 = CARTESIAN_POINT ( 'NONE',  ( 3.756430356249998770, 13.61562499938548498, 32.16877607737302469 ) ) ;
#37700 = CARTESIAN_POINT ( 'NONE',  ( 5.812500001229035540, 0.000000000000000000, 4.999999999999998224 ) ) ;
#37701 = CARTESIAN_POINT ( 'NONE',  ( 9.000000000000001776, -4.330127018922190985, -2.500000000000001332 ) ) ;
#37702 = CARTESIAN_POINT ( 'NONE',  ( 9.571875000614515017, -4.119189519843968306, 2.378215178124996054 ) ) ;
#37703 = CARTESIAN_POINT ( 'NONE',  ( 18.74062500061451431, -3.027376345333610441, -5.243569643749999898 ) ) ;
#37704 = CARTESIAN_POINT ( 'NONE',  ( 8.212500000000000355, 2.886751345948129099, -4.999999999999998224 ) ) ;
#37705 = CARTESIAN_POINT ( 'NONE',  ( 4.153125000614515727, 0.000000000000000000, 5.243569643749999010 ) ) ;
#37706 = CARTESIAN_POINT ( 'NONE',  ( 20.43749999999999645, 5.773502691896255534, 3.535250795749688894E-16 ) ) ;
#37707 = EDGE_CURVE ( 'NONE', #2091, #39103, #21692, .T. ) ;
#37708 = CARTESIAN_POINT ( 'NONE',  ( 19.67812500061451786, 6.421520780324663323E-16, -5.243569643749999010 ) ) ;
#37709 = CARTESIAN_POINT ( 'NONE',  ( 15.71250000122903501, 0.000000000000000000, 4.999999999999998224 ) ) ;
#37710 = CARTESIAN_POINT ( 'NONE',  ( 22.31250000122903288, 4.330127018922192761, -2.499999999999997780 ) ) ;
#37711 = DIRECTION ( 'NONE',  ( -1.000000000000000000, 0.000000000000000000, 0.000000000000000000 ) ) ;
#37712 = CARTESIAN_POINT ( 'NONE',  ( 3.374999999999999556, 4.330127018922191873, 2.499999999999999556 ) ) ;
#37713 = EDGE_CURVE ( 'NONE', #42330, #329, #58903, .T. ) ;
#37714 = ORIENTED_EDGE ( 'NONE', *, *, #50142, .F. ) ;
#37715 = CARTESIAN_POINT ( 'NONE',  ( 18.17812500061451786, -4.541064518000419881, 2.621784821874995952 ) ) ;
#37716 = CARTESIAN_POINT ( 'NONE',  ( 25.00312500061451715, -4.541064518000417216, -2.621784821875001281 ) ) ;
#37717 = CARTESIAN_POINT ( 'NONE',  ( 25.28437500061451715, 4.541064518000418104, 2.621784821874999949 ) ) ;
#37718 = CARTESIAN_POINT ( 'NONE',  ( 8.137500000000002842, -2.886751345948125991, -5.000000000000000000 ) ) ;
#37719 = CARTESIAN_POINT ( 'NONE',  ( 11.72812500061451857, 4.541064518000418104, 2.621784821874999949 ) ) ;
#37720 = CARTESIAN_POINT ( 'NONE',  ( 26.87812500061451360, 6.421520780324663323E-16, -5.243569643749999010 ) ) ;
#37721 = CARTESIAN_POINT ( 'NONE',  ( 17.93437500061451928, 6.421520780324663323E-16, -5.243569643749999010 ) ) ;
#37722 = CARTESIAN_POINT ( 'NONE',  ( 18.04687500061451999, 6.054752690667223547, 3.707466751127219781E-16 ) ) ;
#37723 = CARTESIAN_POINT ( 'NONE',  ( 6.937500001229033764, 6.123233995736764310E-16, -4.999999999999998224 ) ) ;
#37724 = CARTESIAN_POINT ( 'NONE',  ( 4.243569643749999898, 19.12812500061451715, 30.00000000000000000 ) ) ;
#37725 = CARTESIAN_POINT ( 'NONE',  ( 23.85000000122903430, -2.886751345948129988, 4.999999999999997335 ) ) ;
#37726 = CARTESIAN_POINT ( 'NONE',  ( 15.98437500061451821, -4.119189519843968306, 2.378215178124996054 ) ) ;
#37727 = CARTESIAN_POINT ( 'NONE',  ( 14.20312500061451644, -4.541064518000417216, -2.621784821875001281 ) ) ;
#37728 = CARTESIAN_POINT ( 'NONE',  ( 7.359375000614516438, 0.000000000000000000, 5.243569643749999010 ) ) ;
#37729 = CARTESIAN_POINT ( 'NONE',  ( 7.959375000614516971, -4.541064518000417216, -2.621784821875001281 ) ) ;
#37730 = EDGE_CURVE ( 'NONE', #38159, #11468, #3993, .T. ) ;
#37731 = ORIENTED_EDGE ( 'NONE', *, *, #41428, .T. ) ;
#37732 = CARTESIAN_POINT ( 'NONE',  ( -5.810221930991193690E-16, 13.58750000000000036, 26.00000000000000355 ) ) ;
#37733 = CARTESIAN_POINT ( 'NONE',  ( 18.81562500061452070, 3.027376345333613106, -5.243569643749998122 ) ) ;
#37734 = CARTESIAN_POINT ( 'NONE',  ( 23.52187500061451786, 3.027376345333611329, 5.243569643749999010 ) ) ;
#37735 = CARTESIAN_POINT ( 'NONE',  ( 20.20312500061451644, 4.541064518000418104, -2.621784821874998173 ) ) ;
#37736 = CARTESIAN_POINT ( 'NONE',  ( -3.999999999999997335, 11.93750000000000355, 32.30940107675850470 ) ) ;
#37737 = CARTESIAN_POINT ( 'NONE',  ( 26.09062500061451573, 6.054752690667223547, 3.707466751127219781E-16 ) ) ;
#37738 = CARTESIAN_POINT ( 'NONE',  ( 7.575000001229033053, 2.886751345948126879, 4.999999999999999112 ) ) ;
#37739 = ORIENTED_EDGE ( 'NONE', *, *, #67048, .F. ) ;
#37740 = CARTESIAN_POINT ( 'NONE',  ( 3.225000001229033408, -5.773502691896255534, -1.060575238724906372E-15 ) ) ;
#37741 = CARTESIAN_POINT ( 'NONE',  ( 1.999999999999998668, 14.90000000000000036, -33.46410161513775705 ) ) ;
#37742 = CARTESIAN_POINT ( 'NONE',  ( 23.02500000122903145, -5.773502691896255534, -1.060575238724906372E-15 ) ) ;
#37743 = CARTESIAN_POINT ( 'NONE',  ( -1.878215178124999163, 14.25312499938548250, 26.74683588394047007 ) ) ;
#37744 = VECTOR ( 'NONE', #35587, 1000.000000000000000 ) ;
#37745 = EDGE_CURVE ( 'NONE', #68118, #29564, #67429, .T. ) ;
#37746 = CARTESIAN_POINT ( 'NONE',  ( 7.734375000614517326, 4.541064518000418104, 2.621784821874999949 ) ) ;
#37747 = CARTESIAN_POINT ( 'NONE',  ( 20.56875000122903785, 2.886751345948154857, 4.999999999999951150 ) ) ;
#37748 = CARTESIAN_POINT ( 'NONE',  ( 11.57812500061451644, 6.421520780324663323E-16, -5.243569643749999010 ) ) ;
#37749 = CARTESIAN_POINT ( 'NONE',  ( 7.434375000614519280, -4.541064518000419881, 2.621784821874995952 ) ) ;
#37750 = CARTESIAN_POINT ( 'NONE',  ( 25.87500000122903288, 2.886751345948129099, -4.999999999999998224 ) ) ;
#37751 = CARTESIAN_POINT ( 'NONE',  ( 14.67187500061451821, -6.054752690667223547, -1.112240025338166033E-15 ) ) ;
#37752 = CARTESIAN_POINT ( 'NONE',  ( 3.909375000614518481, -4.541064518000417216, -2.621784821875001281 ) ) ;
#37753 = CARTESIAN_POINT ( 'NONE',  ( 23.92499999999999716, 6.123233995736764310E-16, -4.999999999999998224 ) ) ;
#37754 = CARTESIAN_POINT ( 'NONE',  ( 5.428125000614517859, 4.541064518000418104, 2.621784821874999949 ) ) ;
#37755 = CARTESIAN_POINT ( 'NONE',  ( 14.42812500061451786, 4.541064518000418104, 2.621784821874999949 ) ) ;
#37756 = ORIENTED_EDGE ( 'NONE', *, *, #3316, .T. ) ;
#37757 = CARTESIAN_POINT ( 'NONE',  ( 13.45312500061451466, 4.541064518000418104, -2.621784821874998173 ) ) ;
#37758 = CARTESIAN_POINT ( 'NONE',  ( 6.112500001229034474, 4.330127018922192761, -2.499999999999997780 ) ) ;
#37759 = CARTESIAN_POINT ( 'NONE',  ( 7.603125000614517681, 4.541064518000418104, -2.621784821874998173 ) ) ;
#37760 = CARTESIAN_POINT ( 'NONE',  ( 22.13437500061451502, 4.119189519843966529, 2.378215178124999607 ) ) ;
#37761 = CARTESIAN_POINT ( 'NONE',  ( 8.849999999999999645, 0.000000000000000000, 4.999999999999998224 ) ) ;
#37762 = CARTESIAN_POINT ( 'NONE',  ( 3.112500001229034918, 0.000000000000000000, 4.999999999999998224 ) ) ;
#37763 = CARTESIAN_POINT ( 'NONE',  ( 18.33749999999999858, -2.886751345948129988, 4.999999999999997335 ) ) ;
#37764 = CARTESIAN_POINT ( 'NONE',  ( 18.12187500061451573, 3.027376345333611329, 5.243569643749999010 ) ) ;
#37765 = CARTESIAN_POINT ( 'NONE',  ( 14.66250000122903252, 4.330127018922192761, -2.499999999999997780 ) ) ;
#37766 = CARTESIAN_POINT ( 'NONE',  ( 22.05000000000000071, -4.330127018922190985, -2.500000000000001332 ) ) ;
#37767 = CARTESIAN_POINT ( 'NONE',  ( -3.000416591977282496E-16, 16.54062500061451857, -34.90005215228797653 ) ) ;
#37768 = CARTESIAN_POINT ( 'NONE',  ( -2.000000000000000000, 15.98750000122903181, 26.53589838486224650 ) ) ;
#37769 = CARTESIAN_POINT ( 'NONE',  ( 4.898587196589411843E-16, 20.00000000000000000, 33.99999999999999289 ) ) ;
#37770 = CARTESIAN_POINT ( 'NONE',  ( 18.46875000122902932, -5.773502691896255534, -1.060575238724906372E-15 ) ) ;
#37771 = CARTESIAN_POINT ( 'NONE',  ( 29.57812500061451644, 6.421520780324663323E-16, -5.243569643749999010 ) ) ;
#37772 = DIRECTION ( 'NONE',  ( 0.000000000000000000, 0.000000000000000000, 1.000000000000000000 ) ) ;
#37773 = CARTESIAN_POINT ( 'NONE',  ( 16.02187500061451786, -6.054752690667223547, -1.112240025338166033E-15 ) ) ;
#37774 = CARTESIAN_POINT ( 'NONE',  ( 27.71250000000000568, 2.886751345948126879, 4.999999999999999112 ) ) ;
#37775 = CARTESIAN_POINT ( 'NONE',  ( 12.10312500061451857, 4.541064518000418104, -2.621784821874998173 ) ) ;
#37776 = CARTESIAN_POINT ( 'NONE',  ( 28.95937500061451075, -5.492252693125287522, -1.008910452111647106E-15 ) ) ;
#37777 = CARTESIAN_POINT ( 'NONE',  ( 20.33437500061451786, 4.541064518000418104, 2.621784821874999949 ) ) ;
#37778 = CARTESIAN_POINT ( 'NONE',  ( 13.65937500061451537, -5.492252693125287522, -1.008910452111647106E-15 ) ) ;
#37779 = CARTESIAN_POINT ( 'NONE',  ( 8.015625000614518214, 3.027376345333613106, -5.243569643749998122 ) ) ;
#37780 = CARTESIAN_POINT ( 'NONE',  ( 12.68437500061451573, 4.541064518000418104, 2.621784821874999949 ) ) ;
#37781 = EDGE_LOOP ( 'NONE', ( #49342, #13419, #72321, #23749 ) ) ;
#37782 = CARTESIAN_POINT ( 'NONE',  ( 23.18437500061451573, -4.541064518000419881, 2.621784821874995952 ) ) ;
#37783 = CARTESIAN_POINT ( 'NONE',  ( 2.483674929639045459, 4.345807424128182994, -33.14570507670406130 ) ) ;
#37784 = CARTESIAN_POINT ( 'NONE',  ( 26.91562500061451146, 3.027376345333613106, -5.243569643749998122 ) ) ;
#37785 = CARTESIAN_POINT ( 'NONE',  ( 26.06250000000000000, -5.773502691896255534, -1.060575238724906372E-15 ) ) ;
#37786 = CARTESIAN_POINT ( 'NONE',  ( 7.425000000000000711, 4.330127018922191873, 2.499999999999999556 ) ) ;
#37787 = CARTESIAN_POINT ( 'NONE',  ( 16.83750000122903145, 6.123233995736764310E-16, -4.999999999999998224 ) ) ;
#37788 = LINE ( 'NONE', #60308, #41940 ) ;
#37789 = CARTESIAN_POINT ( 'NONE',  ( 8.634375000614515017, -2.746126346562646425, 4.756430356249996549 ) ) ;
#37790 = VERTEX_POINT ( 'NONE', #15056 ) ;
#37791 = CARTESIAN_POINT ( 'NONE',  ( 15.18750000000000000, -2.886751345948129988, 4.999999999999997335 ) ) ;
#37792 = CARTESIAN_POINT ( 'NONE',  ( 17.84999999999999787, 0.000000000000000000, 4.999999999999998224 ) ) ;
#37793 = CARTESIAN_POINT ( 'NONE',  ( 11.20312500061451644, 4.541064518000418104, -2.621784821874998173 ) ) ;
#37794 = EDGE_CURVE ( 'NONE', #32613, #26559, #72166, .T. ) ;
#37795 = EDGE_LOOP ( 'NONE', ( #67986, #50223, #10482, #25626 ) ) ;
#37796 = CARTESIAN_POINT ( 'NONE',  ( 26.21250000000000213, 2.886751345948146419, -4.999999999999968914 ) ) ;
#37797 = CARTESIAN_POINT ( 'NONE',  ( -2.121784821874996840, 17.23437500061451999, -26.32496088578401583 ) ) ;
#37798 = CARTESIAN_POINT ( 'NONE',  ( 3.103125000614517237, 4.541064518000418104, -2.621784821874998173 ) ) ;
#37799 = CARTESIAN_POINT ( 'NONE',  ( -1.071796769724489229, 14.16740381056766473, 34.00000000000000000 ) ) ;
#37800 = CARTESIAN_POINT ( 'NONE',  ( 9.562500000000001776, 2.886751345948129099, -4.999999999999998224 ) ) ;
#37801 = CARTESIAN_POINT ( 'NONE',  ( 3.150046044403394419, 3.883032850835071770, 3.416330326112916982 ) ) ;
#37802 = ORIENTED_EDGE ( 'NONE', *, *, #8067, .T. ) ;
#37803 = CARTESIAN_POINT ( 'NONE',  ( 9.001249775931846008E-16, 13.61562500061451786, 34.90005215228797653 ) ) ;
#37804 = CARTESIAN_POINT ( 'NONE',  ( 25.67812500061451431, 4.541064518000418104, 2.621784821874999949 ) ) ;
#37805 = CARTESIAN_POINT ( 'NONE',  ( 65.00000000000000000, 9.426999614876460059E-14, 9.000000000000000000 ) ) ;
#37806 = CARTESIAN_POINT ( 'NONE',  ( 3.756430356250000546, 19.87812499938548427, 27.83122392262697886 ) ) ;
#37807 = CARTESIAN_POINT ( 'NONE',  ( 21.53437500061451715, 6.421520780324663323E-16, -5.243569643749999010 ) ) ;
#37808 = EDGE_CURVE ( 'NONE', #55534, #15843, #55400, .T. ) ;
#37809 = CARTESIAN_POINT ( 'NONE',  ( 19.30312500061451786, 4.541064518000418104, -2.621784821874998173 ) ) ;
#37810 = CARTESIAN_POINT ( 'NONE',  ( 4.243569643749999898, 14.14062500061459460, -27.54997392385601529 ) ) ;
#37811 = CARTESIAN_POINT ( 'NONE',  ( 23.92500000122903359, -5.773502691896255534, -1.060575238724906372E-15 ) ) ;
#37812 = CARTESIAN_POINT ( 'NONE',  ( 4.903125000614516615, 4.541064518000418104, -2.621784821874998173 ) ) ;
#37813 = CARTESIAN_POINT ( 'NONE',  ( 24.49687500061451573, -2.746126346562646425, 4.756430356249996549 ) ) ;
#37814 = CARTESIAN_POINT ( 'NONE',  ( 22.19062500061451004, -3.027376345333614438, 5.243569643749998122 ) ) ;
#37815 = LINE ( 'NONE', #45910, #56317 ) ;
#37816 = CARTESIAN_POINT ( 'NONE',  ( 1.878215178124997609, 15.26562499938548179, 33.25316411605952993 ) ) ;
#37818 = EDGE_CURVE ( 'NONE', #30507, #14890, #39152, .T. ) ;
#37817 = CARTESIAN_POINT ( 'NONE',  ( 15.64687500061451608, -3.027376345333610441, -5.243569643749999898 ) ) ;
#37819 = CARTESIAN_POINT ( 'NONE',  ( 15.30937500061451750, 4.541064518000418104, -2.621784821874998173 ) ) ;
#37820 = CARTESIAN_POINT ( 'NONE',  ( 21.53437500061451715, 6.421520780324663323E-16, -5.243569643749999010 ) ) ;
#37821 = CARTESIAN_POINT ( 'NONE',  ( -4.243569643749999898, 12.17187500061451999, 27.54997392385601529 ) ) ;
#37822 = CARTESIAN_POINT ( 'NONE',  ( 4.040625000614517681, 6.054752690667223547, 3.707466751127219781E-16 ) ) ;
#37823 = CARTESIAN_POINT ( 'NONE',  ( 28.19062500061451715, -3.027376345333610441, -5.243569643749999898 ) ) ;
#37824 = CARTESIAN_POINT ( 'NONE',  ( 26.57812500061451644, 4.541064518000418104, 2.621784821874999949 ) ) ;
#37825 = CARTESIAN_POINT ( 'NONE',  ( 1.626862140677534273E-15, 14.26250000000000107, 34.00000000000000000 ) ) ;
#37826 = CARTESIAN_POINT ( 'NONE',  ( -3.999999999999999556, 18.16250000000000497, 27.69059892324149530 ) ) ;
#37827 = CARTESIAN_POINT ( 'NONE',  ( 6.196875000614515905, -3.027376345333610441, -5.243569643749999898 ) ) ;
#37828 = CARTESIAN_POINT ( 'NONE',  ( 15.41250000122903252, -4.330127018922190985, -2.500000000000001332 ) ) ;
#37829 = CARTESIAN_POINT ( 'NONE',  ( 8.437500001229034652, 4.330127018922191873, 2.499999999999999556 ) ) ;
#37830 = CARTESIAN_POINT ( 'NONE',  ( 4.265625000614517326, -6.054752690667223547, -1.112240025338166033E-15 ) ) ;
#37831 = CARTESIAN_POINT ( 'NONE',  ( 3.999999999999998668, 15.55624999877096748, 32.30940107675850470 ) ) ;
#37832 = CARTESIAN_POINT ( 'NONE',  ( 17.53125000122903288, -4.330127018922194537, 2.499999999999995559 ) ) ;
#37833 = CARTESIAN_POINT ( 'NONE',  ( 15.23437500061451644, 6.421520780324663323E-16, -5.243569643749999010 ) ) ;
#37834 = CARTESIAN_POINT ( 'NONE',  ( 11.77500000000000036, 6.123233995736764310E-16, -4.999999999999998224 ) ) ;
#37835 = EDGE_LOOP ( 'NONE', ( #28178, #36208, #62993, #34504 ) ) ;
#37836 = CARTESIAN_POINT ( 'NONE',  ( 19.07812500061451644, -4.541064518000419881, 2.621784821874995952 ) ) ;
#37837 = CARTESIAN_POINT ( 'NONE',  ( 6.253125000614517148, 4.541064518000418104, -2.621784821874998173 ) ) ;
#37838 = CARTESIAN_POINT ( 'NONE',  ( 24.27187500061451786, 3.027376345333612662, -5.243569643749998122 ) ) ;
#37839 = CARTESIAN_POINT ( 'NONE',  ( 8.728125000614518569, -4.541064518000419881, 2.621784821874995952 ) ) ;
#37840 = CARTESIAN_POINT ( 'NONE',  ( 20.77500000000000213, 6.123233995736764310E-16, -4.999999999999998224 ) ) ;
#37841 = CARTESIAN_POINT ( 'NONE',  ( 7.987500001229032698, 4.330127018922191873, 2.499999999999999556 ) ) ;
#37842 = CARTESIAN_POINT ( 'NONE',  ( 22.41562500061451502, 3.027376345333613106, -5.243569643749998122 ) ) ;
#37843 = CARTESIAN_POINT ( 'NONE',  ( 4.000000000000000000, 18.95000000122903216, -27.69059892324149530 ) ) ;
#37844 = CARTESIAN_POINT ( 'NONE',  ( 10.87500000122903288, -5.773502691896255534, -1.060575238724906372E-15 ) ) ;
#37845 = CARTESIAN_POINT ( 'NONE',  ( 20.80312500061451431, 0.000000000000000000, 5.243569643749999010 ) ) ;
#37846 = CARTESIAN_POINT ( 'NONE',  ( 15.85312500061451857, 0.000000000000000000, 5.243569643749999010 ) ) ;
#37847 = CARTESIAN_POINT ( 'NONE',  ( 28.20937500061451786, -4.119189519843965641, -2.378215178125001383 ) ) ;
#37848 = CARTESIAN_POINT ( 'NONE',  ( 16.38749999999999929, 5.773502691896255534, 3.535250795749688894E-16 ) ) ;
#37849 = CARTESIAN_POINT ( 'NONE',  ( 11.43750000122903465, 6.123233995736764310E-16, -4.999999999999998224 ) ) ;
#37850 =( BOUNDED_CURVE ( )  B_SPLINE_CURVE ( 2, ( #11380, #21723, #61978, #34257, #56790, #33535, #44652 ),
 .UNSPECIFIED., .F., .F. ) 
 B_SPLINE_CURVE_WITH_KNOTS ( ( 3, 2, 2, 3 ),
 ( 0.4300000000000001044, 0.4333333333333334036, 0.4366666666666667029, 0.4400000000000000022 ),
 .UNSPECIFIED. ) 
 CURVE ( )  GEOMETRIC_REPRESENTATION_ITEM ( )  RATIONAL_B_SPLINE_CURVE ( ( 0.9999999999999955591, 0.8660254037844431485, 1.000000000000000000, 0.8660254037844387076, 1.000000000000000000, 0.8660254037844387076, 1.000000000000000000 ) ) 
 REPRESENTATION_ITEM ( '' )  );
#37851 = EDGE_CURVE ( 'NONE', #52599, #67375, #38704, .T. ) ;
#37852 = CARTESIAN_POINT ( 'NONE',  ( 8.840625000614515727, -3.027376345333610441, -5.243569643749999898 ) ) ;
#37853 = CARTESIAN_POINT ( 'NONE',  ( 10.86562500061451431, 3.027376345333611329, 5.243569643749999010 ) ) ;
#37854 = CARTESIAN_POINT ( 'NONE',  ( 20.51250000122903216, 4.330127018922192761, -2.499999999999997780 ) ) ;
#37855 = CARTESIAN_POINT ( 'NONE',  ( 19.92187500061451644, 3.027376345333611329, 5.243569643749999010 ) ) ;
#37856 = CARTESIAN_POINT ( 'NONE',  ( 22.03125000122903288, -4.330127018922194537, 2.499999999999995559 ) ) ;
#37857 = CARTESIAN_POINT ( 'NONE',  ( 6.112500001229034474, 4.330127018922192761, -2.499999999999997780 ) ) ;
#37858 = CARTESIAN_POINT ( 'NONE',  ( 4.059375000614519280, 4.541064518000418104, -2.621784821874998173 ) ) ;
#37859 = CARTESIAN_POINT ( 'NONE',  ( 23.07187500061451857, 3.027376345333611329, 5.243569643749999010 ) ) ;
#37860 = VECTOR ( 'NONE', #71968, 1000.000000000000000 ) ;
#37861 =( BOUNDED_CURVE ( )  B_SPLINE_CURVE ( 2, ( #13206, #40575, #69018, #47203, #6954, #63463, #41304, #46118, #58266 ),
 .UNSPECIFIED., .F., .F. ) 
 B_SPLINE_CURVE_WITH_KNOTS ( ( 3, 2, 2, 2, 3 ),
 ( 0.3194444444444444753, 0.3240740740740740700, 0.3333333333333333148, 0.3425925925925926152, 0.3472222222222222654 ),
 .UNSPECIFIED. ) 
 CURVE ( )  GEOMETRIC_REPRESENTATION_ITEM ( )  RATIONAL_B_SPLINE_CURVE ( ( 0.9330127018922194093, 0.9330127018922197424, 1.000000000000000000, 0.8660254037844387076, 1.000000000000000000, 0.8660254037844387076, 1.000000000000000000, 0.9330127018922189652, 0.9330127018922194093 ) ) 
 REPRESENTATION_ITEM ( '' )  );
#37862 = CARTESIAN_POINT ( 'NONE',  ( 26.51250000122903216, 0.000000000000000000, 4.999999999999998224 ) ) ;
#37863 = CARTESIAN_POINT ( 'NONE',  ( 18.77812500061451573, 6.421520780324663323E-16, -5.243569643749999010 ) ) ;
#37864 = CARTESIAN_POINT ( 'NONE',  ( 23.29687500061451644, -3.027376345333610441, -5.243569643749999898 ) ) ;
#37865 = CARTESIAN_POINT ( 'NONE',  ( -7.967954043666661671E-16, 18.49062499938548143, 34.33755215474603517 ) ) ;
#37866 = CARTESIAN_POINT ( 'NONE',  ( 4.603329117574985752, 1.951758446961684434, -4.603329117574985752 ) ) ;
#37867 = CARTESIAN_POINT ( 'NONE',  ( 28.17187500061451644, -6.054752690667223547, -1.112240025338166033E-15 ) ) ;
#37868 = CARTESIAN_POINT ( 'NONE',  ( 20.22187500061451715, 4.119189519843966529, 2.378215178124999607 ) ) ;
#37869 = CARTESIAN_POINT ( 'NONE',  ( 16.00312500061451715, -4.541064518000417216, -2.621784821875001281 ) ) ;
#37870 = CARTESIAN_POINT ( 'NONE',  ( 13.24687500061451750, -3.027376345333614438, 5.243569643749998122 ) ) ;
#37871 = ORIENTED_EDGE ( 'NONE', *, *, #27156, .T. ) ;
#37872 = CARTESIAN_POINT ( 'NONE',  ( 9.150000000000002132, 4.330127018922192761, -2.499999999999997780 ) ) ;
#37873 = CARTESIAN_POINT ( 'NONE',  ( 21.81562500061451004, -6.054752690667223547, -1.112240025338166033E-15 ) ) ;
#37874 = CARTESIAN_POINT ( 'NONE',  ( 2.000000000000001332, 12.95000000000000107, -26.53589838486224650 ) ) ;
#37875 = CARTESIAN_POINT ( 'NONE',  ( 14.43750000000000000, -2.886751345948125991, -5.000000000000000000 ) ) ;
#37876 = CARTESIAN_POINT ( 'NONE',  ( 24.90000000122903145, -2.886751345948125991, -5.000000000000000000 ) ) ;
#37877 = CARTESIAN_POINT ( 'NONE',  ( 18.62812500061451715, -4.541064518000419881, 2.621784821874995952 ) ) ;
#37878 = ORIENTED_EDGE ( 'NONE', *, *, #50272, .T. ) ;
#37879 = CARTESIAN_POINT ( 'NONE',  ( 21.78750000000000142, 5.773502691896255534, 3.535250795749688894E-16 ) ) ;
#37880 = CARTESIAN_POINT ( 'NONE',  ( 23.59687500061451715, -3.027376345333614438, 5.243569643749998122 ) ) ;
#37881 = VERTEX_POINT ( 'NONE', #33148 ) ;
#37882 = CARTESIAN_POINT ( 'NONE',  ( 21.22500000000000142, 6.123233995736764310E-16, -4.999999999999998224 ) ) ;
#37883 = CARTESIAN_POINT ( 'NONE',  ( 10.22812500061451679, 6.421520780324663323E-16, -5.243569643749999010 ) ) ;
#37884 = CARTESIAN_POINT ( 'NONE',  ( 3.065625000614517592, 3.027376345333613106, -5.243569643749998122 ) ) ;
#37885 = CARTESIAN_POINT ( 'NONE',  ( 14.97187500061451537, -4.119189519843968306, 2.378215178124996054 ) ) ;
#37886 = CARTESIAN_POINT ( 'NONE',  ( 27.14062500061451644, -3.027376345333614438, 5.243569643749998122 ) ) ;
#37887 =( BOUNDED_CURVE ( )  B_SPLINE_CURVE ( 2, ( #51305, #35034, #18030, #1435, #40586, #63106, #52032, #58277, #69397 ),
 .UNSPECIFIED., .F., .F. ) 
 B_SPLINE_CURVE_WITH_KNOTS ( ( 3, 2, 2, 2, 3 ),
 ( 0.6527777777777777901, 0.6574074074074074403, 0.6666666666666666297, 0.6759259259259259300, 0.6805555555555555802 ),
 .UNSPECIFIED. ) 
 CURVE ( )  GEOMETRIC_REPRESENTATION_ITEM ( )  RATIONAL_B_SPLINE_CURVE ( ( 0.9330127018922194093, 0.9330127018922194093, 1.000000000000000000, 0.8660254037844387076, 1.000000000000000000, 0.8660254037844387076, 1.000000000000000000, 0.9330127018922194093, 0.9330127018922194093 ) ) 
 REPRESENTATION_ITEM ( '' )  );
#37888 = CARTESIAN_POINT ( 'NONE',  ( 17.92500000000000071, -4.330127018922194537, 2.499999999999995559 ) ) ;
#37889 = CARTESIAN_POINT ( 'NONE',  ( 24.37500000000000000, 6.123233995736764310E-16, -4.999999999999998224 ) ) ;
#37890 = CARTESIAN_POINT ( 'NONE',  ( 4.243569643749999010, 19.16562500061451857, 27.54997392385601174 ) ) ;
#37891 = CARTESIAN_POINT ( 'NONE',  ( 6.009375000614519458, 0.000000000000000000, 5.243569643749999010 ) ) ;
#37892 = CARTESIAN_POINT ( 'NONE',  ( 17.52187500061451431, 3.027376345333613106, -5.243569643749998122 ) ) ;
#37893 = CARTESIAN_POINT ( 'NONE',  ( 29.22187500061451715, 3.027376345333613106, -5.243569643749998122 ) ) ;
#37894 = ORIENTED_EDGE ( 'NONE', *, *, #40409, .T. ) ;
#37895=STYLED_ITEM('',(#73144),#20659);
#37896 = CARTESIAN_POINT ( 'NONE',  ( 25.79062500061451502, -3.027376345333614438, 5.243569643749998122 ) ) ;
#37897 = CARTESIAN_POINT ( 'NONE',  ( 28.32187500061451502, 3.027376345333613106, -5.243569643749998122 ) ) ;
#37898 = DIRECTION ( 'NONE',  ( -0.000000000000000000, -1.000000000000000000, -0.000000000000000000 ) ) ;
#37899 = CARTESIAN_POINT ( 'NONE',  ( 13.23750000000000071, 5.773502691896255534, 3.535250795749688894E-16 ) ) ;
#37900 = CARTESIAN_POINT ( 'NONE',  ( 10.15312500061451750, -4.541064518000417216, -2.621784821875001281 ) ) ;
#37901 = CARTESIAN_POINT ( 'NONE',  ( 15.39375000122903359, -2.886751345948126435, -5.000000000000000000 ) ) ;
#37902 = CARTESIAN_POINT ( 'NONE',  ( 24.37500000000000000, 6.123233995736764310E-16, -4.999999999999998224 ) ) ;
#37903 = CARTESIAN_POINT ( 'NONE',  ( 29.61562500061451431, 3.027376345333612662, -5.243569643749998122 ) ) ;
#37904 = CARTESIAN_POINT ( 'NONE',  ( 15.45000000122903216, -2.886751345948125991, -5.000000000000000000 ) ) ;
#37905 = CARTESIAN_POINT ( 'NONE',  ( 3.103072119908869997, -3.920863138419562244, 3.103072119908869997 ) ) ;
#37906 = CARTESIAN_POINT ( 'NONE',  ( 14.18437500061451750, -4.119189519843968306, 2.378215178124996054 ) ) ;
#37907 = CARTESIAN_POINT ( 'NONE',  ( 6.328125000614515550, 4.541064518000418104, 2.621784821874999949 ) ) ;
#37908 = CARTESIAN_POINT ( 'NONE',  ( 21.64687500061451786, 6.054752690667223547, 3.707466751127219781E-16 ) ) ;
#37909 = CARTESIAN_POINT ( 'NONE',  ( -4.243569643749999898, 16.22187500061452070, 27.54997392385601529 ) ) ;
#37910 = EDGE_CURVE ( 'NONE', #12976, #32725, #55685, .T. ) ;
#37911 = CARTESIAN_POINT ( 'NONE',  ( 22.24687500061451217, -3.027376345333614438, 5.243569643749998122 ) ) ;
#37912 = CARTESIAN_POINT ( 'NONE',  ( 5.175000000000002487, 4.330127018922191873, 2.499999999999999556 ) ) ;
#37913 = CARTESIAN_POINT ( 'NONE',  ( -3.999999999999997335, 11.60000000122903430, 32.30940107675850470 ) ) ;
#37914 = CARTESIAN_POINT ( 'NONE',  ( 11.84062500061451750, -3.027376345333614438, 5.243569643749998122 ) ) ;
#37915 = CARTESIAN_POINT ( 'NONE',  ( 4.687500001229034652, 6.123233995736764310E-16, -4.999999999999998224 ) ) ;
#37916 = CARTESIAN_POINT ( 'NONE',  ( 8.671875000614518214, 3.027376345333611329, 5.243569643749999010 ) ) ;
#37917 = CARTESIAN_POINT ( 'NONE',  ( 0.000000000000000000, 20.00000000000000000, -30.00000000000000000 ) ) ;
#37918 = CARTESIAN_POINT ( 'NONE',  ( 9.965625000614517504, 3.027376345333611329, 5.243569643749999010 ) ) ;
#37919 = CARTESIAN_POINT ( 'NONE',  ( 15.12187500061451750, -6.054752690667223547, -1.112240025338166033E-15 ) ) ;
#37920 = DIRECTION ( 'NONE',  ( 0.000000000000000000, 0.000000000000000000, 1.000000000000000000 ) ) ;
#37921 = CARTESIAN_POINT ( 'NONE',  ( 20.51250000122903216, 4.330127018922192761, -2.499999999999997780 ) ) ;
#37922 = CARTESIAN_POINT ( 'NONE',  ( 8.409375000614518925, -4.541064518000417216, -2.621784821875001281 ) ) ;
#37923 = CARTESIAN_POINT ( 'NONE',  ( 11.24062500061451608, 6.054752690667223547, 3.707466751127219781E-16 ) ) ;
#37924 = CARTESIAN_POINT ( 'NONE',  ( 25.29375000122902861, -2.886751345948125991, -5.000000000000000000 ) ) ;
#37925 = CARTESIAN_POINT ( 'NONE',  ( 22.28437500061451715, -4.541064518000419881, 2.621784821874995952 ) ) ;
#37926 = CARTESIAN_POINT ( 'NONE',  ( 25.57500000122903572, 2.886751345948093572, 5.000000000000056843 ) ) ;
#37927 = CARTESIAN_POINT ( 'NONE',  ( -3.779748323423379297, 3.276532024208883342, 31.33396265876518783 ) ) ;
#37928 = DIRECTION ( 'NONE',  ( 0.000000000000000000, 0.000000000000000000, -1.000000000000000000 ) ) ;
#37929 = CARTESIAN_POINT ( 'NONE',  ( 4.243569643749999898, 12.39687500061451786, -27.54997392385601529 ) ) ;
#37930 = CARTESIAN_POINT ( 'NONE',  ( 14.92500000122903181, -5.773502691896255534, -1.060575238724906372E-15 ) ) ;
#37931 = CARTESIAN_POINT ( 'NONE',  ( 2.121784821875001281, 18.15312500061451928, -26.32496088578401938 ) ) ;
#37932 = CARTESIAN_POINT ( 'NONE',  ( 18.45000000122903216, -2.886751345948129988, 4.999999999999997335 ) ) ;
#37933 = CARTESIAN_POINT ( 'NONE',  ( 10.52812500061451750, -4.541064518000419881, 2.621784821874995952 ) ) ;
#37934 = ORIENTED_EDGE ( 'NONE', *, *, #32753, .F. ) ;
#37935 = CARTESIAN_POINT ( 'NONE',  ( 16.38749999999999929, 5.773502691896255534, 3.535250795749688894E-16 ) ) ;
#37936 = CARTESIAN_POINT ( 'NONE',  ( 29.13749999999999574, -2.886751345948092240, 5.000000000000060396 ) ) ;
#37937 = CARTESIAN_POINT ( 'NONE',  ( 23.31562500061451715, 3.027376345333613106, -5.243569643749998122 ) ) ;
#37938 = CARTESIAN_POINT ( 'NONE',  ( 11.33437500061451608, 4.541064518000418104, 2.621784821874999949 ) ) ;
#37939 = CARTESIAN_POINT ( 'NONE',  ( 4.379101211152973683, -2.413214113851987364, -4.655270838772533004 ) ) ;
#37940 = CARTESIAN_POINT ( 'NONE',  ( 10.38750000122903572, -4.330127018922194537, 2.499999999999995559 ) ) ;
#37941 = CARTESIAN_POINT ( 'NONE',  ( 19.46250000122903145, -4.330127018922190985, -2.500000000000001332 ) ) ;
#37942 = CARTESIAN_POINT ( 'NONE',  ( 16.00312500061451715, -4.541064518000417216, -2.621784821875001281 ) ) ;
#37943 = CARTESIAN_POINT ( 'NONE',  ( 17.84062500061451573, -3.027376345333610441, -5.243569643749999898 ) ) ;
#37944 = CARTESIAN_POINT ( 'NONE',  ( 25.83750000122903501, 6.123233995736764310E-16, -4.999999999999998224 ) ) ;
#37945 = CARTESIAN_POINT ( 'NONE',  ( 29.40000000122903145, -2.886751345948125991, -5.000000000000000000 ) ) ;
#37946 = CARTESIAN_POINT ( 'NONE',  ( 23.96249999999999858, 2.886751345948129099, -4.999999999999998224 ) ) ;
#37947 = CARTESIAN_POINT ( 'NONE',  ( 3.756430356250000102, 13.09062499938548463, 30.00000000000000000 ) ) ;
#37948 = CARTESIAN_POINT ( 'NONE',  ( 26.22187500061451715, 3.027376345333611329, 5.243569643749999010 ) ) ;
#37949 = CARTESIAN_POINT ( 'NONE',  ( 4.000000000000000000, 12.53749999999999964, -27.69059892324149885 ) ) ;
#37950 = EDGE_CURVE ( 'NONE', #33507, #54392, #50150, .T. ) ;
#37951 = CARTESIAN_POINT ( 'NONE',  ( 13.27500000122903323, 2.886751345948129099, -4.999999999999998224 ) ) ;
#37952 = CARTESIAN_POINT ( 'NONE',  ( 3.037500000000002309, -2.886751345948129988, 4.999999999999997335 ) ) ;
#37953 = CARTESIAN_POINT ( 'NONE',  ( 0.000000000000000000, 27.50000000000000000, 26.00000000000000000 ) ) ;
#37954 = CARTESIAN_POINT ( 'NONE',  ( 6.796875000614516438, 6.054752690667223547, 3.707466751127219781E-16 ) ) ;
#37955 = CARTESIAN_POINT ( 'NONE',  ( 26.84062500061451573, -3.027376345333610441, -5.243569643749999898 ) ) ;
#37956 = CARTESIAN_POINT ( 'NONE',  ( 1.071796769724500997, 16.90759618943233633, 33.99999999999999289 ) ) ;
#37957 = CARTESIAN_POINT ( 'NONE',  ( -1.071796769724491671, 13.92634618820330061, 26.00000000000000355 ) ) ;
#37958 = CARTESIAN_POINT ( 'NONE',  ( 27.46875000122902577, -5.773502691896255534, -1.060575238724906372E-15 ) ) ;
#37959 = CARTESIAN_POINT ( 'NONE',  ( 5.446875000614518569, 6.054752690667223547, 3.707466751127219781E-16 ) ) ;
#37960 = CARTESIAN_POINT ( 'NONE',  ( 8.671875000614518214, 3.027376345333611329, 5.243569643749999010 ) ) ;
#37961 = CARTESIAN_POINT ( 'NONE',  ( 28.09687500061451360, -3.027376345333614438, 5.243569643749998122 ) ) ;
#37962 = CARTESIAN_POINT ( 'NONE',  ( -4.243569643749999898, 11.25312500061459531, 30.00000000000000000 ) ) ;
#37963 = CARTESIAN_POINT ( 'NONE',  ( 21.89999999999999858, 0.000000000000000000, 4.999999999999998224 ) ) ;
#37964 = CARTESIAN_POINT ( 'NONE',  ( 4.021830710287673583, -2.971297458697284011, 4.021830710287673583 ) ) ;
#37965 = CARTESIAN_POINT ( 'NONE',  ( 29.92500000000000071, 4.330127018922191873, 2.499999999999999556 ) ) ;
#37966 = CARTESIAN_POINT ( 'NONE',  ( 4.800000000000002487, 0.000000000000000000, 4.999999999999998224 ) ) ;
#37967 = VERTEX_POINT ( 'NONE', #51957 ) ;
#37968 = CARTESIAN_POINT ( 'NONE',  ( 18.92812500061451431, 4.541064518000418104, 2.621784821874999949 ) ) ;
#37969 = CARTESIAN_POINT ( 'NONE',  ( 11.05312500061451608, -4.541064518000417216, -2.621784821875001281 ) ) ;
#37970 = CARTESIAN_POINT ( 'NONE',  ( 20.18437500061451217, 5.492252693125287522, 3.363034840372157021E-16 ) ) ;
#37971 = CARTESIAN_POINT ( 'NONE',  ( 7.996875000614519280, -3.027376345333610441, -5.243569643749999898 ) ) ;
#37972 = CARTESIAN_POINT ( 'NONE',  ( 22.61250000000000071, 2.886751345948129099, -4.999999999999998224 ) ) ;
#37973 = CARTESIAN_POINT ( 'NONE',  ( 21.03750000122903074, 4.330127018922191873, 2.499999999999999556 ) ) ;
#37974 = CARTESIAN_POINT ( 'NONE',  ( 24.11250000000000071, 2.886751345948154857, 4.999999999999951150 ) ) ;
#37975 = CARTESIAN_POINT ( 'NONE',  ( 6.196875000614515905, -3.027376345333610441, -5.243569643749999898 ) ) ;
#37976 = CARTESIAN_POINT ( 'NONE',  ( 13.05937500061451750, 4.541064518000418104, -2.621784821874998173 ) ) ;
#37977 = CARTESIAN_POINT ( 'NONE',  ( 23.40937500061451715, 4.541064518000418104, -2.621784821874998173 ) ) ;
#37978 = VERTEX_POINT ( 'NONE', #28691 ) ;
#37979 = CARTESIAN_POINT ( 'NONE',  ( 13.61250000000000071, 2.886751345948129099, -4.999999999999998224 ) ) ;
#37980 = CARTESIAN_POINT ( 'NONE',  ( 18.64687500061451786, -3.027376345333614438, 5.243569643749998122 ) ) ;
#37981 = CARTESIAN_POINT ( 'NONE',  ( 9.534375000614517148, 4.541064518000418104, 2.621784821874999949 ) ) ;
#37982 = CARTESIAN_POINT ( 'NONE',  ( 1.878215178124997609, 15.26562499938548179, 33.25316411605952993 ) ) ;
#37983 = CARTESIAN_POINT ( 'NONE',  ( 22.08749999999999858, -2.886751345948125991, -5.000000000000000000 ) ) ;
#37984 = CARTESIAN_POINT ( 'NONE',  ( 4.000000000000000000, 15.65000000000000036, 30.00000000000000000 ) ) ;
#37985 = CARTESIAN_POINT ( 'NONE',  ( 4.243569643749999898, 10.18437500061451750, -30.00000000000000000 ) ) ;
#37986 = CARTESIAN_POINT ( 'NONE',  ( 22.09687500061451715, 5.492252693125287522, 3.363034840372157021E-16 ) ) ;
#37987 = CARTESIAN_POINT ( 'NONE',  ( 12.40312500061451573, -4.541064518000417216, -2.621784821875001281 ) ) ;
#37988 = CARTESIAN_POINT ( 'NONE',  ( 29.59687500061451715, -3.027376345333610441, -5.243569643749999898 ) ) ;
#37989 = CARTESIAN_POINT ( 'NONE',  ( 4.898587196589411843E-16, 20.00000000000000000, -26.00000000000000000 ) ) ;
#37990 = DIRECTION ( 'NONE',  ( 0.000000000000000000, 0.000000000000000000, 1.000000000000000000 ) ) ;
#37991 = CARTESIAN_POINT ( 'NONE',  ( 11.51250000000000107, 2.886751345948126879, 4.999999999999999112 ) ) ;
#37992 = EDGE_CURVE ( 'NONE', #7272, #48969, #43905, .T. ) ;
#37993 = CARTESIAN_POINT ( 'NONE',  ( -2.000000000000000000, 17.78750000122903430, 26.53589838486224650 ) ) ;
#37994 = CARTESIAN_POINT ( 'NONE',  ( 12.41250000122903430, 4.330127018922192761, -2.499999999999997780 ) ) ;
#37995 = CARTESIAN_POINT ( 'NONE',  ( 23.22187500061451715, -6.054752690667223547, -1.112240025338166033E-15 ) ) ;
#37996 = CARTESIAN_POINT ( 'NONE',  ( 17.03437500061451715, 6.421520780324663323E-16, -5.243569643749999010 ) ) ;
#37997 = DIRECTION ( 'NONE',  ( 0.000000000000000000, 0.000000000000000000, -1.000000000000000000 ) ) ;
#37998 = ORIENTED_EDGE ( 'NONE', *, *, #30313, .F. ) ;
#37999 = CARTESIAN_POINT ( 'NONE',  ( 18.36562500061451431, 3.027376345333613106, -5.243569643749998122 ) ) ;
#38000 = CARTESIAN_POINT ( 'NONE',  ( 29.55000000122903003, 5.773502691896255534, 3.535250795749688894E-16 ) ) ;
#38001 = CARTESIAN_POINT ( 'NONE',  ( 17.59687500061451715, 6.054752690667223547, 3.707466751127219781E-16 ) ) ;
#38002 = CARTESIAN_POINT ( 'NONE',  ( 3.140625000614516882, 6.054752690667223547, 3.707466751127219781E-16 ) ) ;
#38003 = CARTESIAN_POINT ( 'NONE',  ( 18.74062500061451431, -3.027376345333610441, -5.243569643749999898 ) ) ;
#38004 = CARTESIAN_POINT ( 'NONE',  ( 28.51875000122903359, 2.886751345948104674, -5.000000000000039968 ) ) ;
#38005 = CARTESIAN_POINT ( 'NONE',  ( 29.48437500061451644, -4.541064518000419881, 2.621784821874995952 ) ) ;
#38006 = CARTESIAN_POINT ( 'NONE',  ( 9.001249775931846008E-16, 12.26562500061451644, 34.90005215228797653 ) ) ;
#38007 = CARTESIAN_POINT ( 'NONE',  ( 18.08437500061451431, 4.541064518000418104, 2.621784821874999949 ) ) ;
#38008 = CARTESIAN_POINT ( 'NONE',  ( 16.68750000122903288, -4.330127018922194537, 2.499999999999995559 ) ) ;
#38009 = CARTESIAN_POINT ( 'NONE',  ( 10.47187500061451715, 2.746126346562643317, 4.756430356249998326 ) ) ;
#38010 = CARTESIAN_POINT ( 'NONE',  ( 3.366080804335946919, -3.697228694398128290, 3.718268762498968094 ) ) ;
#38011 = CARTESIAN_POINT ( 'NONE',  ( 20.33437500061451786, 4.541064518000418104, 2.621784821874999949 ) ) ;
#38012 = CARTESIAN_POINT ( 'NONE',  ( 21.60000000122903430, -2.886751345948129988, 4.999999999999997335 ) ) ;
#38013 = CARTESIAN_POINT ( 'NONE',  ( 23.39062500061451289, 6.054752690667223547, 3.707466751127219781E-16 ) ) ;
#38014 = CARTESIAN_POINT ( 'NONE',  ( 17.89687500061451431, -3.027376345333610441, -5.243569643749999898 ) ) ;
#38015 = CARTESIAN_POINT ( 'NONE',  ( 12.96562500061451750, 3.027376345333613106, -5.243569643749998122 ) ) ;
#38016 = CARTESIAN_POINT ( 'NONE',  ( -2.121784821874999949, 15.28437500061451892, 26.32496088578401938 ) ) ;
#38017 = CARTESIAN_POINT ( 'NONE',  ( 17.50312500061451715, 4.541064518000418104, -2.621784821874998173 ) ) ;
#38018 = EDGE_LOOP ( 'NONE', ( #71926, #5018, #11995, #23057 ) ) ;
#38019 = ORIENTED_EDGE ( 'NONE', *, *, #5554, .F. ) ;
#38020 = CARTESIAN_POINT ( 'NONE',  ( 22.08749999999999858, -2.886751345948125991, -5.000000000000000000 ) ) ;
#38021 = CARTESIAN_POINT ( 'NONE',  ( 2.121784821875001281, 19.10937500061451644, -26.32496088578401938 ) ) ;
#38022 = CARTESIAN_POINT ( 'NONE',  ( 12.63749999999999751, -2.886751345948193048, -4.999999999999883649 ) ) ;
#38023 = CARTESIAN_POINT ( 'NONE',  ( 25.00312500061451715, -4.541064518000417216, -2.621784821875001281 ) ) ;
#38024 = CARTESIAN_POINT ( 'NONE',  ( 6.515625000614516438, -6.054752690667223547, -1.112240025338166033E-15 ) ) ;
#38025 = CARTESIAN_POINT ( 'NONE',  ( 18.48750000122903359, -4.330127018922194537, 2.499999999999995559 ) ) ;
#38026 = CARTESIAN_POINT ( 'NONE',  ( 21.29062500061451502, -3.027376345333614438, 5.243569643749998122 ) ) ;
#38027 = CARTESIAN_POINT ( 'NONE',  ( 23.77499999999999858, -4.330127018922194537, 2.499999999999995559 ) ) ;
#38028 =( BOUNDED_CURVE ( )  B_SPLINE_CURVE ( 2, ( #54044, #36671, #25593, #3440, #70296, #19667, #25959 ),
 .UNSPECIFIED., .F., .F. ) 
 B_SPLINE_CURVE_WITH_KNOTS ( ( 3, 2, 2, 3 ),
 ( 0.9200000000000001510, 0.9233333333333334503, 0.9266666666666667496, 0.9300000000000001599 ),
 .UNSPECIFIED. ) 
 CURVE ( )  GEOMETRIC_REPRESENTATION_ITEM ( )  RATIONAL_B_SPLINE_CURVE ( ( 0.9999999999999955591, 0.8660254037844431485, 1.000000000000000000, 0.8660254037844387076, 1.000000000000000000, 0.8660254037844342667, 1.000000000000004441 ) ) 
 REPRESENTATION_ITEM ( '' )  );
#38029 = CARTESIAN_POINT ( 'NONE',  ( 25.41562500061451146, -6.054752690667223547, -1.112240025338166033E-15 ) ) ;
#38030 = CARTESIAN_POINT ( 'NONE',  ( 6.928125000614516082, -4.541064518000419881, 2.621784821874995952 ) ) ;
#38031 = VERTEX_POINT ( 'NONE', #63027 ) ;
#38032 = CARTESIAN_POINT ( 'NONE',  ( 22.64062500061451644, -3.027376345333614438, 5.243569643749998122 ) ) ;
#38033 = CARTESIAN_POINT ( 'NONE',  ( 3.890625000614517326, -3.027376345333610441, -5.243569643749999898 ) ) ;
#38034 = CARTESIAN_POINT ( 'NONE',  ( 11.29687500061451644, 5.492252693125287522, 3.363034840372157021E-16 ) ) ;
#38035 = FACE_OUTER_BOUND ( 'NONE', #17430, .T. ) ;
#38036 = CARTESIAN_POINT ( 'NONE',  ( 4.000000000000000000, 12.65000000122903501, -27.69059892324149530 ) ) ;
#38037 = CARTESIAN_POINT ( 'NONE',  ( 10.49999999999999822, 4.330127018922192761, -2.499999999999997780 ) ) ;
#38038 = CARTESIAN_POINT ( 'NONE',  ( 11.70937500061451608, 4.541064518000418104, -2.621784821874998173 ) ) ;
#38039 = CARTESIAN_POINT ( 'NONE',  ( 7.650000001229034119, -2.886751345948129988, 4.999999999999997335 ) ) ;
#38040 = CARTESIAN_POINT ( 'NONE',  ( 14.55937500061451573, 0.000000000000000000, 5.243569643749999010 ) ) ;
#38041 = CARTESIAN_POINT ( 'NONE',  ( 5.634375000614519458, -4.541064518000419881, 2.621784821874995952 ) ) ;
#38042 = CARTESIAN_POINT ( 'NONE',  ( -0.7368881354385758975, 9.803648613939515144, -34.17910028561248481 ) ) ;
#38043 = CARTESIAN_POINT ( 'NONE',  ( 11.37187500061451750, 3.027376345333611329, 5.243569643749999010 ) ) ;
#38044 = CYLINDRICAL_SURFACE ( 'NONE', #52424, 4.999999999999998224 ) ;
#38045 = CARTESIAN_POINT ( 'NONE',  ( 23.12812500061451360, -4.541064518000419881, 2.621784821874995952 ) ) ;
#38046 = CARTESIAN_POINT ( 'NONE',  ( 19.57500000000000284, 4.330127018922191873, 2.499999999999999556 ) ) ;
#38047 = CYLINDRICAL_SURFACE ( 'NONE', #66639, 4.999999999999998224 ) ;
#38048 = CARTESIAN_POINT ( 'NONE',  ( 24.60937500061451644, -4.541064518000417216, -2.621784821875001281 ) ) ;
#38049 = DIRECTION ( 'NONE',  ( -0.4999999999999975575, -0.000000000000000000, 0.8660254037844400399 ) ) ;
#38050 = CARTESIAN_POINT ( 'NONE',  ( 28.05000000122903359, -2.886751345948125991, -5.000000000000000000 ) ) ;
#38051 = EDGE_CURVE ( 'NONE', #31197, #6716, #36797, .T. ) ;
#38052 = CARTESIAN_POINT ( 'NONE',  ( 21.00937500061451857, 2.746126346562645981, -4.756430356249997438 ) ) ;
#38053 = CARTESIAN_POINT ( 'NONE',  ( 26.12812500061451360, 4.541064518000418104, 2.621784821874999949 ) ) ;
#38054 = CARTESIAN_POINT ( 'NONE',  ( 17.20312500061451644, 0.000000000000000000, 5.243569643749999010 ) ) ;
#38055 = CARTESIAN_POINT ( 'NONE',  ( 14.00625000122903252, -4.330127018922190985, -2.500000000000001332 ) ) ;
#38056 = CARTESIAN_POINT ( 'NONE',  ( 14.74687500061451573, -3.027376345333610441, -5.243569643749999898 ) ) ;
#38057 = CARTESIAN_POINT ( 'NONE',  ( 16.94999999999999929, 0.000000000000000000, 4.999999999999998224 ) ) ;
#38058 = CARTESIAN_POINT ( 'NONE',  ( 28.35000000122903430, -2.886751345948129988, 4.999999999999997335 ) ) ;
#38059 = CARTESIAN_POINT ( 'NONE',  ( 5.784375000614517148, 6.421520780324663323E-16, -5.243569643749999010 ) ) ;
#38060 = CARTESIAN_POINT ( 'NONE',  ( 17.48437500061451999, 6.421520780324663323E-16, -5.243569643749999010 ) ) ;
#38061 = CARTESIAN_POINT ( 'NONE',  ( 4.864538933187982472, -1.156167748881617108, -5.114563458357813452 ) ) ;
#38062 = CARTESIAN_POINT ( 'NONE',  ( 25.05000000000000071, 0.000000000000000000, 4.999999999999998224 ) ) ;
#38063 = CARTESIAN_POINT ( 'NONE',  ( 3.937500001229034208, 4.330127018922191873, 2.499999999999999556 ) ) ;
#38064 = CARTESIAN_POINT ( 'NONE',  ( 25.02187500061451431, -6.054752690667223547, -1.112240025338166033E-15 ) ) ;
#38065 = CARTESIAN_POINT ( 'NONE',  ( 16.09687500061452070, -3.027376345333610441, -5.243569643749999898 ) ) ;
#38066 = CARTESIAN_POINT ( 'NONE',  ( 1.878215178125000495, 12.82812499938548356, 26.74683588394047007 ) ) ;
#38067 = CARTESIAN_POINT ( 'NONE',  ( 27.67499999999999716, 4.330127018922191873, 2.499999999999999556 ) ) ;
#38068 = CARTESIAN_POINT ( 'NONE',  ( 4.912499999999999645, -5.773502691896255534, -1.060575238724906372E-15 ) ) ;
#38069 = CARTESIAN_POINT ( 'NONE',  ( 28.84687500061452070, 5.492252693125287522, 3.363034840372157021E-16 ) ) ;
#38070 = CARTESIAN_POINT ( 'NONE',  ( 19.86562500061451786, 3.027376345333611329, 5.243569643749999010 ) ) ;
#38071 = CARTESIAN_POINT ( 'NONE',  ( 10.12500000000000178, 4.330127018922191873, 2.499999999999999556 ) ) ;
#38072 = CARTESIAN_POINT ( 'NONE',  ( 3.028125000614518392, 6.421520780324663323E-16, -5.243569643749999010 ) ) ;
#38073 =( BOUNDED_CURVE ( )  B_SPLINE_CURVE ( 2, ( #18779, #35066, #40986, #12889, #23971, #35782, #6995 ),
 .UNSPECIFIED., .F., .F. ) 
 B_SPLINE_CURVE_WITH_KNOTS ( ( 3, 2, 2, 3 ),
 ( 0.3400000000000000799, 0.3433333333333333792, 0.3466666666666667895, 0.3500000000000000888 ),
 .UNSPECIFIED. ) 
 CURVE ( )  GEOMETRIC_REPRESENTATION_ITEM ( )  RATIONAL_B_SPLINE_CURVE ( ( 0.9999999999999977796, 0.8660254037844409281, 1.000000000000000000, 0.8660254037844387076, 1.000000000000000000, 0.8660254037844342667, 1.000000000000004441 ) ) 
 REPRESENTATION_ITEM ( '' )  );
#38074 = CARTESIAN_POINT ( 'NONE',  ( 18.75000000000000000, 0.000000000000000000, 4.999999999999998224 ) ) ;
#38075 = EDGE_CURVE ( 'NONE', #68271, #54526, #64165, .T. ) ;
#38076 = CARTESIAN_POINT ( 'NONE',  ( 1.071796769724495002, 16.40134618820330203, 34.00000000000000000 ) ) ;
#38077 = CARTESIAN_POINT ( 'NONE',  ( 22.23750000122903003, 6.123233995736764310E-16, -4.999999999999998224 ) ) ;
#38078 = CARTESIAN_POINT ( 'NONE',  ( 3.979525575715635810, 9.178911176227739332, 34.50663612706885175 ) ) ;
#38079 = CARTESIAN_POINT ( 'NONE',  ( 28.62187500061451573, -6.054752690667223547, -1.112240025338166033E-15 ) ) ;
#38080 = VERTEX_POINT ( 'NONE', #45696 ) ;
#38081 = CARTESIAN_POINT ( 'NONE',  ( 18.25312500061451715, -4.541064518000417216, -2.621784821875001281 ) ) ;
#38082 = CARTESIAN_POINT ( 'NONE',  ( 23.39062500061451289, 6.054752690667223547, 3.707466751127219781E-16 ) ) ;
#38083 = CARTESIAN_POINT ( 'NONE',  ( 25.95937500061451431, -4.541064518000417216, -2.621784821875001281 ) ) ;
#38084 = CARTESIAN_POINT ( 'NONE',  ( 7.350000000000002309, 4.330127018922192761, -2.499999999999997780 ) ) ;
#38085 = CARTESIAN_POINT ( 'NONE',  ( 10.97812500061451679, -4.541064518000419881, 2.621784821874995952 ) ) ;
#38086 = CARTESIAN_POINT ( 'NONE',  ( 26.27812500061451573, -4.541064518000419881, 2.621784821874995952 ) ) ;
#38087 = CARTESIAN_POINT ( 'NONE',  ( 13.69687500061451679, -3.027376345333614438, 5.243569643749998122 ) ) ;
#38088 = CARTESIAN_POINT ( 'NONE',  ( 18.90937500061451360, 4.541064518000418104, -2.621784821874998173 ) ) ;
#38089 = CARTESIAN_POINT ( 'NONE',  ( -2.121784821874999949, 18.82812500061451644, 26.32496088578401938 ) ) ;
#38090 = CARTESIAN_POINT ( 'NONE',  ( 24.37500000122903288, -5.773502691896255534, -1.060575238724906372E-15 ) ) ;
#38091 = CARTESIAN_POINT ( 'NONE',  ( 17.48437500061451999, 5.824947211148865298E-16, -4.756430356249998326 ) ) ;
#38092 = CARTESIAN_POINT ( 'NONE',  ( 14.99062500061452141, -3.027376345333614438, 5.243569643749998122 ) ) ;
#38093 = CARTESIAN_POINT ( 'NONE',  ( 7.771875000614516971, 3.027376345333611329, 5.243569643749999010 ) ) ;
#38094 = CARTESIAN_POINT ( 'NONE',  ( 7.996875000614519280, -3.027376345333610441, -5.243569643749999898 ) ) ;
#38095 = EDGE_CURVE ( 'NONE', #33889, #46701, #8881, .T. ) ;
#38096 = VERTEX_POINT ( 'NONE', #29062 ) ;
#38097 = CARTESIAN_POINT ( 'NONE',  ( 28.35937500061451289, 4.541064518000418104, -2.621784821874998173 ) ) ;
#38098 = CARTESIAN_POINT ( 'NONE',  ( 19.22812500061451502, 6.421520780324663323E-16, -5.243569643749999010 ) ) ;
#38099 = CARTESIAN_POINT ( 'NONE',  ( 29.10000000122903074, 5.773502691896255534, 3.535250795749688894E-16 ) ) ;
#38100 = CARTESIAN_POINT ( 'NONE',  ( 3.009375000614516793, -4.541064518000417216, -2.621784821875001281 ) ) ;
#38101 = CARTESIAN_POINT ( 'NONE',  ( 24.38437500061451502, 4.541064518000418104, 2.621784821874999949 ) ) ;
#38102 = CARTESIAN_POINT ( 'NONE',  ( 20.35312500061451502, 0.000000000000000000, 5.243569643749999010 ) ) ;
#38103 = CARTESIAN_POINT ( 'NONE',  ( -3.999999999999999556, 12.76250000000000284, 27.69059892324149530 ) ) ;
#38104 = CARTESIAN_POINT ( 'NONE',  ( 25.22812500061451502, 4.541064518000418104, 2.621784821874999949 ) ) ;
#38105 = CARTESIAN_POINT ( 'NONE',  ( 6.337500001229033231, -4.330127018922194537, 2.499999999999995559 ) ) ;
#38106 = ORIENTED_EDGE ( 'NONE', *, *, #42868, .F. ) ;
#38107 = FACE_OUTER_BOUND ( 'NONE', #53269, .T. ) ;
#38108 = CARTESIAN_POINT ( 'NONE',  ( -3.999999999999997335, 15.08750000000000036, -27.69059892324149175 ) ) ;
#38109 = CARTESIAN_POINT ( 'NONE',  ( 22.53750000122903430, -4.330127018922194537, 2.499999999999995559 ) ) ;
#38110 = CARTESIAN_POINT ( 'NONE',  ( -1.878215178124999163, 15.15312499938548285, 26.74683588394047007 ) ) ;
#38111 = CARTESIAN_POINT ( 'NONE',  ( 4.921875000614518214, 3.027376345333613106, -5.243569643749998122 ) ) ;
#38112 = CARTESIAN_POINT ( 'NONE',  ( 25.38749999999999929, 5.773502691896255534, 3.535250795749688401E-16 ) ) ;
#38113 = CARTESIAN_POINT ( 'NONE',  ( 11.99062500061451608, -3.027376345333610441, -5.243569643749999898 ) ) ;
#38114 = CARTESIAN_POINT ( 'NONE',  ( 5.784375000614517148, 6.421520780324663323E-16, -5.243569643749999010 ) ) ;
#38115 = CARTESIAN_POINT ( 'NONE',  ( 23.43750000122902932, -4.330127018922194537, 2.499999999999995559 ) ) ;
#38116 = CARTESIAN_POINT ( 'NONE',  ( 15.64687500061451608, -3.027376345333610441, -5.243569643749999898 ) ) ;
#38117 = CARTESIAN_POINT ( 'NONE',  ( 3.346875000614518036, -3.027376345333614438, 5.243569643749998122 ) ) ;
#38118 = CARTESIAN_POINT ( 'NONE',  ( 8.062500001229034652, 0.000000000000000000, 4.999999999999998224 ) ) ;
#38119 = CARTESIAN_POINT ( 'NONE',  ( 5.015625000614518214, 3.027376345333611329, 5.243569643749999010 ) ) ;
#38120 = CARTESIAN_POINT ( 'NONE',  ( 15.44062500061451537, -3.027376345333614438, 5.243569643749998122 ) ) ;
#38121 = VERTEX_POINT ( 'NONE', #22777 ) ;
#38122 = CARTESIAN_POINT ( 'NONE',  ( 9.290625000614515017, -3.027376345333610441, -5.243569643749999898 ) ) ;
#38123 = CARTESIAN_POINT ( 'NONE',  ( 7.903125000614515727, -4.541064518000417216, -2.621784821875001281 ) ) ;
#38124 = CARTESIAN_POINT ( 'NONE',  ( 18.49687500061452283, 5.492252693125287522, 3.363034840372157021E-16 ) ) ;
#38125 = CARTESIAN_POINT ( 'NONE',  ( 8.099999999999999645, -4.330127018922190985, -2.500000000000001332 ) ) ;
#38126 = CARTESIAN_POINT ( 'NONE',  ( 4.087500001229035007, -4.330127018922194537, 2.499999999999995559 ) ) ;
#38127 = CARTESIAN_POINT ( 'NONE',  ( 18.11250000000000071, 2.886751345948129099, -4.999999999999998224 ) ) ;
#38128 = CARTESIAN_POINT ( 'NONE',  ( 17.37187500061451573, -6.054752690667223547, -1.112240025338166033E-15 ) ) ;
#38129 = CARTESIAN_POINT ( 'NONE',  ( 12.90000000122903145, 5.773502691896255534, 3.535250795749688894E-16 ) ) ;
#38130 = CARTESIAN_POINT ( 'NONE',  ( 21.75000000000000000, 4.330127018922192761, -2.499999999999997780 ) ) ;
#38131 = CARTESIAN_POINT ( 'NONE',  ( 2.121784821874999061, 16.95312500061451999, -33.67503911421598417 ) ) ;
#38132 = LINE ( 'NONE', #37769, #5315 ) ;
#38133 = CARTESIAN_POINT ( 'NONE',  ( 5.000000000000000000, 39.99999999999999289, 30.00000000000000000 ) ) ;
#38134 = FACE_OUTER_BOUND ( 'NONE', #44781, .T. ) ;
#38135 = CARTESIAN_POINT ( 'NONE',  ( 20.10000000122903074, 5.773502691896255534, 3.535250795749688401E-16 ) ) ;
#38136 = CARTESIAN_POINT ( 'NONE',  ( 1.999999999999998668, 16.25000000000000000, -33.46410161513775705 ) ) ;
#38137 = CARTESIAN_POINT ( 'NONE',  ( 14.74687500061451573, -3.027376345333610441, -5.243569643749999898 ) ) ;
#38138 = CARTESIAN_POINT ( 'NONE',  ( 27.26249999999999929, 2.886751345948126879, 4.999999999999999112 ) ) ;
#38139 = CARTESIAN_POINT ( 'NONE',  ( 12.59062500061451573, 6.054752690667223547, 3.707466751127219781E-16 ) ) ;
#38140 = CARTESIAN_POINT ( 'NONE',  ( 26.52187500061451431, 4.119189519843966529, 2.378215178124999607 ) ) ;
#38141 = CARTESIAN_POINT ( 'NONE',  ( 21.83437500061451786, -4.541064518000419881, 2.621784821874995952 ) ) ;
#38142 = CARTESIAN_POINT ( 'NONE',  ( 13.17187500061451466, -4.119189519843968306, 2.378215178124996054 ) ) ;
#38143 = CARTESIAN_POINT ( 'NONE',  ( 7.865625000614516971, -6.054752690667223547, -1.112240025338166033E-15 ) ) ;
#38144 = CARTESIAN_POINT ( 'NONE',  ( 13.39687500061451608, -3.027376345333610441, -5.243569643749999898 ) ) ;
#38145 = ORIENTED_EDGE ( 'NONE', *, *, #24790, .F. ) ;
#38146 = CARTESIAN_POINT ( 'NONE',  ( 22.80937500061451573, -4.541064518000417216, -2.621784821875001281 ) ) ;
#38147 = CARTESIAN_POINT ( 'NONE',  ( 29.02499999999999858, 4.330127018922191873, 2.499999999999999556 ) ) ;
#38148 = ADVANCED_FACE ( 'NONE', ( #51598 ), #28331, .T. ) ;
#38149 = CARTESIAN_POINT ( 'NONE',  ( 8.775000000000002132, 4.330127018922191873, 2.499999999999999556 ) ) ;
#38150 = CARTESIAN_POINT ( 'NONE',  ( 5.700000000000000178, 0.000000000000000000, 4.999999999999998224 ) ) ;
#38151 = CARTESIAN_POINT ( 'NONE',  ( 16.72500000122903430, -5.773502691896255534, -1.060575238724906372E-15 ) ) ;
#38152 = CARTESIAN_POINT ( 'NONE',  ( 30.00000000000000000, 0.000000000000000000, 9.999999999999998224 ) ) ;
#38153 = CARTESIAN_POINT ( 'NONE',  ( 17.39999999999999858, 0.000000000000000000, 4.999999999999998224 ) ) ;
#38154 = ORIENTED_EDGE ( 'NONE', *, *, #61508, .T. ) ;
